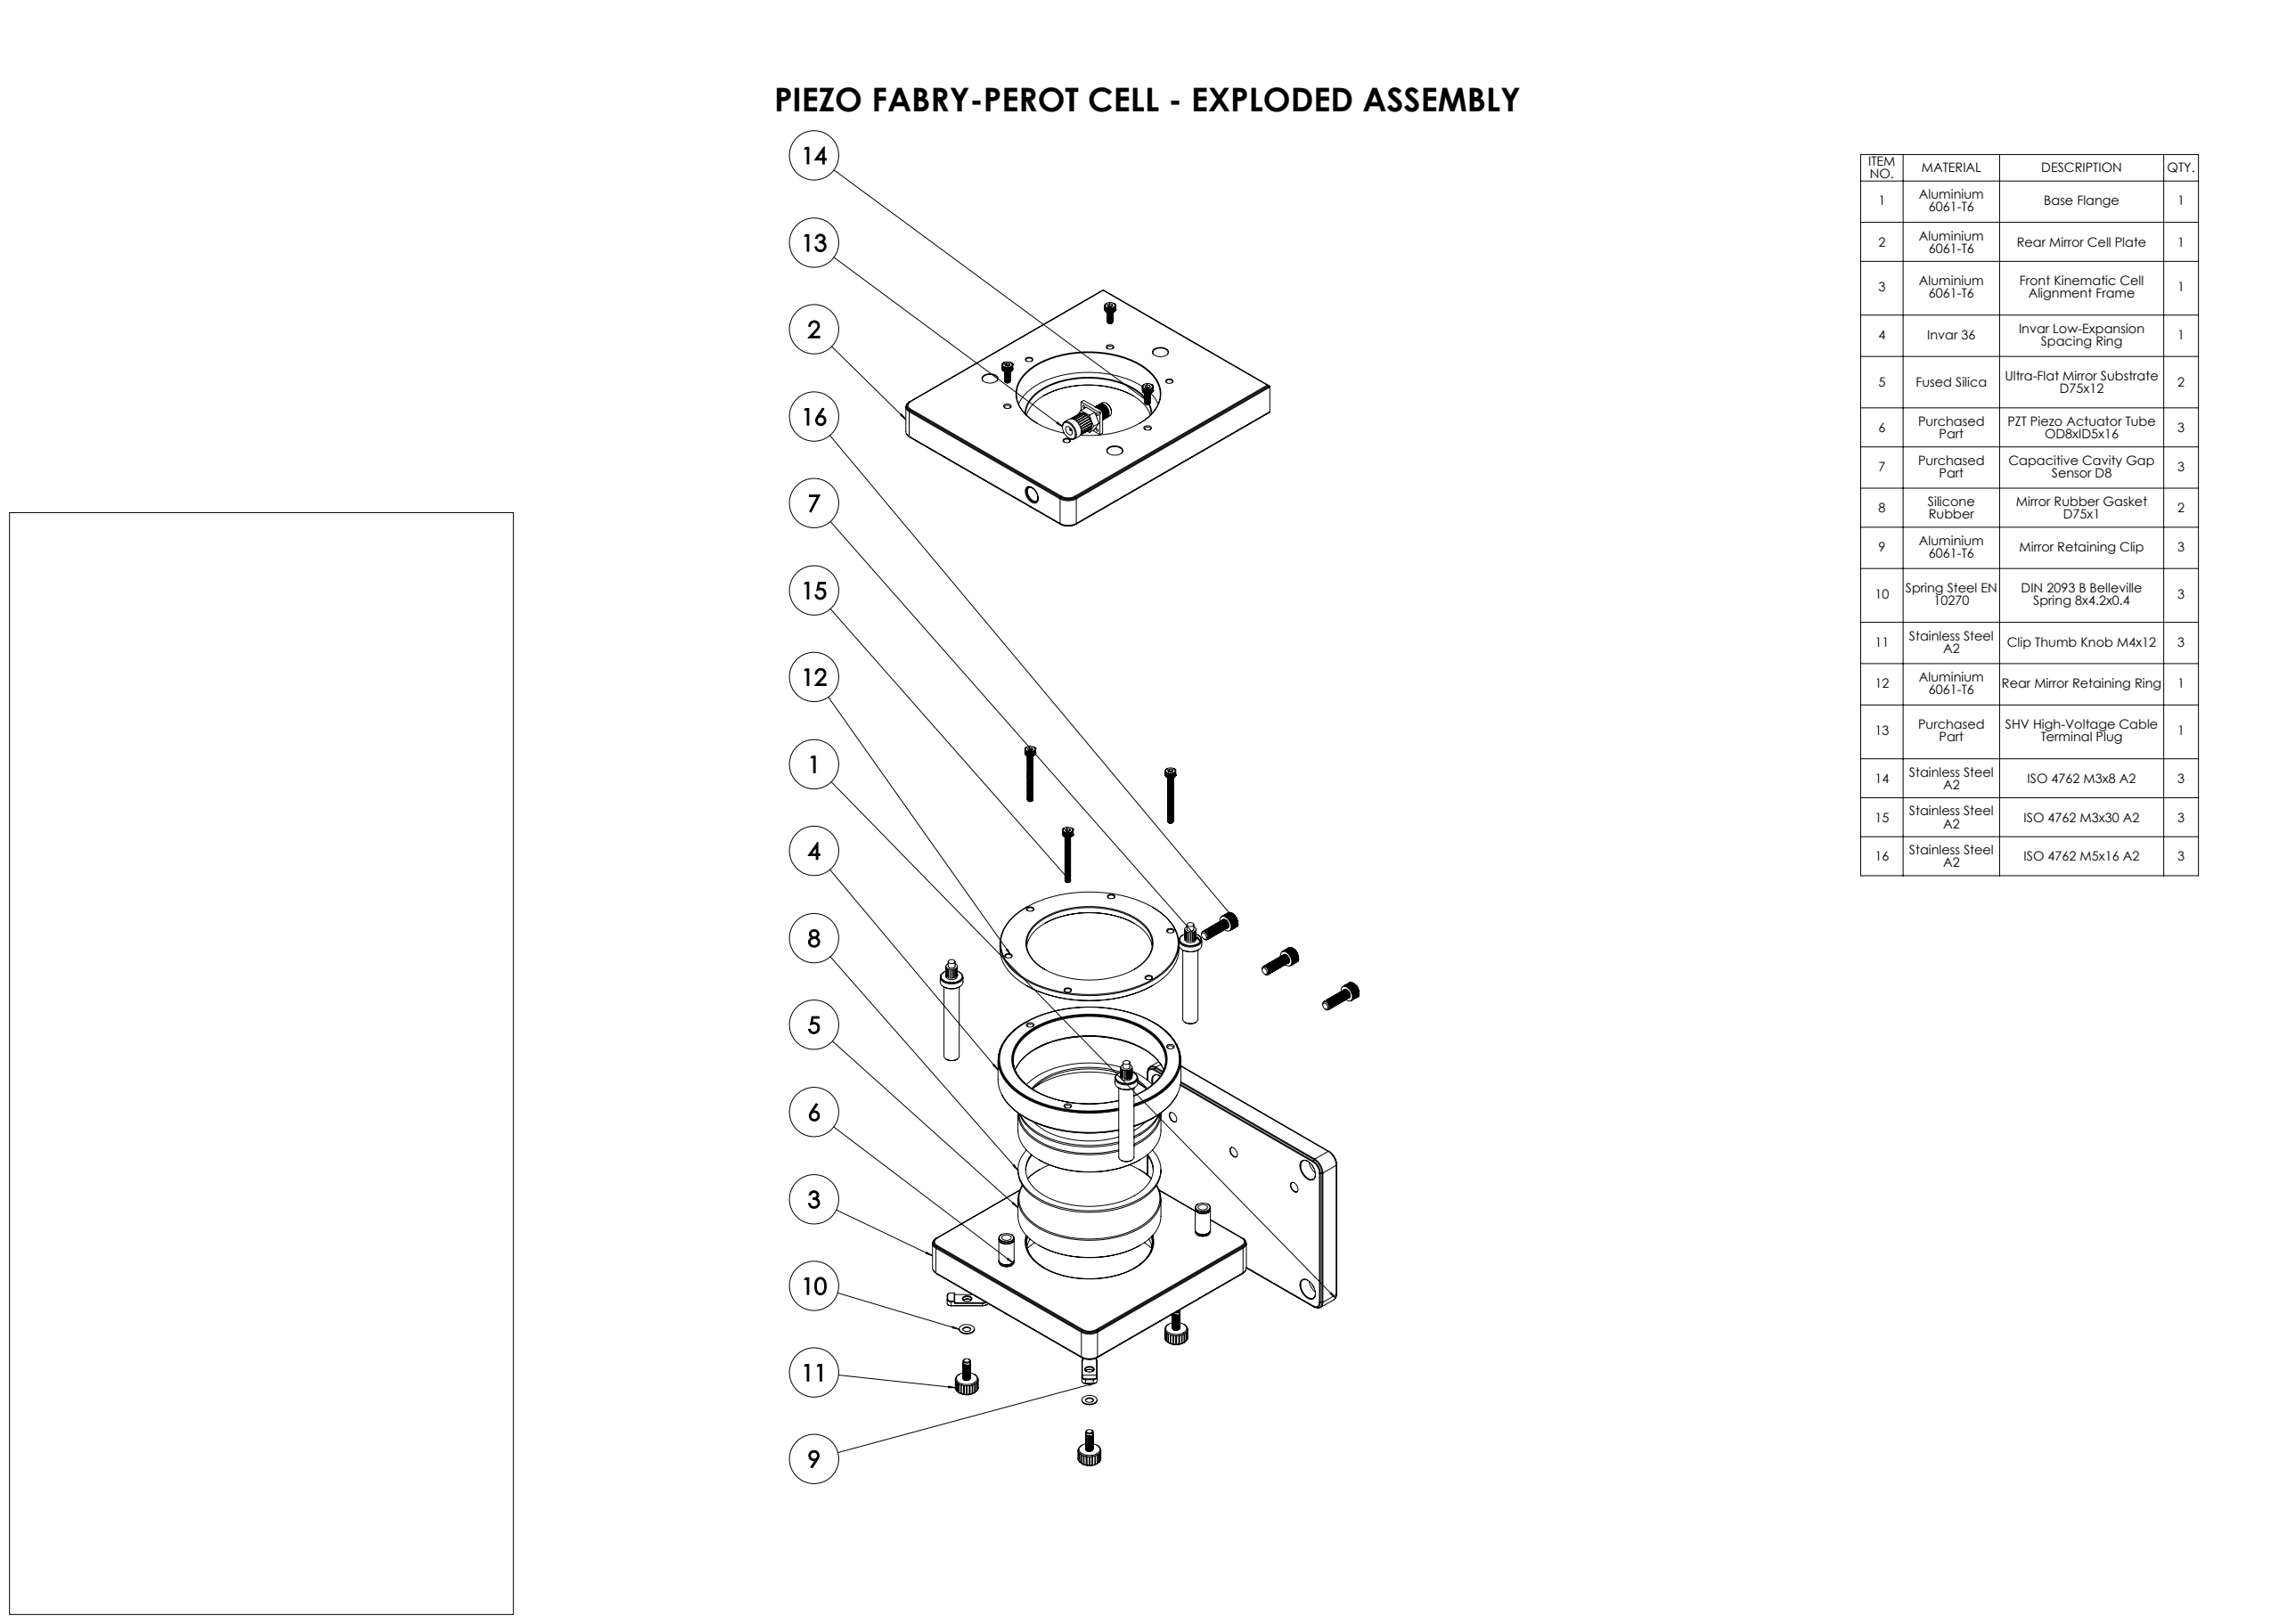
ISO-10303-21;
HEADER;
/* Generated by software containing ST-Developer
 * from STEP Tools, Inc. (www.steptools.com) 
 */

FILE_DESCRIPTION(
/* description */ (''),
/* implementation_level */ '2;1');

FILE_NAME(
/* name */ 'MAS-298',
/* time_stamp */ '2026-10-19T22:59:19-07:00',
/* author */ (''),
/* organization */ (''),
/* preprocessor_version */ 'ST-DEVELOPER v20.2',
/* originating_system */ 'Autodesk Translation Framework v15.15.0.0',
/* authorisation */ '');

FILE_SCHEMA (('AUTOMOTIVE_DESIGN { 1 0 10303 214 3 1 1 }'));
ENDSEC;

DATA;
#10=MECHANICAL_DESIGN_GEOMETRIC_PRESENTATION_REPRESENTATION('',(#911,#912,
#913,#914,#915,#916,#917,#918,#919,#920,#921,#922,#923,#924,#925,#926),
#53650);
#11=ITEM_DEFINED_TRANSFORMATION($,$,#23497,#25620);
#12=ITEM_DEFINED_TRANSFORMATION($,$,#23686,#25621);
#13=ITEM_DEFINED_TRANSFORMATION($,$,#23856,#25622);
#14=ITEM_DEFINED_TRANSFORMATION($,$,#23983,#25623);
#15=ITEM_DEFINED_TRANSFORMATION($,$,#24331,#25624);
#16=ITEM_DEFINED_TRANSFORMATION($,$,#24343,#25625);
#17=ITEM_DEFINED_TRANSFORMATION($,$,#24374,#25626);
#18=ITEM_DEFINED_TRANSFORMATION($,$,#24521,#25627);
#19=ITEM_DEFINED_TRANSFORMATION($,$,#24530,#25628);
#20=ITEM_DEFINED_TRANSFORMATION($,$,#24586,#25629);
#21=ITEM_DEFINED_TRANSFORMATION($,$,#24595,#25630);
#22=ITEM_DEFINED_TRANSFORMATION($,$,#24038,#25631);
#23=ITEM_DEFINED_TRANSFORMATION($,$,#24107,#25632);
#24=ITEM_DEFINED_TRANSFORMATION($,$,#24795,#25633);
#25=ITEM_DEFINED_TRANSFORMATION($,$,#25038,#25634);
#26=ITEM_DEFINED_TRANSFORMATION($,$,#25369,#25635);
#27=ITEM_DEFINED_TRANSFORMATION($,$,#24331,#25636);
#28=ITEM_DEFINED_TRANSFORMATION($,$,#24343,#25637);
#29=ITEM_DEFINED_TRANSFORMATION($,$,#24343,#25638);
#30=ITEM_DEFINED_TRANSFORMATION($,$,#24374,#25639);
#31=ITEM_DEFINED_TRANSFORMATION($,$,#24374,#25640);
#32=ITEM_DEFINED_TRANSFORMATION($,$,#24521,#25641);
#33=ITEM_DEFINED_TRANSFORMATION($,$,#24530,#25642);
#34=ITEM_DEFINED_TRANSFORMATION($,$,#24530,#25643);
#35=ITEM_DEFINED_TRANSFORMATION($,$,#24586,#25644);
#36=ITEM_DEFINED_TRANSFORMATION($,$,#24586,#25645);
#37=ITEM_DEFINED_TRANSFORMATION($,$,#24595,#25646);
#38=ITEM_DEFINED_TRANSFORMATION($,$,#24595,#25647);
#39=ITEM_DEFINED_TRANSFORMATION($,$,#24795,#25648);
#40=ITEM_DEFINED_TRANSFORMATION($,$,#24795,#25649);
#41=ITEM_DEFINED_TRANSFORMATION($,$,#25038,#25650);
#42=ITEM_DEFINED_TRANSFORMATION($,$,#25038,#25651);
#43=ITEM_DEFINED_TRANSFORMATION($,$,#25369,#25652);
#44=ITEM_DEFINED_TRANSFORMATION($,$,#25369,#25653);
#45=(
REPRESENTATION_RELATIONSHIP($,$,#53724,#53723)
REPRESENTATION_RELATIONSHIP_WITH_TRANSFORMATION(#11)
SHAPE_REPRESENTATION_RELATIONSHIP()
);
#46=(
REPRESENTATION_RELATIONSHIP($,$,#53725,#53723)
REPRESENTATION_RELATIONSHIP_WITH_TRANSFORMATION(#12)
SHAPE_REPRESENTATION_RELATIONSHIP()
);
#47=(
REPRESENTATION_RELATIONSHIP($,$,#53726,#53723)
REPRESENTATION_RELATIONSHIP_WITH_TRANSFORMATION(#13)
SHAPE_REPRESENTATION_RELATIONSHIP()
);
#48=(
REPRESENTATION_RELATIONSHIP($,$,#53727,#53723)
REPRESENTATION_RELATIONSHIP_WITH_TRANSFORMATION(#14)
SHAPE_REPRESENTATION_RELATIONSHIP()
);
#49=(
REPRESENTATION_RELATIONSHIP($,$,#53730,#53723)
REPRESENTATION_RELATIONSHIP_WITH_TRANSFORMATION(#15)
SHAPE_REPRESENTATION_RELATIONSHIP()
);
#50=(
REPRESENTATION_RELATIONSHIP($,$,#53731,#53723)
REPRESENTATION_RELATIONSHIP_WITH_TRANSFORMATION(#16)
SHAPE_REPRESENTATION_RELATIONSHIP()
);
#51=(
REPRESENTATION_RELATIONSHIP($,$,#53732,#53723)
REPRESENTATION_RELATIONSHIP_WITH_TRANSFORMATION(#17)
SHAPE_REPRESENTATION_RELATIONSHIP()
);
#52=(
REPRESENTATION_RELATIONSHIP($,$,#53733,#53723)
REPRESENTATION_RELATIONSHIP_WITH_TRANSFORMATION(#18)
SHAPE_REPRESENTATION_RELATIONSHIP()
);
#53=(
REPRESENTATION_RELATIONSHIP($,$,#53734,#53723)
REPRESENTATION_RELATIONSHIP_WITH_TRANSFORMATION(#19)
SHAPE_REPRESENTATION_RELATIONSHIP()
);
#54=(
REPRESENTATION_RELATIONSHIP($,$,#53735,#53723)
REPRESENTATION_RELATIONSHIP_WITH_TRANSFORMATION(#20)
SHAPE_REPRESENTATION_RELATIONSHIP()
);
#55=(
REPRESENTATION_RELATIONSHIP($,$,#53736,#53723)
REPRESENTATION_RELATIONSHIP_WITH_TRANSFORMATION(#21)
SHAPE_REPRESENTATION_RELATIONSHIP()
);
#56=(
REPRESENTATION_RELATIONSHIP($,$,#53728,#53723)
REPRESENTATION_RELATIONSHIP_WITH_TRANSFORMATION(#22)
SHAPE_REPRESENTATION_RELATIONSHIP()
);
#57=(
REPRESENTATION_RELATIONSHIP($,$,#53729,#53723)
REPRESENTATION_RELATIONSHIP_WITH_TRANSFORMATION(#23)
SHAPE_REPRESENTATION_RELATIONSHIP()
);
#58=(
REPRESENTATION_RELATIONSHIP($,$,#53737,#53723)
REPRESENTATION_RELATIONSHIP_WITH_TRANSFORMATION(#24)
SHAPE_REPRESENTATION_RELATIONSHIP()
);
#59=(
REPRESENTATION_RELATIONSHIP($,$,#53738,#53723)
REPRESENTATION_RELATIONSHIP_WITH_TRANSFORMATION(#25)
SHAPE_REPRESENTATION_RELATIONSHIP()
);
#60=(
REPRESENTATION_RELATIONSHIP($,$,#53739,#53723)
REPRESENTATION_RELATIONSHIP_WITH_TRANSFORMATION(#26)
SHAPE_REPRESENTATION_RELATIONSHIP()
);
#61=(
REPRESENTATION_RELATIONSHIP($,$,#53730,#53723)
REPRESENTATION_RELATIONSHIP_WITH_TRANSFORMATION(#27)
SHAPE_REPRESENTATION_RELATIONSHIP()
);
#62=(
REPRESENTATION_RELATIONSHIP($,$,#53731,#53723)
REPRESENTATION_RELATIONSHIP_WITH_TRANSFORMATION(#28)
SHAPE_REPRESENTATION_RELATIONSHIP()
);
#63=(
REPRESENTATION_RELATIONSHIP($,$,#53731,#53723)
REPRESENTATION_RELATIONSHIP_WITH_TRANSFORMATION(#29)
SHAPE_REPRESENTATION_RELATIONSHIP()
);
#64=(
REPRESENTATION_RELATIONSHIP($,$,#53732,#53723)
REPRESENTATION_RELATIONSHIP_WITH_TRANSFORMATION(#30)
SHAPE_REPRESENTATION_RELATIONSHIP()
);
#65=(
REPRESENTATION_RELATIONSHIP($,$,#53732,#53723)
REPRESENTATION_RELATIONSHIP_WITH_TRANSFORMATION(#31)
SHAPE_REPRESENTATION_RELATIONSHIP()
);
#66=(
REPRESENTATION_RELATIONSHIP($,$,#53733,#53723)
REPRESENTATION_RELATIONSHIP_WITH_TRANSFORMATION(#32)
SHAPE_REPRESENTATION_RELATIONSHIP()
);
#67=(
REPRESENTATION_RELATIONSHIP($,$,#53734,#53723)
REPRESENTATION_RELATIONSHIP_WITH_TRANSFORMATION(#33)
SHAPE_REPRESENTATION_RELATIONSHIP()
);
#68=(
REPRESENTATION_RELATIONSHIP($,$,#53734,#53723)
REPRESENTATION_RELATIONSHIP_WITH_TRANSFORMATION(#34)
SHAPE_REPRESENTATION_RELATIONSHIP()
);
#69=(
REPRESENTATION_RELATIONSHIP($,$,#53735,#53723)
REPRESENTATION_RELATIONSHIP_WITH_TRANSFORMATION(#35)
SHAPE_REPRESENTATION_RELATIONSHIP()
);
#70=(
REPRESENTATION_RELATIONSHIP($,$,#53735,#53723)
REPRESENTATION_RELATIONSHIP_WITH_TRANSFORMATION(#36)
SHAPE_REPRESENTATION_RELATIONSHIP()
);
#71=(
REPRESENTATION_RELATIONSHIP($,$,#53736,#53723)
REPRESENTATION_RELATIONSHIP_WITH_TRANSFORMATION(#37)
SHAPE_REPRESENTATION_RELATIONSHIP()
);
#72=(
REPRESENTATION_RELATIONSHIP($,$,#53736,#53723)
REPRESENTATION_RELATIONSHIP_WITH_TRANSFORMATION(#38)
SHAPE_REPRESENTATION_RELATIONSHIP()
);
#73=(
REPRESENTATION_RELATIONSHIP($,$,#53737,#53723)
REPRESENTATION_RELATIONSHIP_WITH_TRANSFORMATION(#39)
SHAPE_REPRESENTATION_RELATIONSHIP()
);
#74=(
REPRESENTATION_RELATIONSHIP($,$,#53737,#53723)
REPRESENTATION_RELATIONSHIP_WITH_TRANSFORMATION(#40)
SHAPE_REPRESENTATION_RELATIONSHIP()
);
#75=(
REPRESENTATION_RELATIONSHIP($,$,#53738,#53723)
REPRESENTATION_RELATIONSHIP_WITH_TRANSFORMATION(#41)
SHAPE_REPRESENTATION_RELATIONSHIP()
);
#76=(
REPRESENTATION_RELATIONSHIP($,$,#53738,#53723)
REPRESENTATION_RELATIONSHIP_WITH_TRANSFORMATION(#42)
SHAPE_REPRESENTATION_RELATIONSHIP()
);
#77=(
REPRESENTATION_RELATIONSHIP($,$,#53739,#53723)
REPRESENTATION_RELATIONSHIP_WITH_TRANSFORMATION(#43)
SHAPE_REPRESENTATION_RELATIONSHIP()
);
#78=(
REPRESENTATION_RELATIONSHIP($,$,#53739,#53723)
REPRESENTATION_RELATIONSHIP_WITH_TRANSFORMATION(#44)
SHAPE_REPRESENTATION_RELATIONSHIP()
);
#79=CONTEXT_DEPENDENT_SHAPE_REPRESENTATION(#45,#53689);
#80=CONTEXT_DEPENDENT_SHAPE_REPRESENTATION(#46,#53690);
#81=CONTEXT_DEPENDENT_SHAPE_REPRESENTATION(#47,#53691);
#82=CONTEXT_DEPENDENT_SHAPE_REPRESENTATION(#48,#53692);
#83=CONTEXT_DEPENDENT_SHAPE_REPRESENTATION(#49,#53693);
#84=CONTEXT_DEPENDENT_SHAPE_REPRESENTATION(#50,#53694);
#85=CONTEXT_DEPENDENT_SHAPE_REPRESENTATION(#51,#53695);
#86=CONTEXT_DEPENDENT_SHAPE_REPRESENTATION(#52,#53696);
#87=CONTEXT_DEPENDENT_SHAPE_REPRESENTATION(#53,#53697);
#88=CONTEXT_DEPENDENT_SHAPE_REPRESENTATION(#54,#53698);
#89=CONTEXT_DEPENDENT_SHAPE_REPRESENTATION(#55,#53699);
#90=CONTEXT_DEPENDENT_SHAPE_REPRESENTATION(#56,#53700);
#91=CONTEXT_DEPENDENT_SHAPE_REPRESENTATION(#57,#53701);
#92=CONTEXT_DEPENDENT_SHAPE_REPRESENTATION(#58,#53702);
#93=CONTEXT_DEPENDENT_SHAPE_REPRESENTATION(#59,#53703);
#94=CONTEXT_DEPENDENT_SHAPE_REPRESENTATION(#60,#53704);
#95=CONTEXT_DEPENDENT_SHAPE_REPRESENTATION(#61,#53705);
#96=CONTEXT_DEPENDENT_SHAPE_REPRESENTATION(#62,#53706);
#97=CONTEXT_DEPENDENT_SHAPE_REPRESENTATION(#63,#53707);
#98=CONTEXT_DEPENDENT_SHAPE_REPRESENTATION(#64,#53708);
#99=CONTEXT_DEPENDENT_SHAPE_REPRESENTATION(#65,#53709);
#100=CONTEXT_DEPENDENT_SHAPE_REPRESENTATION(#66,#53710);
#101=CONTEXT_DEPENDENT_SHAPE_REPRESENTATION(#67,#53711);
#102=CONTEXT_DEPENDENT_SHAPE_REPRESENTATION(#68,#53712);
#103=CONTEXT_DEPENDENT_SHAPE_REPRESENTATION(#69,#53713);
#104=CONTEXT_DEPENDENT_SHAPE_REPRESENTATION(#70,#53714);
#105=CONTEXT_DEPENDENT_SHAPE_REPRESENTATION(#71,#53715);
#106=CONTEXT_DEPENDENT_SHAPE_REPRESENTATION(#72,#53716);
#107=CONTEXT_DEPENDENT_SHAPE_REPRESENTATION(#73,#53717);
#108=CONTEXT_DEPENDENT_SHAPE_REPRESENTATION(#74,#53718);
#109=CONTEXT_DEPENDENT_SHAPE_REPRESENTATION(#75,#53719);
#110=CONTEXT_DEPENDENT_SHAPE_REPRESENTATION(#76,#53720);
#111=CONTEXT_DEPENDENT_SHAPE_REPRESENTATION(#77,#53721);
#112=CONTEXT_DEPENDENT_SHAPE_REPRESENTATION(#78,#53722);
#113=NEXT_ASSEMBLY_USAGE_OCCURRENCE('01_Base_Flange:1',
'01_Base_Flange:1','01_Base_Flange:1',#53741,#53742,'01_Base_Flange:1');
#114=NEXT_ASSEMBLY_USAGE_OCCURRENCE('02_Rear_Mirror_Cell_Plate:1',
'02_Rear_Mirror_Cell_Plate:1','02_Rear_Mirror_Cell_Plate:1',#53741,#53743,
'02_Rear_Mirror_Cell_Plate:1');
#115=NEXT_ASSEMBLY_USAGE_OCCURRENCE(
'03_Front_Kinematic_Cell_Alignment_Frame:1',
'03_Front_Kinematic_Cell_Alignment_Frame:1',
'03_Front_Kinematic_Cell_Alignment_Frame:1',#53741,#53744,
'03_Front_Kinematic_Cell_Alignment_Frame:1');
#116=NEXT_ASSEMBLY_USAGE_OCCURRENCE(
'04_Invar_Low-Expansion_Spacing_Ring:1',
'04_Invar_Low-Expansion_Spacing_Ring:1',
'04_Invar_Low-Expansion_Spacing_Ring:1',#53741,#53745,
'04_Invar_Low-Expansion_Spacing_Ring:1');
#117=NEXT_ASSEMBLY_USAGE_OCCURRENCE(
'05_Ultra-Flat_Mirror_Substrate_D75x12:1',
'05_Ultra-Flat_Mirror_Substrate_D75x12:1',
'05_Ultra-Flat_Mirror_Substrate_D75x12:1',#53741,#53748,
'05_Ultra-Flat_Mirror_Substrate_D75x12:1');
#118=NEXT_ASSEMBLY_USAGE_OCCURRENCE(
'06_PZT_Piezo_Actuator_Tube_OD8xID5x16:1',
'06_PZT_Piezo_Actuator_Tube_OD8xID5x16:1',
'06_PZT_Piezo_Actuator_Tube_OD8xID5x16:1',#53741,#53749,
'06_PZT_Piezo_Actuator_Tube_OD8xID5x16:1');
#119=NEXT_ASSEMBLY_USAGE_OCCURRENCE(
'07_Capacitive_Cavity_Gap_Sensor_D8:1',
'07_Capacitive_Cavity_Gap_Sensor_D8:1',
'07_Capacitive_Cavity_Gap_Sensor_D8:1',#53741,#53750,
'07_Capacitive_Cavity_Gap_Sensor_D8:1');
#120=NEXT_ASSEMBLY_USAGE_OCCURRENCE('08_Mirror_Rubber_Gasket_D75x1:1',
'08_Mirror_Rubber_Gasket_D75x1:1','08_Mirror_Rubber_Gasket_D75x1:1',#53741,
#53751,'08_Mirror_Rubber_Gasket_D75x1:1');
#121=NEXT_ASSEMBLY_USAGE_OCCURRENCE('09_Mirror_Retaining_Clip:1',
'09_Mirror_Retaining_Clip:1','09_Mirror_Retaining_Clip:1',#53741,#53752,
'09_Mirror_Retaining_Clip:1');
#122=NEXT_ASSEMBLY_USAGE_OCCURRENCE(
'10_DIN_2093_B_Belleville_Spring_8x4.2x0.4:1',
'10_DIN_2093_B_Belleville_Spring_8x4.2x0.4:1',
'10_DIN_2093_B_Belleville_Spring_8x4.2x0.4:1',#53741,#53753,
'10_DIN_2093_B_Belleville_Spring_8x4.2x0.4:1');
#123=NEXT_ASSEMBLY_USAGE_OCCURRENCE('11_Clip_Thumb_Knob_M4x12:1',
'11_Clip_Thumb_Knob_M4x12:1','11_Clip_Thumb_Knob_M4x12:1',#53741,#53754,
'11_Clip_Thumb_Knob_M4x12:1');
#124=NEXT_ASSEMBLY_USAGE_OCCURRENCE('12_Rear_Mirror_Retaining_Ring:1',
'12_Rear_Mirror_Retaining_Ring:1','12_Rear_Mirror_Retaining_Ring:1',#53741,
#53746,'12_Rear_Mirror_Retaining_Ring:1');
#125=NEXT_ASSEMBLY_USAGE_OCCURRENCE(
'13_SHV_High-Voltage_Cable_Terminal_Plug:1',
'13_SHV_High-Voltage_Cable_Terminal_Plug:1',
'13_SHV_High-Voltage_Cable_Terminal_Plug:1',#53741,#53747,
'13_SHV_High-Voltage_Cable_Terminal_Plug:1');
#126=NEXT_ASSEMBLY_USAGE_OCCURRENCE('14_ISO_4762_M3x8_A2:1',
'14_ISO_4762_M3x8_A2:1','14_ISO_4762_M3x8_A2:1',#53741,#53755,
'14_ISO_4762_M3x8_A2:1');
#127=NEXT_ASSEMBLY_USAGE_OCCURRENCE('15_ISO_4762_M3x30_A2:1',
'15_ISO_4762_M3x30_A2:1','15_ISO_4762_M3x30_A2:1',#53741,#53756,
'15_ISO_4762_M3x30_A2:1');
#128=NEXT_ASSEMBLY_USAGE_OCCURRENCE('16_ISO_4762_M5x16_A2:1',
'16_ISO_4762_M5x16_A2:1','16_ISO_4762_M5x16_A2:1',#53741,#53757,
'16_ISO_4762_M5x16_A2:1');
#129=NEXT_ASSEMBLY_USAGE_OCCURRENCE(
'05_Ultra-Flat_Mirror_Substrate_D75x12:2',
'05_Ultra-Flat_Mirror_Substrate_D75x12:2',
'05_Ultra-Flat_Mirror_Substrate_D75x12:2',#53741,#53748,
'05_Ultra-Flat_Mirror_Substrate_D75x12:2');
#130=NEXT_ASSEMBLY_USAGE_OCCURRENCE(
'06_PZT_Piezo_Actuator_Tube_OD8xID5x16:2',
'06_PZT_Piezo_Actuator_Tube_OD8xID5x16:2',
'06_PZT_Piezo_Actuator_Tube_OD8xID5x16:2',#53741,#53749,
'06_PZT_Piezo_Actuator_Tube_OD8xID5x16:2');
#131=NEXT_ASSEMBLY_USAGE_OCCURRENCE(
'06_PZT_Piezo_Actuator_Tube_OD8xID5x16:3',
'06_PZT_Piezo_Actuator_Tube_OD8xID5x16:3',
'06_PZT_Piezo_Actuator_Tube_OD8xID5x16:3',#53741,#53749,
'06_PZT_Piezo_Actuator_Tube_OD8xID5x16:3');
#132=NEXT_ASSEMBLY_USAGE_OCCURRENCE(
'07_Capacitive_Cavity_Gap_Sensor_D8:2',
'07_Capacitive_Cavity_Gap_Sensor_D8:2',
'07_Capacitive_Cavity_Gap_Sensor_D8:2',#53741,#53750,
'07_Capacitive_Cavity_Gap_Sensor_D8:2');
#133=NEXT_ASSEMBLY_USAGE_OCCURRENCE(
'07_Capacitive_Cavity_Gap_Sensor_D8:3',
'07_Capacitive_Cavity_Gap_Sensor_D8:3',
'07_Capacitive_Cavity_Gap_Sensor_D8:3',#53741,#53750,
'07_Capacitive_Cavity_Gap_Sensor_D8:3');
#134=NEXT_ASSEMBLY_USAGE_OCCURRENCE('08_Mirror_Rubber_Gasket_D75x1:2',
'08_Mirror_Rubber_Gasket_D75x1:2','08_Mirror_Rubber_Gasket_D75x1:2',#53741,
#53751,'08_Mirror_Rubber_Gasket_D75x1:2');
#135=NEXT_ASSEMBLY_USAGE_OCCURRENCE('09_Mirror_Retaining_Clip:2',
'09_Mirror_Retaining_Clip:2','09_Mirror_Retaining_Clip:2',#53741,#53752,
'09_Mirror_Retaining_Clip:2');
#136=NEXT_ASSEMBLY_USAGE_OCCURRENCE('09_Mirror_Retaining_Clip:3',
'09_Mirror_Retaining_Clip:3','09_Mirror_Retaining_Clip:3',#53741,#53752,
'09_Mirror_Retaining_Clip:3');
#137=NEXT_ASSEMBLY_USAGE_OCCURRENCE(
'10_DIN_2093_B_Belleville_Spring_8x4.2x0.4:2',
'10_DIN_2093_B_Belleville_Spring_8x4.2x0.4:2',
'10_DIN_2093_B_Belleville_Spring_8x4.2x0.4:2',#53741,#53753,
'10_DIN_2093_B_Belleville_Spring_8x4.2x0.4:2');
#138=NEXT_ASSEMBLY_USAGE_OCCURRENCE(
'10_DIN_2093_B_Belleville_Spring_8x4.2x0.4:3',
'10_DIN_2093_B_Belleville_Spring_8x4.2x0.4:3',
'10_DIN_2093_B_Belleville_Spring_8x4.2x0.4:3',#53741,#53753,
'10_DIN_2093_B_Belleville_Spring_8x4.2x0.4:3');
#139=NEXT_ASSEMBLY_USAGE_OCCURRENCE('11_Clip_Thumb_Knob_M4x12:2',
'11_Clip_Thumb_Knob_M4x12:2','11_Clip_Thumb_Knob_M4x12:2',#53741,#53754,
'11_Clip_Thumb_Knob_M4x12:2');
#140=NEXT_ASSEMBLY_USAGE_OCCURRENCE('11_Clip_Thumb_Knob_M4x12:3',
'11_Clip_Thumb_Knob_M4x12:3','11_Clip_Thumb_Knob_M4x12:3',#53741,#53754,
'11_Clip_Thumb_Knob_M4x12:3');
#141=NEXT_ASSEMBLY_USAGE_OCCURRENCE('14_ISO_4762_M3x8_A2:2',
'14_ISO_4762_M3x8_A2:2','14_ISO_4762_M3x8_A2:2',#53741,#53755,
'14_ISO_4762_M3x8_A2:2');
#142=NEXT_ASSEMBLY_USAGE_OCCURRENCE('14_ISO_4762_M3x8_A2:3',
'14_ISO_4762_M3x8_A2:3','14_ISO_4762_M3x8_A2:3',#53741,#53755,
'14_ISO_4762_M3x8_A2:3');
#143=NEXT_ASSEMBLY_USAGE_OCCURRENCE('15_ISO_4762_M3x30_A2:2',
'15_ISO_4762_M3x30_A2:2','15_ISO_4762_M3x30_A2:2',#53741,#53756,
'15_ISO_4762_M3x30_A2:2');
#144=NEXT_ASSEMBLY_USAGE_OCCURRENCE('15_ISO_4762_M3x30_A2:3',
'15_ISO_4762_M3x30_A2:3','15_ISO_4762_M3x30_A2:3',#53741,#53756,
'15_ISO_4762_M3x30_A2:3');
#145=NEXT_ASSEMBLY_USAGE_OCCURRENCE('16_ISO_4762_M5x16_A2:2',
'16_ISO_4762_M5x16_A2:2','16_ISO_4762_M5x16_A2:2',#53741,#53757,
'16_ISO_4762_M5x16_A2:2');
#146=NEXT_ASSEMBLY_USAGE_OCCURRENCE('16_ISO_4762_M5x16_A2:3',
'16_ISO_4762_M5x16_A2:3','16_ISO_4762_M5x16_A2:3',#53741,#53757,
'16_ISO_4762_M5x16_A2:3');
#147=(
BOUNDED_CURVE()
B_SPLINE_CURVE(2,(#40816,#40817,#40818),.UNSPECIFIED.,.F.,.F.)
B_SPLINE_CURVE_WITH_KNOTS((3,3),(0.,0.00848409808460555),.UNSPECIFIED.)
CURVE()
GEOMETRIC_REPRESENTATION_ITEM()
RATIONAL_B_SPLINE_CURVE((1.,1.00016582969981,1.00020138402525))
REPRESENTATION_ITEM('')
);
#148=(
BOUNDED_CURVE()
B_SPLINE_CURVE(2,(#40822,#40823,#40824),.UNSPECIFIED.,.F.,.F.)
B_SPLINE_CURVE_WITH_KNOTS((3,3),(0.0131150022108642,0.0215991002954745),
 .UNSPECIFIED.)
CURVE()
GEOMETRIC_REPRESENTATION_ITEM()
RATIONAL_B_SPLINE_CURVE((1.0002013840307,1.00016582970429,1.))
REPRESENTATION_ITEM('')
);
#149=(
BOUNDED_CURVE()
B_SPLINE_CURVE(2,(#40837,#40838,#40839),.UNSPECIFIED.,.F.,.F.)
B_SPLINE_CURVE_WITH_KNOTS((3,3),(0.,0.0084840980845983),.UNSPECIFIED.)
CURVE()
GEOMETRIC_REPRESENTATION_ITEM()
RATIONAL_B_SPLINE_CURVE((1.,1.00016582970166,1.00020138402749))
REPRESENTATION_ITEM('')
);
#150=(
BOUNDED_CURVE()
B_SPLINE_CURVE(2,(#40843,#40844,#40845),.UNSPECIFIED.,.F.,.F.)
B_SPLINE_CURVE_WITH_KNOTS((3,3),(0.0131150022108621,0.0215991002954745),
 .UNSPECIFIED.)
CURVE()
GEOMETRIC_REPRESENTATION_ITEM()
RATIONAL_B_SPLINE_CURVE((1.00020138404061,1.00016582971246,1.))
REPRESENTATION_ITEM('')
);
#151=(
BOUNDED_CURVE()
B_SPLINE_CURVE(2,(#40858,#40859,#40860),.UNSPECIFIED.,.F.,.F.)
B_SPLINE_CURVE_WITH_KNOTS((3,3),(0.,0.0084840980847528),.UNSPECIFIED.)
CURVE()
GEOMETRIC_REPRESENTATION_ITEM()
RATIONAL_B_SPLINE_CURVE((1.,1.00016582970549,1.00020138403215))
REPRESENTATION_ITEM('')
);
#152=(
BOUNDED_CURVE()
B_SPLINE_CURVE(2,(#40864,#40865,#40866),.UNSPECIFIED.,.F.,.F.)
B_SPLINE_CURVE_WITH_KNOTS((3,3),(0.0131150022108369,0.0215991002954744),
 .UNSPECIFIED.)
CURVE()
GEOMETRIC_REPRESENTATION_ITEM()
RATIONAL_B_SPLINE_CURVE((1.00020138403309,1.00016582970627,1.))
REPRESENTATION_ITEM('')
);
#153=(
BOUNDED_CURVE()
B_SPLINE_CURVE(2,(#40879,#40880,#40881),.UNSPECIFIED.,.F.,.F.)
B_SPLINE_CURVE_WITH_KNOTS((3,3),(0.,0.00848409808456441),.UNSPECIFIED.)
CURVE()
GEOMETRIC_REPRESENTATION_ITEM()
RATIONAL_B_SPLINE_CURVE((1.,1.00016582971128,1.00020138403918))
REPRESENTATION_ITEM('')
);
#154=(
BOUNDED_CURVE()
B_SPLINE_CURVE(2,(#40885,#40886,#40887),.UNSPECIFIED.,.F.,.F.)
B_SPLINE_CURVE_WITH_KNOTS((3,3),(0.0131150022107445,0.0215991002954745),
 .UNSPECIFIED.)
CURVE()
GEOMETRIC_REPRESENTATION_ITEM()
RATIONAL_B_SPLINE_CURVE((1.00020138401994,1.00016582969544,1.))
REPRESENTATION_ITEM('')
);
#155=(
BOUNDED_CURVE()
B_SPLINE_CURVE(2,(#40900,#40901,#40902),.UNSPECIFIED.,.F.,.F.)
B_SPLINE_CURVE_WITH_KNOTS((3,3),(0.,0.00848409808454028),.UNSPECIFIED.)
CURVE()
GEOMETRIC_REPRESENTATION_ITEM()
RATIONAL_B_SPLINE_CURVE((1.,1.00016582970383,1.00020138403013))
REPRESENTATION_ITEM('')
);
#156=(
BOUNDED_CURVE()
B_SPLINE_CURVE(2,(#40906,#40907,#40908),.UNSPECIFIED.,.F.,.F.)
B_SPLINE_CURVE_WITH_KNOTS((3,3),(0.0131150022108609,0.0215991002954744),
 .UNSPECIFIED.)
CURVE()
GEOMETRIC_REPRESENTATION_ITEM()
RATIONAL_B_SPLINE_CURVE((1.00020138403313,1.0001658297063,1.))
REPRESENTATION_ITEM('')
);
#157=(
BOUNDED_CURVE()
B_SPLINE_CURVE(2,(#40921,#40922,#40923),.UNSPECIFIED.,.F.,.F.)
B_SPLINE_CURVE_WITH_KNOTS((3,3),(0.,0.00848409808447202),.UNSPECIFIED.)
CURVE()
GEOMETRIC_REPRESENTATION_ITEM()
RATIONAL_B_SPLINE_CURVE((1.,1.00016582970768,1.00020138403481))
REPRESENTATION_ITEM('')
);
#158=(
BOUNDED_CURVE()
B_SPLINE_CURVE(2,(#40927,#40928,#40929),.UNSPECIFIED.,.F.,.F.)
B_SPLINE_CURVE_WITH_KNOTS((3,3),(0.0131150022108224,0.0215991002954744),
 .UNSPECIFIED.)
CURVE()
GEOMETRIC_REPRESENTATION_ITEM()
RATIONAL_B_SPLINE_CURVE((1.00020138403609,1.00016582970874,1.))
REPRESENTATION_ITEM('')
);
#159=(
BOUNDED_CURVE()
B_SPLINE_CURVE(2,(#40942,#40943,#40944),.UNSPECIFIED.,.F.,.F.)
B_SPLINE_CURVE_WITH_KNOTS((3,3),(0.,0.00848409808427833),.UNSPECIFIED.)
CURVE()
GEOMETRIC_REPRESENTATION_ITEM()
RATIONAL_B_SPLINE_CURVE((1.,1.00016582970634,1.00020138403319))
REPRESENTATION_ITEM('')
);
#160=(
BOUNDED_CURVE()
B_SPLINE_CURVE(2,(#40948,#40949,#40950),.UNSPECIFIED.,.F.,.F.)
B_SPLINE_CURVE_WITH_KNOTS((3,3),(0.013115002210556,0.0215991002954744),
 .UNSPECIFIED.)
CURVE()
GEOMETRIC_REPRESENTATION_ITEM()
RATIONAL_B_SPLINE_CURVE((1.00020138403007,1.00016582970378,1.))
REPRESENTATION_ITEM('')
);
#161=(
BOUNDED_CURVE()
B_SPLINE_CURVE(2,(#40963,#40964,#40965),.UNSPECIFIED.,.F.,.F.)
B_SPLINE_CURVE_WITH_KNOTS((3,3),(0.,0.00848409808441644),.UNSPECIFIED.)
CURVE()
GEOMETRIC_REPRESENTATION_ITEM()
RATIONAL_B_SPLINE_CURVE((1.,1.00016582971078,1.00020138403858))
REPRESENTATION_ITEM('')
);
#162=(
BOUNDED_CURVE()
B_SPLINE_CURVE(2,(#40969,#40970,#40971),.UNSPECIFIED.,.F.,.F.)
B_SPLINE_CURVE_WITH_KNOTS((3,3),(0.0131150022111809,0.0215991002954744),
 .UNSPECIFIED.)
CURVE()
GEOMETRIC_REPRESENTATION_ITEM()
RATIONAL_B_SPLINE_CURVE((1.00020138403856,1.00016582971077,1.))
REPRESENTATION_ITEM('')
);
#163=(
BOUNDED_CURVE()
B_SPLINE_CURVE(2,(#40984,#40985,#40986),.UNSPECIFIED.,.F.,.F.)
B_SPLINE_CURVE_WITH_KNOTS((3,3),(0.,0.00848409808461716),.UNSPECIFIED.)
CURVE()
GEOMETRIC_REPRESENTATION_ITEM()
RATIONAL_B_SPLINE_CURVE((1.,1.00016582970495,1.00020138403149))
REPRESENTATION_ITEM('')
);
#164=(
BOUNDED_CURVE()
B_SPLINE_CURVE(2,(#40990,#40991,#40992),.UNSPECIFIED.,.F.,.F.)
B_SPLINE_CURVE_WITH_KNOTS((3,3),(0.0131150022109262,0.0215991002954744),
 .UNSPECIFIED.)
CURVE()
GEOMETRIC_REPRESENTATION_ITEM()
RATIONAL_B_SPLINE_CURVE((1.00020138404239,1.00016582971392,1.))
REPRESENTATION_ITEM('')
);
#165=(
BOUNDED_CURVE()
B_SPLINE_CURVE(2,(#41005,#41006,#41007),.UNSPECIFIED.,.F.,.F.)
B_SPLINE_CURVE_WITH_KNOTS((3,3),(0.,0.00848409808431464),.UNSPECIFIED.)
CURVE()
GEOMETRIC_REPRESENTATION_ITEM()
RATIONAL_B_SPLINE_CURVE((1.,1.00016582970871,1.00020138403606))
REPRESENTATION_ITEM('')
);
#166=(
BOUNDED_CURVE()
B_SPLINE_CURVE(2,(#41011,#41012,#41013),.UNSPECIFIED.,.F.,.F.)
B_SPLINE_CURVE_WITH_KNOTS((3,3),(0.0131150022106601,0.0215991002954745),
 .UNSPECIFIED.)
CURVE()
GEOMETRIC_REPRESENTATION_ITEM()
RATIONAL_B_SPLINE_CURVE((1.00020138402617,1.00016582970057,1.))
REPRESENTATION_ITEM('')
);
#167=(
BOUNDED_CURVE()
B_SPLINE_CURVE(2,(#41026,#41027,#41028),.UNSPECIFIED.,.F.,.F.)
B_SPLINE_CURVE_WITH_KNOTS((3,3),(0.,0.00848409808479875),.UNSPECIFIED.)
CURVE()
GEOMETRIC_REPRESENTATION_ITEM()
RATIONAL_B_SPLINE_CURVE((1.,1.00016582970535,1.00020138403197))
REPRESENTATION_ITEM('')
);
#168=(
BOUNDED_CURVE()
B_SPLINE_CURVE(2,(#41032,#41033,#41034),.UNSPECIFIED.,.F.,.F.)
B_SPLINE_CURVE_WITH_KNOTS((3,3),(0.0131150022108306,0.0215991002954744),
 .UNSPECIFIED.)
CURVE()
GEOMETRIC_REPRESENTATION_ITEM()
RATIONAL_B_SPLINE_CURVE((1.00020138403405,1.00016582970706,1.))
REPRESENTATION_ITEM('')
);
#169=(
BOUNDED_CURVE()
B_SPLINE_CURVE(2,(#41047,#41048,#41049),.UNSPECIFIED.,.F.,.F.)
B_SPLINE_CURVE_WITH_KNOTS((3,3),(0.,0.0084840980847528),.UNSPECIFIED.)
CURVE()
GEOMETRIC_REPRESENTATION_ITEM()
RATIONAL_B_SPLINE_CURVE((1.,1.00016582970549,1.00020138403215))
REPRESENTATION_ITEM('')
);
#170=(
BOUNDED_CURVE()
B_SPLINE_CURVE(2,(#41053,#41054,#41055),.UNSPECIFIED.,.F.,.F.)
B_SPLINE_CURVE_WITH_KNOTS((3,3),(0.0131150022108369,0.0215991002954744),
 .UNSPECIFIED.)
CURVE()
GEOMETRIC_REPRESENTATION_ITEM()
RATIONAL_B_SPLINE_CURVE((1.00020138403309,1.00016582970627,1.))
REPRESENTATION_ITEM('')
);
#171=(
BOUNDED_CURVE()
B_SPLINE_CURVE(2,(#41068,#41069,#41070),.UNSPECIFIED.,.F.,.F.)
B_SPLINE_CURVE_WITH_KNOTS((3,3),(0.,0.0084840980842322),.UNSPECIFIED.)
CURVE()
GEOMETRIC_REPRESENTATION_ITEM()
RATIONAL_B_SPLINE_CURVE((1.,1.00016582971394,1.00020138404241))
REPRESENTATION_ITEM('')
);
#172=(
BOUNDED_CURVE()
B_SPLINE_CURVE(2,(#41074,#41075,#41076),.UNSPECIFIED.,.F.,.F.)
B_SPLINE_CURVE_WITH_KNOTS((3,3),(0.0131150022105481,0.0215991002954744),
 .UNSPECIFIED.)
CURVE()
GEOMETRIC_REPRESENTATION_ITEM()
RATIONAL_B_SPLINE_CURVE((1.00020138402709,1.00016582970133,1.))
REPRESENTATION_ITEM('')
);
#173=(
BOUNDED_CURVE()
B_SPLINE_CURVE(2,(#41089,#41090,#41091),.UNSPECIFIED.,.F.,.F.)
B_SPLINE_CURVE_WITH_KNOTS((3,3),(0.,0.00848409808414784),.UNSPECIFIED.)
CURVE()
GEOMETRIC_REPRESENTATION_ITEM()
RATIONAL_B_SPLINE_CURVE((1.,1.00016582970969,1.00020138403725))
REPRESENTATION_ITEM('')
);
#174=(
BOUNDED_CURVE()
B_SPLINE_CURVE(2,(#41095,#41096,#41097),.UNSPECIFIED.,.F.,.F.)
B_SPLINE_CURVE_WITH_KNOTS((3,3),(0.0131150022106295,0.0215991002954744),
 .UNSPECIFIED.)
CURVE()
GEOMETRIC_REPRESENTATION_ITEM()
RATIONAL_B_SPLINE_CURVE((1.00020138402686,1.00016582970114,1.))
REPRESENTATION_ITEM('')
);
#175=(
BOUNDED_CURVE()
B_SPLINE_CURVE(2,(#41110,#41111,#41112),.UNSPECIFIED.,.F.,.F.)
B_SPLINE_CURVE_WITH_KNOTS((3,3),(0.,0.00848409808445945),.UNSPECIFIED.)
CURVE()
GEOMETRIC_REPRESENTATION_ITEM()
RATIONAL_B_SPLINE_CURVE((1.,1.00016582971029,1.00020138403798))
REPRESENTATION_ITEM('')
);
#176=(
BOUNDED_CURVE()
B_SPLINE_CURVE(2,(#41116,#41117,#41118),.UNSPECIFIED.,.F.,.F.)
B_SPLINE_CURVE_WITH_KNOTS((3,3),(0.0131150022108553,0.0215991002954744),
 .UNSPECIFIED.)
CURVE()
GEOMETRIC_REPRESENTATION_ITEM()
RATIONAL_B_SPLINE_CURVE((1.00020138402807,1.00016582970213,1.))
REPRESENTATION_ITEM('')
);
#177=(
BOUNDED_CURVE()
B_SPLINE_CURVE(2,(#41131,#41132,#41133),.UNSPECIFIED.,.F.,.F.)
B_SPLINE_CURVE_WITH_KNOTS((3,3),(0.,0.00848409808448244),.UNSPECIFIED.)
CURVE()
GEOMETRIC_REPRESENTATION_ITEM()
RATIONAL_B_SPLINE_CURVE((1.,1.00016582970044,1.00020138402602))
REPRESENTATION_ITEM('')
);
#178=(
BOUNDED_CURVE()
B_SPLINE_CURVE(2,(#41137,#41138,#41139),.UNSPECIFIED.,.F.,.F.)
B_SPLINE_CURVE_WITH_KNOTS((3,3),(0.0131150022107,0.0215991002954745),
 .UNSPECIFIED.)
CURVE()
GEOMETRIC_REPRESENTATION_ITEM()
RATIONAL_B_SPLINE_CURVE((1.00020138402745,1.00016582970163,1.))
REPRESENTATION_ITEM('')
);
#179=(
BOUNDED_CURVE()
B_SPLINE_CURVE(2,(#41152,#41153,#41154),.UNSPECIFIED.,.F.,.F.)
B_SPLINE_CURVE_WITH_KNOTS((3,3),(0.,0.0084840980844404),.UNSPECIFIED.)
CURVE()
GEOMETRIC_REPRESENTATION_ITEM()
RATIONAL_B_SPLINE_CURVE((1.,1.00016582969984,1.00020138402529))
REPRESENTATION_ITEM('')
);
#180=(
BOUNDED_CURVE()
B_SPLINE_CURVE(2,(#41158,#41159,#41160),.UNSPECIFIED.,.F.,.F.)
B_SPLINE_CURVE_WITH_KNOTS((3,3),(0.0131150022109728,0.0215991002954744),
 .UNSPECIFIED.)
CURVE()
GEOMETRIC_REPRESENTATION_ITEM()
RATIONAL_B_SPLINE_CURVE((1.00020138403593,1.0001658297086,1.))
REPRESENTATION_ITEM('')
);
#181=(
BOUNDED_CURVE()
B_SPLINE_CURVE(2,(#41175,#41176,#41177),.UNSPECIFIED.,.F.,.F.)
B_SPLINE_CURVE_WITH_KNOTS((3,3),(0.,0.00848409808461716),.UNSPECIFIED.)
CURVE()
GEOMETRIC_REPRESENTATION_ITEM()
RATIONAL_B_SPLINE_CURVE((1.,1.00016582970494,1.00020138403149))
REPRESENTATION_ITEM('')
);
#182=(
BOUNDED_CURVE()
B_SPLINE_CURVE(2,(#41181,#41182,#41183),.UNSPECIFIED.,.F.,.F.)
B_SPLINE_CURVE_WITH_KNOTS((3,3),(0.0131150022107313,0.0215991002954744),
 .UNSPECIFIED.)
CURVE()
GEOMETRIC_REPRESENTATION_ITEM()
RATIONAL_B_SPLINE_CURVE((1.00020138404435,1.00016582971554,1.))
REPRESENTATION_ITEM('')
);
#183=(
BOUNDED_CURVE()
B_SPLINE_CURVE(2,(#41196,#41197,#41198),.UNSPECIFIED.,.F.,.F.)
B_SPLINE_CURVE_WITH_KNOTS((3,3),(0.,0.0084840980847339),.UNSPECIFIED.)
CURVE()
GEOMETRIC_REPRESENTATION_ITEM()
RATIONAL_B_SPLINE_CURVE((1.,1.00016582970597,1.00020138403273))
REPRESENTATION_ITEM('')
);
#184=(
BOUNDED_CURVE()
B_SPLINE_CURVE(2,(#41202,#41203,#41204),.UNSPECIFIED.,.F.,.F.)
B_SPLINE_CURVE_WITH_KNOTS((3,3),(0.0131150022106966,0.0215991002954744),
 .UNSPECIFIED.)
CURVE()
GEOMETRIC_REPRESENTATION_ITEM()
RATIONAL_B_SPLINE_CURVE((1.00020138403392,1.00016582970695,1.))
REPRESENTATION_ITEM('')
);
#185=(
BOUNDED_CURVE()
B_SPLINE_CURVE(2,(#41217,#41218,#41219),.UNSPECIFIED.,.F.,.F.)
B_SPLINE_CURVE_WITH_KNOTS((3,3),(0.,0.00848409808458664),.UNSPECIFIED.)
CURVE()
GEOMETRIC_REPRESENTATION_ITEM()
RATIONAL_B_SPLINE_CURVE((1.,1.00016582970477,1.00020138403127))
REPRESENTATION_ITEM('')
);
#186=(
BOUNDED_CURVE()
B_SPLINE_CURVE(2,(#41223,#41224,#41225),.UNSPECIFIED.,.F.,.F.)
B_SPLINE_CURVE_WITH_KNOTS((3,3),(0.0131150022108393,0.0215991002954745),
 .UNSPECIFIED.)
CURVE()
GEOMETRIC_REPRESENTATION_ITEM()
RATIONAL_B_SPLINE_CURVE((1.00020138403572,1.00016582970843,1.))
REPRESENTATION_ITEM('')
);
#187=(
BOUNDED_CURVE()
B_SPLINE_CURVE(2,(#41238,#41239,#41240),.UNSPECIFIED.,.F.,.F.)
B_SPLINE_CURVE_WITH_KNOTS((3,3),(0.,0.00848409808463718),.UNSPECIFIED.)
CURVE()
GEOMETRIC_REPRESENTATION_ITEM()
RATIONAL_B_SPLINE_CURVE((1.,1.00016582970055,1.00020138402615))
REPRESENTATION_ITEM('')
);
#188=(
BOUNDED_CURVE()
B_SPLINE_CURVE(2,(#41244,#41245,#41246),.UNSPECIFIED.,.F.,.F.)
B_SPLINE_CURVE_WITH_KNOTS((3,3),(0.013115002211021,0.0215991002954743),
 .UNSPECIFIED.)
CURVE()
GEOMETRIC_REPRESENTATION_ITEM()
RATIONAL_B_SPLINE_CURVE((1.00020138403351,1.00016582970661,1.))
REPRESENTATION_ITEM('')
);
#189=(
BOUNDED_CURVE()
B_SPLINE_CURVE(2,(#41259,#41260,#41261),.UNSPECIFIED.,.F.,.F.)
B_SPLINE_CURVE_WITH_KNOTS((3,3),(0.,0.0084840980842322),.UNSPECIFIED.)
CURVE()
GEOMETRIC_REPRESENTATION_ITEM()
RATIONAL_B_SPLINE_CURVE((1.,1.00016582971394,1.00020138404241))
REPRESENTATION_ITEM('')
);
#190=(
BOUNDED_CURVE()
B_SPLINE_CURVE(2,(#41265,#41266,#41267),.UNSPECIFIED.,.F.,.F.)
B_SPLINE_CURVE_WITH_KNOTS((3,3),(0.0131150022105481,0.0215991002954744),
 .UNSPECIFIED.)
CURVE()
GEOMETRIC_REPRESENTATION_ITEM()
RATIONAL_B_SPLINE_CURVE((1.00020138402709,1.00016582970133,1.))
REPRESENTATION_ITEM('')
);
#191=(
BOUNDED_CURVE()
B_SPLINE_CURVE(2,(#41280,#41281,#41282),.UNSPECIFIED.,.F.,.F.)
B_SPLINE_CURVE_WITH_KNOTS((3,3),(0.,0.00848409808456074),.UNSPECIFIED.)
CURVE()
GEOMETRIC_REPRESENTATION_ITEM()
RATIONAL_B_SPLINE_CURVE((1.,1.00016582970947,1.00020138403699))
REPRESENTATION_ITEM('')
);
#192=(
BOUNDED_CURVE()
B_SPLINE_CURVE(2,(#41286,#41287,#41288),.UNSPECIFIED.,.F.,.F.)
B_SPLINE_CURVE_WITH_KNOTS((3,3),(0.0131150022109338,0.0215991002954745),
 .UNSPECIFIED.)
CURVE()
GEOMETRIC_REPRESENTATION_ITEM()
RATIONAL_B_SPLINE_CURVE((1.00020138403466,1.00016582970756,1.))
REPRESENTATION_ITEM('')
);
#193=(
BOUNDED_CURVE()
B_SPLINE_CURVE(2,(#41301,#41302,#41303),.UNSPECIFIED.,.F.,.F.)
B_SPLINE_CURVE_WITH_KNOTS((3,3),(0.,0.00848409808446819),.UNSPECIFIED.)
CURVE()
GEOMETRIC_REPRESENTATION_ITEM()
RATIONAL_B_SPLINE_CURVE((1.,1.00016582970737,1.00020138403444))
REPRESENTATION_ITEM('')
);
#194=(
BOUNDED_CURVE()
B_SPLINE_CURVE(2,(#41307,#41308,#41309),.UNSPECIFIED.,.F.,.F.)
B_SPLINE_CURVE_WITH_KNOTS((3,3),(0.0131150022107308,0.0215991002954744),
 .UNSPECIFIED.)
CURVE()
GEOMETRIC_REPRESENTATION_ITEM()
RATIONAL_B_SPLINE_CURVE((1.00020138402973,1.0001658297035,1.))
REPRESENTATION_ITEM('')
);
#195=(
BOUNDED_CURVE()
B_SPLINE_CURVE(2,(#41322,#41323,#41324),.UNSPECIFIED.,.F.,.F.)
B_SPLINE_CURVE_WITH_KNOTS((3,3),(0.,0.00848409808448244),.UNSPECIFIED.)
CURVE()
GEOMETRIC_REPRESENTATION_ITEM()
RATIONAL_B_SPLINE_CURVE((1.,1.00016582970044,1.00020138402602))
REPRESENTATION_ITEM('')
);
#196=(
BOUNDED_CURVE()
B_SPLINE_CURVE(2,(#41328,#41329,#41330),.UNSPECIFIED.,.F.,.F.)
B_SPLINE_CURVE_WITH_KNOTS((3,3),(0.0131150022107,0.0215991002954745),
 .UNSPECIFIED.)
CURVE()
GEOMETRIC_REPRESENTATION_ITEM()
RATIONAL_B_SPLINE_CURVE((1.00020138402745,1.00016582970163,1.))
REPRESENTATION_ITEM('')
);
#197=(
BOUNDED_CURVE()
B_SPLINE_CURVE(2,(#41343,#41344,#41345),.UNSPECIFIED.,.F.,.F.)
B_SPLINE_CURVE_WITH_KNOTS((3,3),(0.,0.00848409808441086),.UNSPECIFIED.)
CURVE()
GEOMETRIC_REPRESENTATION_ITEM()
RATIONAL_B_SPLINE_CURVE((1.,1.00016582971069,1.00020138403846))
REPRESENTATION_ITEM('')
);
#198=(
BOUNDED_CURVE()
B_SPLINE_CURVE(2,(#41349,#41350,#41351),.UNSPECIFIED.,.F.,.F.)
B_SPLINE_CURVE_WITH_KNOTS((3,3),(0.0131150022109839,0.0215991002954745),
 .UNSPECIFIED.)
CURVE()
GEOMETRIC_REPRESENTATION_ITEM()
RATIONAL_B_SPLINE_CURVE((1.00020138402514,1.00016582969972,1.))
REPRESENTATION_ITEM('')
);
#199=(
BOUNDED_CURVE()
B_SPLINE_CURVE(2,(#41364,#41365,#41366),.UNSPECIFIED.,.F.,.F.)
B_SPLINE_CURVE_WITH_KNOTS((3,3),(0.,0.00848409808461089),.UNSPECIFIED.)
CURVE()
GEOMETRIC_REPRESENTATION_ITEM()
RATIONAL_B_SPLINE_CURVE((1.,1.00016582970996,1.00020138403757))
REPRESENTATION_ITEM('')
);
#200=(
BOUNDED_CURVE()
B_SPLINE_CURVE(2,(#41370,#41371,#41372),.UNSPECIFIED.,.F.,.F.)
B_SPLINE_CURVE_WITH_KNOTS((3,3),(0.0131150022107081,0.0215991002954744),
 .UNSPECIFIED.)
CURVE()
GEOMETRIC_REPRESENTATION_ITEM()
RATIONAL_B_SPLINE_CURVE((1.00020138403464,1.00016582970754,1.))
REPRESENTATION_ITEM('')
);
#201=(
BOUNDED_CURVE()
B_SPLINE_CURVE(2,(#41385,#41386,#41387),.UNSPECIFIED.,.F.,.F.)
B_SPLINE_CURVE_WITH_KNOTS((3,3),(0.,0.00848409808429742),.UNSPECIFIED.)
CURVE()
GEOMETRIC_REPRESENTATION_ITEM()
RATIONAL_B_SPLINE_CURVE((1.,1.00016582971405,1.00020138404255))
REPRESENTATION_ITEM('')
);
#202=(
BOUNDED_CURVE()
B_SPLINE_CURVE(2,(#41391,#41392,#41393),.UNSPECIFIED.,.F.,.F.)
B_SPLINE_CURVE_WITH_KNOTS((3,3),(0.0131150022109026,0.0215991002954744),
 .UNSPECIFIED.)
CURVE()
GEOMETRIC_REPRESENTATION_ITEM()
RATIONAL_B_SPLINE_CURVE((1.00020138403953,1.00016582971157,1.))
REPRESENTATION_ITEM('')
);
#203=(
BOUNDED_CURVE()
B_SPLINE_CURVE(2,(#41406,#41407,#41408),.UNSPECIFIED.,.F.,.F.)
B_SPLINE_CURVE_WITH_KNOTS((3,3),(0.,0.00848409808458664),.UNSPECIFIED.)
CURVE()
GEOMETRIC_REPRESENTATION_ITEM()
RATIONAL_B_SPLINE_CURVE((1.,1.00016582970477,1.00020138403127))
REPRESENTATION_ITEM('')
);
#204=(
BOUNDED_CURVE()
B_SPLINE_CURVE(2,(#41412,#41413,#41414),.UNSPECIFIED.,.F.,.F.)
B_SPLINE_CURVE_WITH_KNOTS((3,3),(0.0131150022108393,0.0215991002954745),
 .UNSPECIFIED.)
CURVE()
GEOMETRIC_REPRESENTATION_ITEM()
RATIONAL_B_SPLINE_CURVE((1.00020138403572,1.00016582970843,1.))
REPRESENTATION_ITEM('')
);
#205=(
BOUNDED_CURVE()
B_SPLINE_CURVE(2,(#41427,#41428,#41429),.UNSPECIFIED.,.F.,.F.)
B_SPLINE_CURVE_WITH_KNOTS((3,3),(0.,0.00848409808472772),.UNSPECIFIED.)
CURVE()
GEOMETRIC_REPRESENTATION_ITEM()
RATIONAL_B_SPLINE_CURVE((1.,1.00016582970133,1.0002013840271))
REPRESENTATION_ITEM('')
);
#206=(
BOUNDED_CURVE()
B_SPLINE_CURVE(2,(#41433,#41434,#41435),.UNSPECIFIED.,.F.,.F.)
B_SPLINE_CURVE_WITH_KNOTS((3,3),(0.0131150022106421,0.0215991002954744),
 .UNSPECIFIED.)
CURVE()
GEOMETRIC_REPRESENTATION_ITEM()
RATIONAL_B_SPLINE_CURVE((1.00020138403214,1.00016582970549,1.))
REPRESENTATION_ITEM('')
);
#207=(
BOUNDED_CURVE()
B_SPLINE_CURVE(2,(#41448,#41449,#41450),.UNSPECIFIED.,.F.,.F.)
B_SPLINE_CURVE_WITH_KNOTS((3,3),(0.,0.00848409808461495),.UNSPECIFIED.)
CURVE()
GEOMETRIC_REPRESENTATION_ITEM()
RATIONAL_B_SPLINE_CURVE((1.,1.00016582970949,1.000201384037))
REPRESENTATION_ITEM('')
);
#208=(
BOUNDED_CURVE()
B_SPLINE_CURVE(2,(#41454,#41455,#41456),.UNSPECIFIED.,.F.,.F.)
B_SPLINE_CURVE_WITH_KNOTS((3,3),(0.0131150022109445,0.0215991002954744),
 .UNSPECIFIED.)
CURVE()
GEOMETRIC_REPRESENTATION_ITEM()
RATIONAL_B_SPLINE_CURVE((1.00020138402523,1.00016582969979,1.))
REPRESENTATION_ITEM('')
);
#209=(
BOUNDED_CURVE()
B_SPLINE_CURVE(2,(#41469,#41470,#41471),.UNSPECIFIED.,.F.,.F.)
B_SPLINE_CURVE_WITH_KNOTS((3,3),(0.,0.00848409808414784),.UNSPECIFIED.)
CURVE()
GEOMETRIC_REPRESENTATION_ITEM()
RATIONAL_B_SPLINE_CURVE((1.,1.00016582970969,1.00020138403725))
REPRESENTATION_ITEM('')
);
#210=(
BOUNDED_CURVE()
B_SPLINE_CURVE(2,(#41475,#41476,#41477),.UNSPECIFIED.,.F.,.F.)
B_SPLINE_CURVE_WITH_KNOTS((3,3),(0.0131150022106295,0.0215991002954744),
 .UNSPECIFIED.)
CURVE()
GEOMETRIC_REPRESENTATION_ITEM()
RATIONAL_B_SPLINE_CURVE((1.00020138402686,1.00016582970114,1.))
REPRESENTATION_ITEM('')
);
#211=(
BOUNDED_CURVE()
B_SPLINE_CURVE(2,(#41490,#41491,#41492),.UNSPECIFIED.,.F.,.F.)
B_SPLINE_CURVE_WITH_KNOTS((3,3),(0.,0.00848409808467215),.UNSPECIFIED.)
CURVE()
GEOMETRIC_REPRESENTATION_ITEM()
RATIONAL_B_SPLINE_CURVE((1.,1.00016582970831,1.00020138403558))
REPRESENTATION_ITEM('')
);
#212=(
BOUNDED_CURVE()
B_SPLINE_CURVE(2,(#41496,#41497,#41498),.UNSPECIFIED.,.F.,.F.)
B_SPLINE_CURVE_WITH_KNOTS((3,3),(0.0131150022106657,0.0215991002954744),
 .UNSPECIFIED.)
CURVE()
GEOMETRIC_REPRESENTATION_ITEM()
RATIONAL_B_SPLINE_CURVE((1.00020138402665,1.00016582970096,1.))
REPRESENTATION_ITEM('')
);
#213=(
BOUNDED_CURVE()
B_SPLINE_CURVE(2,(#41511,#41512,#41513),.UNSPECIFIED.,.F.,.F.)
B_SPLINE_CURVE_WITH_KNOTS((3,3),(0.,0.00848409808448244),.UNSPECIFIED.)
CURVE()
GEOMETRIC_REPRESENTATION_ITEM()
RATIONAL_B_SPLINE_CURVE((1.,1.00016582970044,1.00020138402602))
REPRESENTATION_ITEM('')
);
#214=(
BOUNDED_CURVE()
B_SPLINE_CURVE(2,(#41517,#41518,#41519),.UNSPECIFIED.,.F.,.F.)
B_SPLINE_CURVE_WITH_KNOTS((3,3),(0.0131150022107,0.0215991002954745),
 .UNSPECIFIED.)
CURVE()
GEOMETRIC_REPRESENTATION_ITEM()
RATIONAL_B_SPLINE_CURVE((1.00020138402745,1.00016582970163,1.))
REPRESENTATION_ITEM('')
);
#215=(
BOUNDED_CURVE()
B_SPLINE_CURVE(2,(#41532,#41533,#41534),.UNSPECIFIED.,.F.,.F.)
B_SPLINE_CURVE_WITH_KNOTS((3,3),(0.,0.00848409808462521),.UNSPECIFIED.)
CURVE()
GEOMETRIC_REPRESENTATION_ITEM()
RATIONAL_B_SPLINE_CURVE((1.,1.00016582970203,1.00020138402795))
REPRESENTATION_ITEM('')
);
#216=(
BOUNDED_CURVE()
B_SPLINE_CURVE(2,(#41538,#41539,#41540),.UNSPECIFIED.,.F.,.F.)
B_SPLINE_CURVE_WITH_KNOTS((3,3),(0.0131150022109901,0.0215991002954744),
 .UNSPECIFIED.)
CURVE()
GEOMETRIC_REPRESENTATION_ITEM()
RATIONAL_B_SPLINE_CURVE((1.00020138403892,1.00016582971107,1.))
REPRESENTATION_ITEM('')
);
#217=(
BOUNDED_CURVE()
B_SPLINE_CURVE(2,(#41593,#41594,#41595),.UNSPECIFIED.,.F.,.F.)
B_SPLINE_CURVE_WITH_KNOTS((3,3),(0.,0.0084840980844225),.UNSPECIFIED.)
CURVE()
GEOMETRIC_REPRESENTATION_ITEM()
RATIONAL_B_SPLINE_CURVE((1.,1.00016582970633,1.00020138403317))
REPRESENTATION_ITEM('')
);
#218=(
BOUNDED_CURVE()
B_SPLINE_CURVE(2,(#41597,#41598,#41599),.UNSPECIFIED.,.F.,.F.)
B_SPLINE_CURVE_WITH_KNOTS((3,3),(0.0131150022108769,0.0215991002954744),
 .UNSPECIFIED.)
CURVE()
GEOMETRIC_REPRESENTATION_ITEM()
RATIONAL_B_SPLINE_CURVE((1.00020138402781,1.00016582970192,1.))
REPRESENTATION_ITEM('')
);
#219=(
BOUNDED_CURVE()
B_SPLINE_CURVE(2,(#49244,#49245,#49246),.UNSPECIFIED.,.F.,.F.)
B_SPLINE_CURVE_WITH_KNOTS((3,3),(0.,0.00848409808460555),.UNSPECIFIED.)
CURVE()
GEOMETRIC_REPRESENTATION_ITEM()
RATIONAL_B_SPLINE_CURVE((1.,1.00016582969981,1.00020138402525))
REPRESENTATION_ITEM('')
);
#220=(
BOUNDED_CURVE()
B_SPLINE_CURVE(2,(#49250,#49251,#49252),.UNSPECIFIED.,.F.,.F.)
B_SPLINE_CURVE_WITH_KNOTS((3,3),(0.0131150022108642,0.0215991002954745),
 .UNSPECIFIED.)
CURVE()
GEOMETRIC_REPRESENTATION_ITEM()
RATIONAL_B_SPLINE_CURVE((1.0002013840307,1.00016582970429,1.))
REPRESENTATION_ITEM('')
);
#221=(
BOUNDED_CURVE()
B_SPLINE_CURVE(2,(#49265,#49266,#49267),.UNSPECIFIED.,.F.,.F.)
B_SPLINE_CURVE_WITH_KNOTS((3,3),(0.,0.0084840980845983),.UNSPECIFIED.)
CURVE()
GEOMETRIC_REPRESENTATION_ITEM()
RATIONAL_B_SPLINE_CURVE((1.,1.00016582970166,1.00020138402749))
REPRESENTATION_ITEM('')
);
#222=(
BOUNDED_CURVE()
B_SPLINE_CURVE(2,(#49271,#49272,#49273),.UNSPECIFIED.,.F.,.F.)
B_SPLINE_CURVE_WITH_KNOTS((3,3),(0.0131150022108621,0.0215991002954745),
 .UNSPECIFIED.)
CURVE()
GEOMETRIC_REPRESENTATION_ITEM()
RATIONAL_B_SPLINE_CURVE((1.00020138404061,1.00016582971246,1.))
REPRESENTATION_ITEM('')
);
#223=(
BOUNDED_CURVE()
B_SPLINE_CURVE(2,(#49286,#49287,#49288),.UNSPECIFIED.,.F.,.F.)
B_SPLINE_CURVE_WITH_KNOTS((3,3),(0.,0.0084840980847528),.UNSPECIFIED.)
CURVE()
GEOMETRIC_REPRESENTATION_ITEM()
RATIONAL_B_SPLINE_CURVE((1.,1.00016582970549,1.00020138403215))
REPRESENTATION_ITEM('')
);
#224=(
BOUNDED_CURVE()
B_SPLINE_CURVE(2,(#49292,#49293,#49294),.UNSPECIFIED.,.F.,.F.)
B_SPLINE_CURVE_WITH_KNOTS((3,3),(0.0131150022108369,0.0215991002954744),
 .UNSPECIFIED.)
CURVE()
GEOMETRIC_REPRESENTATION_ITEM()
RATIONAL_B_SPLINE_CURVE((1.00020138403309,1.00016582970627,1.))
REPRESENTATION_ITEM('')
);
#225=(
BOUNDED_CURVE()
B_SPLINE_CURVE(2,(#49307,#49308,#49309),.UNSPECIFIED.,.F.,.F.)
B_SPLINE_CURVE_WITH_KNOTS((3,3),(0.,0.00848409808456441),.UNSPECIFIED.)
CURVE()
GEOMETRIC_REPRESENTATION_ITEM()
RATIONAL_B_SPLINE_CURVE((1.,1.00016582971128,1.00020138403918))
REPRESENTATION_ITEM('')
);
#226=(
BOUNDED_CURVE()
B_SPLINE_CURVE(2,(#49313,#49314,#49315),.UNSPECIFIED.,.F.,.F.)
B_SPLINE_CURVE_WITH_KNOTS((3,3),(0.0131150022107445,0.0215991002954745),
 .UNSPECIFIED.)
CURVE()
GEOMETRIC_REPRESENTATION_ITEM()
RATIONAL_B_SPLINE_CURVE((1.00020138401994,1.00016582969544,1.))
REPRESENTATION_ITEM('')
);
#227=(
BOUNDED_CURVE()
B_SPLINE_CURVE(2,(#49328,#49329,#49330),.UNSPECIFIED.,.F.,.F.)
B_SPLINE_CURVE_WITH_KNOTS((3,3),(0.,0.00848409808454028),.UNSPECIFIED.)
CURVE()
GEOMETRIC_REPRESENTATION_ITEM()
RATIONAL_B_SPLINE_CURVE((1.,1.00016582970383,1.00020138403013))
REPRESENTATION_ITEM('')
);
#228=(
BOUNDED_CURVE()
B_SPLINE_CURVE(2,(#49334,#49335,#49336),.UNSPECIFIED.,.F.,.F.)
B_SPLINE_CURVE_WITH_KNOTS((3,3),(0.0131150022108609,0.0215991002954744),
 .UNSPECIFIED.)
CURVE()
GEOMETRIC_REPRESENTATION_ITEM()
RATIONAL_B_SPLINE_CURVE((1.00020138403313,1.0001658297063,1.))
REPRESENTATION_ITEM('')
);
#229=(
BOUNDED_CURVE()
B_SPLINE_CURVE(2,(#49349,#49350,#49351),.UNSPECIFIED.,.F.,.F.)
B_SPLINE_CURVE_WITH_KNOTS((3,3),(0.,0.00848409808447202),.UNSPECIFIED.)
CURVE()
GEOMETRIC_REPRESENTATION_ITEM()
RATIONAL_B_SPLINE_CURVE((1.,1.00016582970768,1.00020138403481))
REPRESENTATION_ITEM('')
);
#230=(
BOUNDED_CURVE()
B_SPLINE_CURVE(2,(#49355,#49356,#49357),.UNSPECIFIED.,.F.,.F.)
B_SPLINE_CURVE_WITH_KNOTS((3,3),(0.0131150022108224,0.0215991002954744),
 .UNSPECIFIED.)
CURVE()
GEOMETRIC_REPRESENTATION_ITEM()
RATIONAL_B_SPLINE_CURVE((1.00020138403609,1.00016582970874,1.))
REPRESENTATION_ITEM('')
);
#231=(
BOUNDED_CURVE()
B_SPLINE_CURVE(2,(#49370,#49371,#49372),.UNSPECIFIED.,.F.,.F.)
B_SPLINE_CURVE_WITH_KNOTS((3,3),(0.,0.00848409808427833),.UNSPECIFIED.)
CURVE()
GEOMETRIC_REPRESENTATION_ITEM()
RATIONAL_B_SPLINE_CURVE((1.,1.00016582970634,1.00020138403319))
REPRESENTATION_ITEM('')
);
#232=(
BOUNDED_CURVE()
B_SPLINE_CURVE(2,(#49376,#49377,#49378),.UNSPECIFIED.,.F.,.F.)
B_SPLINE_CURVE_WITH_KNOTS((3,3),(0.013115002210556,0.0215991002954744),
 .UNSPECIFIED.)
CURVE()
GEOMETRIC_REPRESENTATION_ITEM()
RATIONAL_B_SPLINE_CURVE((1.00020138403007,1.00016582970378,1.))
REPRESENTATION_ITEM('')
);
#233=(
BOUNDED_CURVE()
B_SPLINE_CURVE(2,(#49391,#49392,#49393),.UNSPECIFIED.,.F.,.F.)
B_SPLINE_CURVE_WITH_KNOTS((3,3),(0.,0.00848409808441644),.UNSPECIFIED.)
CURVE()
GEOMETRIC_REPRESENTATION_ITEM()
RATIONAL_B_SPLINE_CURVE((1.,1.00016582971078,1.00020138403858))
REPRESENTATION_ITEM('')
);
#234=(
BOUNDED_CURVE()
B_SPLINE_CURVE(2,(#49397,#49398,#49399),.UNSPECIFIED.,.F.,.F.)
B_SPLINE_CURVE_WITH_KNOTS((3,3),(0.0131150022111809,0.0215991002954744),
 .UNSPECIFIED.)
CURVE()
GEOMETRIC_REPRESENTATION_ITEM()
RATIONAL_B_SPLINE_CURVE((1.00020138403856,1.00016582971077,1.))
REPRESENTATION_ITEM('')
);
#235=(
BOUNDED_CURVE()
B_SPLINE_CURVE(2,(#49412,#49413,#49414),.UNSPECIFIED.,.F.,.F.)
B_SPLINE_CURVE_WITH_KNOTS((3,3),(0.,0.00848409808461716),.UNSPECIFIED.)
CURVE()
GEOMETRIC_REPRESENTATION_ITEM()
RATIONAL_B_SPLINE_CURVE((1.,1.00016582970495,1.00020138403149))
REPRESENTATION_ITEM('')
);
#236=(
BOUNDED_CURVE()
B_SPLINE_CURVE(2,(#49418,#49419,#49420),.UNSPECIFIED.,.F.,.F.)
B_SPLINE_CURVE_WITH_KNOTS((3,3),(0.0131150022109262,0.0215991002954744),
 .UNSPECIFIED.)
CURVE()
GEOMETRIC_REPRESENTATION_ITEM()
RATIONAL_B_SPLINE_CURVE((1.00020138404239,1.00016582971392,1.))
REPRESENTATION_ITEM('')
);
#237=(
BOUNDED_CURVE()
B_SPLINE_CURVE(2,(#49433,#49434,#49435),.UNSPECIFIED.,.F.,.F.)
B_SPLINE_CURVE_WITH_KNOTS((3,3),(0.,0.00848409808431464),.UNSPECIFIED.)
CURVE()
GEOMETRIC_REPRESENTATION_ITEM()
RATIONAL_B_SPLINE_CURVE((1.,1.00016582970871,1.00020138403606))
REPRESENTATION_ITEM('')
);
#238=(
BOUNDED_CURVE()
B_SPLINE_CURVE(2,(#49439,#49440,#49441),.UNSPECIFIED.,.F.,.F.)
B_SPLINE_CURVE_WITH_KNOTS((3,3),(0.0131150022106601,0.0215991002954745),
 .UNSPECIFIED.)
CURVE()
GEOMETRIC_REPRESENTATION_ITEM()
RATIONAL_B_SPLINE_CURVE((1.00020138402617,1.00016582970057,1.))
REPRESENTATION_ITEM('')
);
#239=(
BOUNDED_CURVE()
B_SPLINE_CURVE(2,(#49454,#49455,#49456),.UNSPECIFIED.,.F.,.F.)
B_SPLINE_CURVE_WITH_KNOTS((3,3),(0.,0.00848409808479875),.UNSPECIFIED.)
CURVE()
GEOMETRIC_REPRESENTATION_ITEM()
RATIONAL_B_SPLINE_CURVE((1.,1.00016582970535,1.00020138403197))
REPRESENTATION_ITEM('')
);
#240=(
BOUNDED_CURVE()
B_SPLINE_CURVE(2,(#49460,#49461,#49462),.UNSPECIFIED.,.F.,.F.)
B_SPLINE_CURVE_WITH_KNOTS((3,3),(0.0131150022108306,0.0215991002954744),
 .UNSPECIFIED.)
CURVE()
GEOMETRIC_REPRESENTATION_ITEM()
RATIONAL_B_SPLINE_CURVE((1.00020138403405,1.00016582970706,1.))
REPRESENTATION_ITEM('')
);
#241=(
BOUNDED_CURVE()
B_SPLINE_CURVE(2,(#49475,#49476,#49477),.UNSPECIFIED.,.F.,.F.)
B_SPLINE_CURVE_WITH_KNOTS((3,3),(0.,0.0084840980847528),.UNSPECIFIED.)
CURVE()
GEOMETRIC_REPRESENTATION_ITEM()
RATIONAL_B_SPLINE_CURVE((1.,1.00016582970549,1.00020138403215))
REPRESENTATION_ITEM('')
);
#242=(
BOUNDED_CURVE()
B_SPLINE_CURVE(2,(#49481,#49482,#49483),.UNSPECIFIED.,.F.,.F.)
B_SPLINE_CURVE_WITH_KNOTS((3,3),(0.0131150022108369,0.0215991002954744),
 .UNSPECIFIED.)
CURVE()
GEOMETRIC_REPRESENTATION_ITEM()
RATIONAL_B_SPLINE_CURVE((1.00020138403309,1.00016582970627,1.))
REPRESENTATION_ITEM('')
);
#243=(
BOUNDED_CURVE()
B_SPLINE_CURVE(2,(#49496,#49497,#49498),.UNSPECIFIED.,.F.,.F.)
B_SPLINE_CURVE_WITH_KNOTS((3,3),(0.,0.0084840980842322),.UNSPECIFIED.)
CURVE()
GEOMETRIC_REPRESENTATION_ITEM()
RATIONAL_B_SPLINE_CURVE((1.,1.00016582971394,1.00020138404241))
REPRESENTATION_ITEM('')
);
#244=(
BOUNDED_CURVE()
B_SPLINE_CURVE(2,(#49502,#49503,#49504),.UNSPECIFIED.,.F.,.F.)
B_SPLINE_CURVE_WITH_KNOTS((3,3),(0.0131150022105481,0.0215991002954744),
 .UNSPECIFIED.)
CURVE()
GEOMETRIC_REPRESENTATION_ITEM()
RATIONAL_B_SPLINE_CURVE((1.00020138402709,1.00016582970133,1.))
REPRESENTATION_ITEM('')
);
#245=(
BOUNDED_CURVE()
B_SPLINE_CURVE(2,(#49517,#49518,#49519),.UNSPECIFIED.,.F.,.F.)
B_SPLINE_CURVE_WITH_KNOTS((3,3),(0.,0.00848409808414784),.UNSPECIFIED.)
CURVE()
GEOMETRIC_REPRESENTATION_ITEM()
RATIONAL_B_SPLINE_CURVE((1.,1.00016582970969,1.00020138403725))
REPRESENTATION_ITEM('')
);
#246=(
BOUNDED_CURVE()
B_SPLINE_CURVE(2,(#49523,#49524,#49525),.UNSPECIFIED.,.F.,.F.)
B_SPLINE_CURVE_WITH_KNOTS((3,3),(0.0131150022106295,0.0215991002954744),
 .UNSPECIFIED.)
CURVE()
GEOMETRIC_REPRESENTATION_ITEM()
RATIONAL_B_SPLINE_CURVE((1.00020138402686,1.00016582970114,1.))
REPRESENTATION_ITEM('')
);
#247=(
BOUNDED_CURVE()
B_SPLINE_CURVE(2,(#49538,#49539,#49540),.UNSPECIFIED.,.F.,.F.)
B_SPLINE_CURVE_WITH_KNOTS((3,3),(0.,0.00848409808445945),.UNSPECIFIED.)
CURVE()
GEOMETRIC_REPRESENTATION_ITEM()
RATIONAL_B_SPLINE_CURVE((1.,1.00016582971029,1.00020138403798))
REPRESENTATION_ITEM('')
);
#248=(
BOUNDED_CURVE()
B_SPLINE_CURVE(2,(#49544,#49545,#49546),.UNSPECIFIED.,.F.,.F.)
B_SPLINE_CURVE_WITH_KNOTS((3,3),(0.0131150022108553,0.0215991002954744),
 .UNSPECIFIED.)
CURVE()
GEOMETRIC_REPRESENTATION_ITEM()
RATIONAL_B_SPLINE_CURVE((1.00020138402807,1.00016582970213,1.))
REPRESENTATION_ITEM('')
);
#249=(
BOUNDED_CURVE()
B_SPLINE_CURVE(2,(#49559,#49560,#49561),.UNSPECIFIED.,.F.,.F.)
B_SPLINE_CURVE_WITH_KNOTS((3,3),(0.,0.00848409808448244),.UNSPECIFIED.)
CURVE()
GEOMETRIC_REPRESENTATION_ITEM()
RATIONAL_B_SPLINE_CURVE((1.,1.00016582970044,1.00020138402602))
REPRESENTATION_ITEM('')
);
#250=(
BOUNDED_CURVE()
B_SPLINE_CURVE(2,(#49565,#49566,#49567),.UNSPECIFIED.,.F.,.F.)
B_SPLINE_CURVE_WITH_KNOTS((3,3),(0.0131150022107,0.0215991002954745),
 .UNSPECIFIED.)
CURVE()
GEOMETRIC_REPRESENTATION_ITEM()
RATIONAL_B_SPLINE_CURVE((1.00020138402745,1.00016582970163,1.))
REPRESENTATION_ITEM('')
);
#251=(
BOUNDED_CURVE()
B_SPLINE_CURVE(2,(#49580,#49581,#49582),.UNSPECIFIED.,.F.,.F.)
B_SPLINE_CURVE_WITH_KNOTS((3,3),(0.,0.0084840980844404),.UNSPECIFIED.)
CURVE()
GEOMETRIC_REPRESENTATION_ITEM()
RATIONAL_B_SPLINE_CURVE((1.,1.00016582969984,1.00020138402529))
REPRESENTATION_ITEM('')
);
#252=(
BOUNDED_CURVE()
B_SPLINE_CURVE(2,(#49586,#49587,#49588),.UNSPECIFIED.,.F.,.F.)
B_SPLINE_CURVE_WITH_KNOTS((3,3),(0.0131150022109728,0.0215991002954744),
 .UNSPECIFIED.)
CURVE()
GEOMETRIC_REPRESENTATION_ITEM()
RATIONAL_B_SPLINE_CURVE((1.00020138403593,1.0001658297086,1.))
REPRESENTATION_ITEM('')
);
#253=(
BOUNDED_CURVE()
B_SPLINE_CURVE(2,(#49603,#49604,#49605),.UNSPECIFIED.,.F.,.F.)
B_SPLINE_CURVE_WITH_KNOTS((3,3),(0.,0.00848409808461716),.UNSPECIFIED.)
CURVE()
GEOMETRIC_REPRESENTATION_ITEM()
RATIONAL_B_SPLINE_CURVE((1.,1.00016582970494,1.00020138403149))
REPRESENTATION_ITEM('')
);
#254=(
BOUNDED_CURVE()
B_SPLINE_CURVE(2,(#49609,#49610,#49611),.UNSPECIFIED.,.F.,.F.)
B_SPLINE_CURVE_WITH_KNOTS((3,3),(0.0131150022107313,0.0215991002954744),
 .UNSPECIFIED.)
CURVE()
GEOMETRIC_REPRESENTATION_ITEM()
RATIONAL_B_SPLINE_CURVE((1.00020138404435,1.00016582971554,1.))
REPRESENTATION_ITEM('')
);
#255=(
BOUNDED_CURVE()
B_SPLINE_CURVE(2,(#49624,#49625,#49626),.UNSPECIFIED.,.F.,.F.)
B_SPLINE_CURVE_WITH_KNOTS((3,3),(0.,0.0084840980847339),.UNSPECIFIED.)
CURVE()
GEOMETRIC_REPRESENTATION_ITEM()
RATIONAL_B_SPLINE_CURVE((1.,1.00016582970597,1.00020138403273))
REPRESENTATION_ITEM('')
);
#256=(
BOUNDED_CURVE()
B_SPLINE_CURVE(2,(#49630,#49631,#49632),.UNSPECIFIED.,.F.,.F.)
B_SPLINE_CURVE_WITH_KNOTS((3,3),(0.0131150022106966,0.0215991002954744),
 .UNSPECIFIED.)
CURVE()
GEOMETRIC_REPRESENTATION_ITEM()
RATIONAL_B_SPLINE_CURVE((1.00020138403392,1.00016582970695,1.))
REPRESENTATION_ITEM('')
);
#257=(
BOUNDED_CURVE()
B_SPLINE_CURVE(2,(#49645,#49646,#49647),.UNSPECIFIED.,.F.,.F.)
B_SPLINE_CURVE_WITH_KNOTS((3,3),(0.,0.00848409808458664),.UNSPECIFIED.)
CURVE()
GEOMETRIC_REPRESENTATION_ITEM()
RATIONAL_B_SPLINE_CURVE((1.,1.00016582970477,1.00020138403127))
REPRESENTATION_ITEM('')
);
#258=(
BOUNDED_CURVE()
B_SPLINE_CURVE(2,(#49651,#49652,#49653),.UNSPECIFIED.,.F.,.F.)
B_SPLINE_CURVE_WITH_KNOTS((3,3),(0.0131150022108393,0.0215991002954745),
 .UNSPECIFIED.)
CURVE()
GEOMETRIC_REPRESENTATION_ITEM()
RATIONAL_B_SPLINE_CURVE((1.00020138403572,1.00016582970843,1.))
REPRESENTATION_ITEM('')
);
#259=(
BOUNDED_CURVE()
B_SPLINE_CURVE(2,(#49666,#49667,#49668),.UNSPECIFIED.,.F.,.F.)
B_SPLINE_CURVE_WITH_KNOTS((3,3),(0.,0.00848409808463718),.UNSPECIFIED.)
CURVE()
GEOMETRIC_REPRESENTATION_ITEM()
RATIONAL_B_SPLINE_CURVE((1.,1.00016582970055,1.00020138402615))
REPRESENTATION_ITEM('')
);
#260=(
BOUNDED_CURVE()
B_SPLINE_CURVE(2,(#49672,#49673,#49674),.UNSPECIFIED.,.F.,.F.)
B_SPLINE_CURVE_WITH_KNOTS((3,3),(0.013115002211021,0.0215991002954743),
 .UNSPECIFIED.)
CURVE()
GEOMETRIC_REPRESENTATION_ITEM()
RATIONAL_B_SPLINE_CURVE((1.00020138403351,1.00016582970661,1.))
REPRESENTATION_ITEM('')
);
#261=(
BOUNDED_CURVE()
B_SPLINE_CURVE(2,(#49687,#49688,#49689),.UNSPECIFIED.,.F.,.F.)
B_SPLINE_CURVE_WITH_KNOTS((3,3),(0.,0.0084840980842322),.UNSPECIFIED.)
CURVE()
GEOMETRIC_REPRESENTATION_ITEM()
RATIONAL_B_SPLINE_CURVE((1.,1.00016582971394,1.00020138404241))
REPRESENTATION_ITEM('')
);
#262=(
BOUNDED_CURVE()
B_SPLINE_CURVE(2,(#49693,#49694,#49695),.UNSPECIFIED.,.F.,.F.)
B_SPLINE_CURVE_WITH_KNOTS((3,3),(0.0131150022105481,0.0215991002954744),
 .UNSPECIFIED.)
CURVE()
GEOMETRIC_REPRESENTATION_ITEM()
RATIONAL_B_SPLINE_CURVE((1.00020138402709,1.00016582970133,1.))
REPRESENTATION_ITEM('')
);
#263=(
BOUNDED_CURVE()
B_SPLINE_CURVE(2,(#49708,#49709,#49710),.UNSPECIFIED.,.F.,.F.)
B_SPLINE_CURVE_WITH_KNOTS((3,3),(0.,0.00848409808456074),.UNSPECIFIED.)
CURVE()
GEOMETRIC_REPRESENTATION_ITEM()
RATIONAL_B_SPLINE_CURVE((1.,1.00016582970947,1.00020138403699))
REPRESENTATION_ITEM('')
);
#264=(
BOUNDED_CURVE()
B_SPLINE_CURVE(2,(#49714,#49715,#49716),.UNSPECIFIED.,.F.,.F.)
B_SPLINE_CURVE_WITH_KNOTS((3,3),(0.0131150022109338,0.0215991002954745),
 .UNSPECIFIED.)
CURVE()
GEOMETRIC_REPRESENTATION_ITEM()
RATIONAL_B_SPLINE_CURVE((1.00020138403466,1.00016582970756,1.))
REPRESENTATION_ITEM('')
);
#265=(
BOUNDED_CURVE()
B_SPLINE_CURVE(2,(#49729,#49730,#49731),.UNSPECIFIED.,.F.,.F.)
B_SPLINE_CURVE_WITH_KNOTS((3,3),(0.,0.00848409808446819),.UNSPECIFIED.)
CURVE()
GEOMETRIC_REPRESENTATION_ITEM()
RATIONAL_B_SPLINE_CURVE((1.,1.00016582970737,1.00020138403444))
REPRESENTATION_ITEM('')
);
#266=(
BOUNDED_CURVE()
B_SPLINE_CURVE(2,(#49735,#49736,#49737),.UNSPECIFIED.,.F.,.F.)
B_SPLINE_CURVE_WITH_KNOTS((3,3),(0.0131150022107308,0.0215991002954744),
 .UNSPECIFIED.)
CURVE()
GEOMETRIC_REPRESENTATION_ITEM()
RATIONAL_B_SPLINE_CURVE((1.00020138402973,1.0001658297035,1.))
REPRESENTATION_ITEM('')
);
#267=(
BOUNDED_CURVE()
B_SPLINE_CURVE(2,(#49750,#49751,#49752),.UNSPECIFIED.,.F.,.F.)
B_SPLINE_CURVE_WITH_KNOTS((3,3),(0.,0.00848409808448244),.UNSPECIFIED.)
CURVE()
GEOMETRIC_REPRESENTATION_ITEM()
RATIONAL_B_SPLINE_CURVE((1.,1.00016582970044,1.00020138402602))
REPRESENTATION_ITEM('')
);
#268=(
BOUNDED_CURVE()
B_SPLINE_CURVE(2,(#49756,#49757,#49758),.UNSPECIFIED.,.F.,.F.)
B_SPLINE_CURVE_WITH_KNOTS((3,3),(0.0131150022107,0.0215991002954745),
 .UNSPECIFIED.)
CURVE()
GEOMETRIC_REPRESENTATION_ITEM()
RATIONAL_B_SPLINE_CURVE((1.00020138402745,1.00016582970163,1.))
REPRESENTATION_ITEM('')
);
#269=(
BOUNDED_CURVE()
B_SPLINE_CURVE(2,(#49771,#49772,#49773),.UNSPECIFIED.,.F.,.F.)
B_SPLINE_CURVE_WITH_KNOTS((3,3),(0.,0.00848409808441086),.UNSPECIFIED.)
CURVE()
GEOMETRIC_REPRESENTATION_ITEM()
RATIONAL_B_SPLINE_CURVE((1.,1.00016582971069,1.00020138403846))
REPRESENTATION_ITEM('')
);
#270=(
BOUNDED_CURVE()
B_SPLINE_CURVE(2,(#49777,#49778,#49779),.UNSPECIFIED.,.F.,.F.)
B_SPLINE_CURVE_WITH_KNOTS((3,3),(0.0131150022109839,0.0215991002954745),
 .UNSPECIFIED.)
CURVE()
GEOMETRIC_REPRESENTATION_ITEM()
RATIONAL_B_SPLINE_CURVE((1.00020138402514,1.00016582969972,1.))
REPRESENTATION_ITEM('')
);
#271=(
BOUNDED_CURVE()
B_SPLINE_CURVE(2,(#49792,#49793,#49794),.UNSPECIFIED.,.F.,.F.)
B_SPLINE_CURVE_WITH_KNOTS((3,3),(0.,0.00848409808461089),.UNSPECIFIED.)
CURVE()
GEOMETRIC_REPRESENTATION_ITEM()
RATIONAL_B_SPLINE_CURVE((1.,1.00016582970996,1.00020138403757))
REPRESENTATION_ITEM('')
);
#272=(
BOUNDED_CURVE()
B_SPLINE_CURVE(2,(#49798,#49799,#49800),.UNSPECIFIED.,.F.,.F.)
B_SPLINE_CURVE_WITH_KNOTS((3,3),(0.0131150022107081,0.0215991002954744),
 .UNSPECIFIED.)
CURVE()
GEOMETRIC_REPRESENTATION_ITEM()
RATIONAL_B_SPLINE_CURVE((1.00020138403464,1.00016582970754,1.))
REPRESENTATION_ITEM('')
);
#273=(
BOUNDED_CURVE()
B_SPLINE_CURVE(2,(#49813,#49814,#49815),.UNSPECIFIED.,.F.,.F.)
B_SPLINE_CURVE_WITH_KNOTS((3,3),(0.,0.00848409808429742),.UNSPECIFIED.)
CURVE()
GEOMETRIC_REPRESENTATION_ITEM()
RATIONAL_B_SPLINE_CURVE((1.,1.00016582971405,1.00020138404255))
REPRESENTATION_ITEM('')
);
#274=(
BOUNDED_CURVE()
B_SPLINE_CURVE(2,(#49819,#49820,#49821),.UNSPECIFIED.,.F.,.F.)
B_SPLINE_CURVE_WITH_KNOTS((3,3),(0.0131150022109026,0.0215991002954744),
 .UNSPECIFIED.)
CURVE()
GEOMETRIC_REPRESENTATION_ITEM()
RATIONAL_B_SPLINE_CURVE((1.00020138403953,1.00016582971157,1.))
REPRESENTATION_ITEM('')
);
#275=(
BOUNDED_CURVE()
B_SPLINE_CURVE(2,(#49834,#49835,#49836),.UNSPECIFIED.,.F.,.F.)
B_SPLINE_CURVE_WITH_KNOTS((3,3),(0.,0.00848409808458664),.UNSPECIFIED.)
CURVE()
GEOMETRIC_REPRESENTATION_ITEM()
RATIONAL_B_SPLINE_CURVE((1.,1.00016582970477,1.00020138403127))
REPRESENTATION_ITEM('')
);
#276=(
BOUNDED_CURVE()
B_SPLINE_CURVE(2,(#49840,#49841,#49842),.UNSPECIFIED.,.F.,.F.)
B_SPLINE_CURVE_WITH_KNOTS((3,3),(0.0131150022108393,0.0215991002954745),
 .UNSPECIFIED.)
CURVE()
GEOMETRIC_REPRESENTATION_ITEM()
RATIONAL_B_SPLINE_CURVE((1.00020138403572,1.00016582970843,1.))
REPRESENTATION_ITEM('')
);
#277=(
BOUNDED_CURVE()
B_SPLINE_CURVE(2,(#49855,#49856,#49857),.UNSPECIFIED.,.F.,.F.)
B_SPLINE_CURVE_WITH_KNOTS((3,3),(0.,0.00848409808472772),.UNSPECIFIED.)
CURVE()
GEOMETRIC_REPRESENTATION_ITEM()
RATIONAL_B_SPLINE_CURVE((1.,1.00016582970133,1.0002013840271))
REPRESENTATION_ITEM('')
);
#278=(
BOUNDED_CURVE()
B_SPLINE_CURVE(2,(#49861,#49862,#49863),.UNSPECIFIED.,.F.,.F.)
B_SPLINE_CURVE_WITH_KNOTS((3,3),(0.0131150022106421,0.0215991002954744),
 .UNSPECIFIED.)
CURVE()
GEOMETRIC_REPRESENTATION_ITEM()
RATIONAL_B_SPLINE_CURVE((1.00020138403214,1.00016582970549,1.))
REPRESENTATION_ITEM('')
);
#279=(
BOUNDED_CURVE()
B_SPLINE_CURVE(2,(#49876,#49877,#49878),.UNSPECIFIED.,.F.,.F.)
B_SPLINE_CURVE_WITH_KNOTS((3,3),(0.,0.00848409808461495),.UNSPECIFIED.)
CURVE()
GEOMETRIC_REPRESENTATION_ITEM()
RATIONAL_B_SPLINE_CURVE((1.,1.00016582970949,1.000201384037))
REPRESENTATION_ITEM('')
);
#280=(
BOUNDED_CURVE()
B_SPLINE_CURVE(2,(#49882,#49883,#49884),.UNSPECIFIED.,.F.,.F.)
B_SPLINE_CURVE_WITH_KNOTS((3,3),(0.0131150022109445,0.0215991002954744),
 .UNSPECIFIED.)
CURVE()
GEOMETRIC_REPRESENTATION_ITEM()
RATIONAL_B_SPLINE_CURVE((1.00020138402523,1.00016582969979,1.))
REPRESENTATION_ITEM('')
);
#281=(
BOUNDED_CURVE()
B_SPLINE_CURVE(2,(#49897,#49898,#49899),.UNSPECIFIED.,.F.,.F.)
B_SPLINE_CURVE_WITH_KNOTS((3,3),(0.,0.00848409808414784),.UNSPECIFIED.)
CURVE()
GEOMETRIC_REPRESENTATION_ITEM()
RATIONAL_B_SPLINE_CURVE((1.,1.00016582970969,1.00020138403725))
REPRESENTATION_ITEM('')
);
#282=(
BOUNDED_CURVE()
B_SPLINE_CURVE(2,(#49903,#49904,#49905),.UNSPECIFIED.,.F.,.F.)
B_SPLINE_CURVE_WITH_KNOTS((3,3),(0.0131150022106295,0.0215991002954744),
 .UNSPECIFIED.)
CURVE()
GEOMETRIC_REPRESENTATION_ITEM()
RATIONAL_B_SPLINE_CURVE((1.00020138402686,1.00016582970114,1.))
REPRESENTATION_ITEM('')
);
#283=(
BOUNDED_CURVE()
B_SPLINE_CURVE(2,(#49918,#49919,#49920),.UNSPECIFIED.,.F.,.F.)
B_SPLINE_CURVE_WITH_KNOTS((3,3),(0.,0.00848409808467215),.UNSPECIFIED.)
CURVE()
GEOMETRIC_REPRESENTATION_ITEM()
RATIONAL_B_SPLINE_CURVE((1.,1.00016582970831,1.00020138403558))
REPRESENTATION_ITEM('')
);
#284=(
BOUNDED_CURVE()
B_SPLINE_CURVE(2,(#49924,#49925,#49926),.UNSPECIFIED.,.F.,.F.)
B_SPLINE_CURVE_WITH_KNOTS((3,3),(0.0131150022106657,0.0215991002954744),
 .UNSPECIFIED.)
CURVE()
GEOMETRIC_REPRESENTATION_ITEM()
RATIONAL_B_SPLINE_CURVE((1.00020138402665,1.00016582970096,1.))
REPRESENTATION_ITEM('')
);
#285=(
BOUNDED_CURVE()
B_SPLINE_CURVE(2,(#49939,#49940,#49941),.UNSPECIFIED.,.F.,.F.)
B_SPLINE_CURVE_WITH_KNOTS((3,3),(0.,0.00848409808448244),.UNSPECIFIED.)
CURVE()
GEOMETRIC_REPRESENTATION_ITEM()
RATIONAL_B_SPLINE_CURVE((1.,1.00016582970044,1.00020138402602))
REPRESENTATION_ITEM('')
);
#286=(
BOUNDED_CURVE()
B_SPLINE_CURVE(2,(#49945,#49946,#49947),.UNSPECIFIED.,.F.,.F.)
B_SPLINE_CURVE_WITH_KNOTS((3,3),(0.0131150022107,0.0215991002954745),
 .UNSPECIFIED.)
CURVE()
GEOMETRIC_REPRESENTATION_ITEM()
RATIONAL_B_SPLINE_CURVE((1.00020138402745,1.00016582970163,1.))
REPRESENTATION_ITEM('')
);
#287=(
BOUNDED_CURVE()
B_SPLINE_CURVE(2,(#49960,#49961,#49962),.UNSPECIFIED.,.F.,.F.)
B_SPLINE_CURVE_WITH_KNOTS((3,3),(0.,0.00848409808462521),.UNSPECIFIED.)
CURVE()
GEOMETRIC_REPRESENTATION_ITEM()
RATIONAL_B_SPLINE_CURVE((1.,1.00016582970203,1.00020138402795))
REPRESENTATION_ITEM('')
);
#288=(
BOUNDED_CURVE()
B_SPLINE_CURVE(2,(#49966,#49967,#49968),.UNSPECIFIED.,.F.,.F.)
B_SPLINE_CURVE_WITH_KNOTS((3,3),(0.0131150022109901,0.0215991002954744),
 .UNSPECIFIED.)
CURVE()
GEOMETRIC_REPRESENTATION_ITEM()
RATIONAL_B_SPLINE_CURVE((1.00020138403892,1.00016582971107,1.))
REPRESENTATION_ITEM('')
);
#289=(
BOUNDED_CURVE()
B_SPLINE_CURVE(2,(#50021,#50022,#50023),.UNSPECIFIED.,.F.,.F.)
B_SPLINE_CURVE_WITH_KNOTS((3,3),(0.,0.0084840980844225),.UNSPECIFIED.)
CURVE()
GEOMETRIC_REPRESENTATION_ITEM()
RATIONAL_B_SPLINE_CURVE((1.,1.00016582970633,1.00020138403317))
REPRESENTATION_ITEM('')
);
#290=(
BOUNDED_CURVE()
B_SPLINE_CURVE(2,(#50025,#50026,#50027),.UNSPECIFIED.,.F.,.F.)
B_SPLINE_CURVE_WITH_KNOTS((3,3),(0.0131150022108769,0.0215991002954744),
 .UNSPECIFIED.)
CURVE()
GEOMETRIC_REPRESENTATION_ITEM()
RATIONAL_B_SPLINE_CURVE((1.00020138402781,1.00016582970192,1.))
REPRESENTATION_ITEM('')
);
#291=(
BOUNDED_CURVE()
B_SPLINE_CURVE(2,(#52736,#52737,#52738),.UNSPECIFIED.,.F.,.F.)
B_SPLINE_CURVE_WITH_KNOTS((3,3),(0.,0.00853918025720996),.UNSPECIFIED.)
CURVE()
GEOMETRIC_REPRESENTATION_ITEM()
RATIONAL_B_SPLINE_CURVE((1.,1.00006847609056,1.000082803656))
REPRESENTATION_ITEM('')
);
#292=(
BOUNDED_CURVE()
B_SPLINE_CURVE(2,(#52742,#52743,#52744),.UNSPECIFIED.,.F.,.F.)
B_SPLINE_CURVE_WITH_KNOTS((3,3),(0.0130580720892981,0.0215972523464016),
 .UNSPECIFIED.)
CURVE()
GEOMETRIC_REPRESENTATION_ITEM()
RATIONAL_B_SPLINE_CURVE((1.0000828036589,1.00006847609296,1.))
REPRESENTATION_ITEM('')
);
#293=(
BOUNDED_CURVE()
B_SPLINE_CURVE(2,(#52757,#52758,#52759),.UNSPECIFIED.,.F.,.F.)
B_SPLINE_CURVE_WITH_KNOTS((3,3),(0.,0.00853918025691421),.UNSPECIFIED.)
CURVE()
GEOMETRIC_REPRESENTATION_ITEM()
RATIONAL_B_SPLINE_CURVE((1.,1.00006847609621,1.00008280366283))
REPRESENTATION_ITEM('')
);
#294=(
BOUNDED_CURVE()
B_SPLINE_CURVE(2,(#52763,#52764,#52765),.UNSPECIFIED.,.F.,.F.)
B_SPLINE_CURVE_WITH_KNOTS((3,3),(0.0130580720898257,0.0215972523464016),
 .UNSPECIFIED.)
CURVE()
GEOMETRIC_REPRESENTATION_ITEM()
RATIONAL_B_SPLINE_CURVE((1.00008280366765,1.00006847610019,1.))
REPRESENTATION_ITEM('')
);
#295=(
BOUNDED_CURVE()
B_SPLINE_CURVE(2,(#52778,#52779,#52780),.UNSPECIFIED.,.F.,.F.)
B_SPLINE_CURVE_WITH_KNOTS((3,3),(0.,0.00853918025697634),.UNSPECIFIED.)
CURVE()
GEOMETRIC_REPRESENTATION_ITEM()
RATIONAL_B_SPLINE_CURVE((1.,1.00006847609435,1.00008280366058))
REPRESENTATION_ITEM('')
);
#296=(
BOUNDED_CURVE()
B_SPLINE_CURVE(2,(#52784,#52785,#52786),.UNSPECIFIED.,.F.,.F.)
B_SPLINE_CURVE_WITH_KNOTS((3,3),(0.0130580720892075,0.0215972523464017),
 .UNSPECIFIED.)
CURVE()
GEOMETRIC_REPRESENTATION_ITEM()
RATIONAL_B_SPLINE_CURVE((1.00008280365926,1.00006847609326,1.))
REPRESENTATION_ITEM('')
);
#297=(
BOUNDED_CURVE()
B_SPLINE_CURVE(2,(#52799,#52800,#52801),.UNSPECIFIED.,.F.,.F.)
B_SPLINE_CURVE_WITH_KNOTS((3,3),(0.,0.00853918025740409),.UNSPECIFIED.)
CURVE()
GEOMETRIC_REPRESENTATION_ITEM()
RATIONAL_B_SPLINE_CURVE((1.,1.0000684761032,1.00008280367129))
REPRESENTATION_ITEM('')
);
#298=(
BOUNDED_CURVE()
B_SPLINE_CURVE(2,(#52805,#52806,#52807),.UNSPECIFIED.,.F.,.F.)
B_SPLINE_CURVE_WITH_KNOTS((3,3),(0.0130580720892825,0.0215972523464017),
 .UNSPECIFIED.)
CURVE()
GEOMETRIC_REPRESENTATION_ITEM()
RATIONAL_B_SPLINE_CURVE((1.00008280366617,1.00006847609897,1.))
REPRESENTATION_ITEM('')
);
#299=(
BOUNDED_CURVE()
B_SPLINE_CURVE(2,(#52820,#52821,#52822),.UNSPECIFIED.,.F.,.F.)
B_SPLINE_CURVE_WITH_KNOTS((3,3),(0.,0.00853918025766262),.UNSPECIFIED.)
CURVE()
GEOMETRIC_REPRESENTATION_ITEM()
RATIONAL_B_SPLINE_CURVE((1.,1.0000684761088,1.00008280367806))
REPRESENTATION_ITEM('')
);
#300=(
BOUNDED_CURVE()
B_SPLINE_CURVE(2,(#52826,#52827,#52828),.UNSPECIFIED.,.F.,.F.)
B_SPLINE_CURVE_WITH_KNOTS((3,3),(0.0130580720892071,0.0215972523464016),
 .UNSPECIFIED.)
CURVE()
GEOMETRIC_REPRESENTATION_ITEM()
RATIONAL_B_SPLINE_CURVE((1.00008280363157,1.00006847607036,1.))
REPRESENTATION_ITEM('')
);
#301=(
BOUNDED_CURVE()
B_SPLINE_CURVE(2,(#52841,#52842,#52843),.UNSPECIFIED.,.F.,.F.)
B_SPLINE_CURVE_WITH_KNOTS((3,3),(0.,0.00853918025670973),.UNSPECIFIED.)
CURVE()
GEOMETRIC_REPRESENTATION_ITEM()
RATIONAL_B_SPLINE_CURVE((1.,1.00006847609795,1.00008280366494))
REPRESENTATION_ITEM('')
);
#302=(
BOUNDED_CURVE()
B_SPLINE_CURVE(2,(#52847,#52848,#52849),.UNSPECIFIED.,.F.,.F.)
B_SPLINE_CURVE_WITH_KNOTS((3,3),(0.0130580720892956,0.0215972523464017),
 .UNSPECIFIED.)
CURVE()
GEOMETRIC_REPRESENTATION_ITEM()
RATIONAL_B_SPLINE_CURVE((1.00008280365344,1.00006847608844,1.))
REPRESENTATION_ITEM('')
);
#303=(
BOUNDED_CURVE()
B_SPLINE_CURVE(2,(#52862,#52863,#52864),.UNSPECIFIED.,.F.,.F.)
B_SPLINE_CURVE_WITH_KNOTS((3,3),(0.,0.00853918025748816),.UNSPECIFIED.)
CURVE()
GEOMETRIC_REPRESENTATION_ITEM()
RATIONAL_B_SPLINE_CURVE((1.,1.00006847611526,1.00008280368587))
REPRESENTATION_ITEM('')
);
#304=(
BOUNDED_CURVE()
B_SPLINE_CURVE(2,(#52868,#52869,#52870),.UNSPECIFIED.,.F.,.F.)
B_SPLINE_CURVE_WITH_KNOTS((3,3),(0.0130580720891411,0.0215972523464017),
 .UNSPECIFIED.)
CURVE()
GEOMETRIC_REPRESENTATION_ITEM()
RATIONAL_B_SPLINE_CURVE((1.00008280367274,1.00006847610441,1.))
REPRESENTATION_ITEM('')
);
#305=(
BOUNDED_CURVE()
B_SPLINE_CURVE(2,(#52883,#52884,#52885),.UNSPECIFIED.,.F.,.F.)
B_SPLINE_CURVE_WITH_KNOTS((3,3),(0.,0.00853918025712499),.UNSPECIFIED.)
CURVE()
GEOMETRIC_REPRESENTATION_ITEM()
RATIONAL_B_SPLINE_CURVE((1.,1.00006847609903,1.00008280366624))
REPRESENTATION_ITEM('')
);
#306=(
BOUNDED_CURVE()
B_SPLINE_CURVE(2,(#52889,#52890,#52891),.UNSPECIFIED.,.F.,.F.)
B_SPLINE_CURVE_WITH_KNOTS((3,3),(0.0130580720891696,0.0215972523464017),
 .UNSPECIFIED.)
CURVE()
GEOMETRIC_REPRESENTATION_ITEM()
RATIONAL_B_SPLINE_CURVE((1.00008280365716,1.00006847609152,1.))
REPRESENTATION_ITEM('')
);
#307=(
BOUNDED_CURVE()
B_SPLINE_CURVE(2,(#52904,#52905,#52906),.UNSPECIFIED.,.F.,.F.)
B_SPLINE_CURVE_WITH_KNOTS((3,3),(0.,0.00853918025650805),.UNSPECIFIED.)
CURVE()
GEOMETRIC_REPRESENTATION_ITEM()
RATIONAL_B_SPLINE_CURVE((1.,1.00006847611696,1.00008280368793))
REPRESENTATION_ITEM('')
);
#308=(
BOUNDED_CURVE()
B_SPLINE_CURVE(2,(#52910,#52911,#52912),.UNSPECIFIED.,.F.,.F.)
B_SPLINE_CURVE_WITH_KNOTS((3,3),(0.0130580720893445,0.0215972523464017),
 .UNSPECIFIED.)
CURVE()
GEOMETRIC_REPRESENTATION_ITEM()
RATIONAL_B_SPLINE_CURVE((1.00008280366859,1.00006847610097,1.))
REPRESENTATION_ITEM('')
);
#309=(
BOUNDED_CURVE()
B_SPLINE_CURVE(2,(#52925,#52926,#52927),.UNSPECIFIED.,.F.,.F.)
B_SPLINE_CURVE_WITH_KNOTS((3,3),(0.,0.00853918025671517),.UNSPECIFIED.)
CURVE()
GEOMETRIC_REPRESENTATION_ITEM()
RATIONAL_B_SPLINE_CURVE((1.,1.00006847609917,1.00008280366641))
REPRESENTATION_ITEM('')
);
#310=(
BOUNDED_CURVE()
B_SPLINE_CURVE(2,(#52931,#52932,#52933),.UNSPECIFIED.,.F.,.F.)
B_SPLINE_CURVE_WITH_KNOTS((3,3),(0.013058072089299,0.0215972523464016),
 .UNSPECIFIED.)
CURVE()
GEOMETRIC_REPRESENTATION_ITEM()
RATIONAL_B_SPLINE_CURVE((1.00008280365965,1.00006847609358,1.))
REPRESENTATION_ITEM('')
);
#311=(
BOUNDED_CURVE()
B_SPLINE_CURVE(2,(#52946,#52947,#52948),.UNSPECIFIED.,.F.,.F.)
B_SPLINE_CURVE_WITH_KNOTS((3,3),(0.,0.00853918025687022),.UNSPECIFIED.)
CURVE()
GEOMETRIC_REPRESENTATION_ITEM()
RATIONAL_B_SPLINE_CURVE((1.,1.0000684761112,1.00008280368096))
REPRESENTATION_ITEM('')
);
#312=(
BOUNDED_CURVE()
B_SPLINE_CURVE(2,(#52952,#52953,#52954),.UNSPECIFIED.,.F.,.F.)
B_SPLINE_CURVE_WITH_KNOTS((3,3),(0.0130580720898527,0.0215972523464016),
 .UNSPECIFIED.)
CURVE()
GEOMETRIC_REPRESENTATION_ITEM()
RATIONAL_B_SPLINE_CURVE((1.00008280367213,1.00006847610389,1.))
REPRESENTATION_ITEM('')
);
#313=(
BOUNDED_CURVE()
B_SPLINE_CURVE(2,(#52967,#52968,#52969),.UNSPECIFIED.,.F.,.F.)
B_SPLINE_CURVE_WITH_KNOTS((3,3),(0.,0.00853918025697634),.UNSPECIFIED.)
CURVE()
GEOMETRIC_REPRESENTATION_ITEM()
RATIONAL_B_SPLINE_CURVE((1.,1.00006847609435,1.00008280366058))
REPRESENTATION_ITEM('')
);
#314=(
BOUNDED_CURVE()
B_SPLINE_CURVE(2,(#52973,#52974,#52975),.UNSPECIFIED.,.F.,.F.)
B_SPLINE_CURVE_WITH_KNOTS((3,3),(0.0130580720892075,0.0215972523464017),
 .UNSPECIFIED.)
CURVE()
GEOMETRIC_REPRESENTATION_ITEM()
RATIONAL_B_SPLINE_CURVE((1.00008280365926,1.00006847609326,1.))
REPRESENTATION_ITEM('')
);
#315=(
BOUNDED_CURVE()
B_SPLINE_CURVE(2,(#52988,#52989,#52990),.UNSPECIFIED.,.F.,.F.)
B_SPLINE_CURVE_WITH_KNOTS((3,3),(0.,0.0085391802568594),.UNSPECIFIED.)
CURVE()
GEOMETRIC_REPRESENTATION_ITEM()
RATIONAL_B_SPLINE_CURVE((1.,1.00006847609064,1.00008280365609))
REPRESENTATION_ITEM('')
);
#316=(
BOUNDED_CURVE()
B_SPLINE_CURVE(2,(#52994,#52995,#52996),.UNSPECIFIED.,.F.,.F.)
B_SPLINE_CURVE_WITH_KNOTS((3,3),(0.0130580720892872,0.0215972523464017),
 .UNSPECIFIED.)
CURVE()
GEOMETRIC_REPRESENTATION_ITEM()
RATIONAL_B_SPLINE_CURVE((1.00008280366813,1.00006847610059,1.))
REPRESENTATION_ITEM('')
);
#317=(
BOUNDED_CURVE()
B_SPLINE_CURVE(2,(#53009,#53010,#53011),.UNSPECIFIED.,.F.,.F.)
B_SPLINE_CURVE_WITH_KNOTS((3,3),(0.,0.0085391802567755),.UNSPECIFIED.)
CURVE()
GEOMETRIC_REPRESENTATION_ITEM()
RATIONAL_B_SPLINE_CURVE((1.,1.00006847609773,1.00008280366467))
REPRESENTATION_ITEM('')
);
#318=(
BOUNDED_CURVE()
B_SPLINE_CURVE(2,(#53015,#53016,#53017),.UNSPECIFIED.,.F.,.F.)
B_SPLINE_CURVE_WITH_KNOTS((3,3),(0.0130580720893092,0.0215972523464017),
 .UNSPECIFIED.)
CURVE()
GEOMETRIC_REPRESENTATION_ITEM()
RATIONAL_B_SPLINE_CURVE((1.00008280366132,1.00006847609496,1.))
REPRESENTATION_ITEM('')
);
#319=(
BOUNDED_CURVE()
B_SPLINE_CURVE(2,(#53030,#53031,#53032),.UNSPECIFIED.,.F.,.F.)
B_SPLINE_CURVE_WITH_KNOTS((3,3),(0.,0.00853918025625497),.UNSPECIFIED.)
CURVE()
GEOMETRIC_REPRESENTATION_ITEM()
RATIONAL_B_SPLINE_CURVE((1.,1.00006847611021,1.00008280367977))
REPRESENTATION_ITEM('')
);
#320=(
BOUNDED_CURVE()
B_SPLINE_CURVE(2,(#53036,#53037,#53038),.UNSPECIFIED.,.F.,.F.)
B_SPLINE_CURVE_WITH_KNOTS((3,3),(0.0130580720899158,0.0215972523464017),
 .UNSPECIFIED.)
CURVE()
GEOMETRIC_REPRESENTATION_ITEM()
RATIONAL_B_SPLINE_CURVE((1.00008280367479,1.0000684761061,1.))
REPRESENTATION_ITEM('')
);
#321=(
BOUNDED_CURVE()
B_SPLINE_CURVE(2,(#53051,#53052,#53053),.UNSPECIFIED.,.F.,.F.)
B_SPLINE_CURVE_WITH_KNOTS((3,3),(0.,0.00853918025654146),.UNSPECIFIED.)
CURVE()
GEOMETRIC_REPRESENTATION_ITEM()
RATIONAL_B_SPLINE_CURVE((1.,1.00006847611225,1.00008280368223))
REPRESENTATION_ITEM('')
);
#322=(
BOUNDED_CURVE()
B_SPLINE_CURVE(2,(#53057,#53058,#53059),.UNSPECIFIED.,.F.,.F.)
B_SPLINE_CURVE_WITH_KNOTS((3,3),(0.0130580720890747,0.0215972523464017),
 .UNSPECIFIED.)
CURVE()
GEOMETRIC_REPRESENTATION_ITEM()
RATIONAL_B_SPLINE_CURVE((1.00008280366807,1.00006847610054,1.))
REPRESENTATION_ITEM('')
);
#323=(
BOUNDED_CURVE()
B_SPLINE_CURVE(2,(#53072,#53073,#53074),.UNSPECIFIED.,.F.,.F.)
B_SPLINE_CURVE_WITH_KNOTS((3,3),(0.,0.00853918025709599),.UNSPECIFIED.)
CURVE()
GEOMETRIC_REPRESENTATION_ITEM()
RATIONAL_B_SPLINE_CURVE((1.,1.00006847610924,1.00008280367859))
REPRESENTATION_ITEM('')
);
#324=(
BOUNDED_CURVE()
B_SPLINE_CURVE(2,(#53078,#53079,#53080),.UNSPECIFIED.,.F.,.F.)
B_SPLINE_CURVE_WITH_KNOTS((3,3),(0.0130580720900087,0.0215972523464017),
 .UNSPECIFIED.)
CURVE()
GEOMETRIC_REPRESENTATION_ITEM()
RATIONAL_B_SPLINE_CURVE((1.00008280365785,1.00006847609209,1.))
REPRESENTATION_ITEM('')
);
#325=(
BOUNDED_CURVE()
B_SPLINE_CURVE(2,(#53095,#53096,#53097),.UNSPECIFIED.,.F.,.F.)
B_SPLINE_CURVE_WITH_KNOTS((3,3),(0.,0.00853918025700788),.UNSPECIFIED.)
CURVE()
GEOMETRIC_REPRESENTATION_ITEM()
RATIONAL_B_SPLINE_CURVE((1.,1.00006847611371,1.000082803684))
REPRESENTATION_ITEM('')
);
#326=(
BOUNDED_CURVE()
B_SPLINE_CURVE(2,(#53101,#53102,#53103),.UNSPECIFIED.,.F.,.F.)
B_SPLINE_CURVE_WITH_KNOTS((3,3),(0.0130580720893571,0.0215972523464017),
 .UNSPECIFIED.)
CURVE()
GEOMETRIC_REPRESENTATION_ITEM()
RATIONAL_B_SPLINE_CURVE((1.00008280366365,1.00006847609689,1.))
REPRESENTATION_ITEM('')
);
#327=(
BOUNDED_CURVE()
B_SPLINE_CURVE(2,(#53116,#53117,#53118),.UNSPECIFIED.,.F.,.F.)
B_SPLINE_CURVE_WITH_KNOTS((3,3),(0.,0.0085391802571346),.UNSPECIFIED.)
CURVE()
GEOMETRIC_REPRESENTATION_ITEM()
RATIONAL_B_SPLINE_CURVE((1.,1.00006847610954,1.00008280367896))
REPRESENTATION_ITEM('')
);
#328=(
BOUNDED_CURVE()
B_SPLINE_CURVE(2,(#53122,#53123,#53124),.UNSPECIFIED.,.F.,.F.)
B_SPLINE_CURVE_WITH_KNOTS((3,3),(0.0130580720898028,0.0215972523464017),
 .UNSPECIFIED.)
CURVE()
GEOMETRIC_REPRESENTATION_ITEM()
RATIONAL_B_SPLINE_CURVE((1.00008280367741,1.00006847610826,1.))
REPRESENTATION_ITEM('')
);
#329=(
BOUNDED_CURVE()
B_SPLINE_CURVE(2,(#53137,#53138,#53139),.UNSPECIFIED.,.F.,.F.)
B_SPLINE_CURVE_WITH_KNOTS((3,3),(0.,0.00853918025673768),.UNSPECIFIED.)
CURVE()
GEOMETRIC_REPRESENTATION_ITEM()
RATIONAL_B_SPLINE_CURVE((1.,1.00006847610804,1.00008280367714))
REPRESENTATION_ITEM('')
);
#330=(
BOUNDED_CURVE()
B_SPLINE_CURVE(2,(#53143,#53144,#53145),.UNSPECIFIED.,.F.,.F.)
B_SPLINE_CURVE_WITH_KNOTS((3,3),(0.013058072089849,0.0215972523464017),
 .UNSPECIFIED.)
CURVE()
GEOMETRIC_REPRESENTATION_ITEM()
RATIONAL_B_SPLINE_CURVE((1.0000828036755,1.00006847610668,1.))
REPRESENTATION_ITEM('')
);
#331=(
BOUNDED_CURVE()
B_SPLINE_CURVE(2,(#53158,#53159,#53160),.UNSPECIFIED.,.F.,.F.)
B_SPLINE_CURVE_WITH_KNOTS((3,3),(0.,0.00853918025708019),.UNSPECIFIED.)
CURVE()
GEOMETRIC_REPRESENTATION_ITEM()
RATIONAL_B_SPLINE_CURVE((1.,1.00006847610096,1.00008280366858))
REPRESENTATION_ITEM('')
);
#332=(
BOUNDED_CURVE()
B_SPLINE_CURVE(2,(#53164,#53165,#53166),.UNSPECIFIED.,.F.,.F.)
B_SPLINE_CURVE_WITH_KNOTS((3,3),(0.0130580720886814,0.0215972523464017),
 .UNSPECIFIED.)
CURVE()
GEOMETRIC_REPRESENTATION_ITEM()
RATIONAL_B_SPLINE_CURVE((1.00008280364451,1.00006847608106,1.))
REPRESENTATION_ITEM('')
);
#333=(
BOUNDED_CURVE()
B_SPLINE_CURVE(2,(#53179,#53180,#53181),.UNSPECIFIED.,.F.,.F.)
B_SPLINE_CURVE_WITH_KNOTS((3,3),(0.,0.0085391802568594),.UNSPECIFIED.)
CURVE()
GEOMETRIC_REPRESENTATION_ITEM()
RATIONAL_B_SPLINE_CURVE((1.,1.00006847609064,1.00008280365609))
REPRESENTATION_ITEM('')
);
#334=(
BOUNDED_CURVE()
B_SPLINE_CURVE(2,(#53185,#53186,#53187),.UNSPECIFIED.,.F.,.F.)
B_SPLINE_CURVE_WITH_KNOTS((3,3),(0.0130580720892872,0.0215972523464017),
 .UNSPECIFIED.)
CURVE()
GEOMETRIC_REPRESENTATION_ITEM()
RATIONAL_B_SPLINE_CURVE((1.00008280366813,1.00006847610059,1.))
REPRESENTATION_ITEM('')
);
#335=(
BOUNDED_CURVE()
B_SPLINE_CURVE(2,(#53200,#53201,#53202),.UNSPECIFIED.,.F.,.F.)
B_SPLINE_CURVE_WITH_KNOTS((3,3),(0.,0.00853918025666453),.UNSPECIFIED.)
CURVE()
GEOMETRIC_REPRESENTATION_ITEM()
RATIONAL_B_SPLINE_CURVE((1.,1.0000684761013,1.00008280366899))
REPRESENTATION_ITEM('')
);
#336=(
BOUNDED_CURVE()
B_SPLINE_CURVE(2,(#53206,#53207,#53208),.UNSPECIFIED.,.F.,.F.)
B_SPLINE_CURVE_WITH_KNOTS((3,3),(0.013058072089416,0.0215972523464017),
 .UNSPECIFIED.)
CURVE()
GEOMETRIC_REPRESENTATION_ITEM()
RATIONAL_B_SPLINE_CURVE((1.00008280367373,1.00006847610522,1.))
REPRESENTATION_ITEM('')
);
#337=(
BOUNDED_CURVE()
B_SPLINE_CURVE(2,(#53221,#53222,#53223),.UNSPECIFIED.,.F.,.F.)
B_SPLINE_CURVE_WITH_KNOTS((3,3),(0.,0.00853918025670855),.UNSPECIFIED.)
CURVE()
GEOMETRIC_REPRESENTATION_ITEM()
RATIONAL_B_SPLINE_CURVE((1.,1.00006847610409,1.00008280367237))
REPRESENTATION_ITEM('')
);
#338=(
BOUNDED_CURVE()
B_SPLINE_CURVE(2,(#53227,#53228,#53229),.UNSPECIFIED.,.F.,.F.)
B_SPLINE_CURVE_WITH_KNOTS((3,3),(0.0130580720894821,0.0215972523464016),
 .UNSPECIFIED.)
CURVE()
GEOMETRIC_REPRESENTATION_ITEM()
RATIONAL_B_SPLINE_CURVE((1.00008280368423,1.00006847611391,1.))
REPRESENTATION_ITEM('')
);
#339=(
BOUNDED_CURVE()
B_SPLINE_CURVE(2,(#53242,#53243,#53244),.UNSPECIFIED.,.F.,.F.)
B_SPLINE_CURVE_WITH_KNOTS((3,3),(0.,0.00853918025654146),.UNSPECIFIED.)
CURVE()
GEOMETRIC_REPRESENTATION_ITEM()
RATIONAL_B_SPLINE_CURVE((1.,1.00006847611225,1.00008280368223))
REPRESENTATION_ITEM('')
);
#340=(
BOUNDED_CURVE()
B_SPLINE_CURVE(2,(#53248,#53249,#53250),.UNSPECIFIED.,.F.,.F.)
B_SPLINE_CURVE_WITH_KNOTS((3,3),(0.0130580720890747,0.0215972523464017),
 .UNSPECIFIED.)
CURVE()
GEOMETRIC_REPRESENTATION_ITEM()
RATIONAL_B_SPLINE_CURVE((1.00008280366807,1.00006847610054,1.))
REPRESENTATION_ITEM('')
);
#341=(
BOUNDED_CURVE()
B_SPLINE_CURVE(2,(#53263,#53264,#53265),.UNSPECIFIED.,.F.,.F.)
B_SPLINE_CURVE_WITH_KNOTS((3,3),(0.,0.00853918025706428),.UNSPECIFIED.)
CURVE()
GEOMETRIC_REPRESENTATION_ITEM()
RATIONAL_B_SPLINE_CURVE((1.,1.00006847610177,1.00008280366956))
REPRESENTATION_ITEM('')
);
#342=(
BOUNDED_CURVE()
B_SPLINE_CURVE(2,(#53269,#53270,#53271),.UNSPECIFIED.,.F.,.F.)
B_SPLINE_CURVE_WITH_KNOTS((3,3),(0.013058072089191,0.0215972523464017),
 .UNSPECIFIED.)
CURVE()
GEOMETRIC_REPRESENTATION_ITEM()
RATIONAL_B_SPLINE_CURVE((1.00008280366799,1.00006847610048,1.))
REPRESENTATION_ITEM('')
);
#343=(
BOUNDED_CURVE()
B_SPLINE_CURVE(2,(#53284,#53285,#53286),.UNSPECIFIED.,.F.,.F.)
B_SPLINE_CURVE_WITH_KNOTS((3,3),(0.,0.00853918025704869),.UNSPECIFIED.)
CURVE()
GEOMETRIC_REPRESENTATION_ITEM()
RATIONAL_B_SPLINE_CURVE((1.,1.00006847609971,1.00008280366706))
REPRESENTATION_ITEM('')
);
#344=(
BOUNDED_CURVE()
B_SPLINE_CURVE(2,(#53290,#53291,#53292),.UNSPECIFIED.,.F.,.F.)
B_SPLINE_CURVE_WITH_KNOTS((3,3),(0.0130580720893516,0.0215972523464017),
 .UNSPECIFIED.)
CURVE()
GEOMETRIC_REPRESENTATION_ITEM()
RATIONAL_B_SPLINE_CURVE((1.00008280366174,1.0000684760953,1.))
REPRESENTATION_ITEM('')
);
#345=(
BOUNDED_CURVE()
B_SPLINE_CURVE(2,(#53305,#53306,#53307),.UNSPECIFIED.,.F.,.F.)
B_SPLINE_CURVE_WITH_KNOTS((3,3),(0.,0.00853918025720127),.UNSPECIFIED.)
CURVE()
GEOMETRIC_REPRESENTATION_ITEM()
RATIONAL_B_SPLINE_CURVE((1.,1.0000684760941,1.00008280366028))
REPRESENTATION_ITEM('')
);
#346=(
BOUNDED_CURVE()
B_SPLINE_CURVE(2,(#53311,#53312,#53313),.UNSPECIFIED.,.F.,.F.)
B_SPLINE_CURVE_WITH_KNOTS((3,3),(0.0130580720897893,0.0215972523464017),
 .UNSPECIFIED.)
CURVE()
GEOMETRIC_REPRESENTATION_ITEM()
RATIONAL_B_SPLINE_CURVE((1.00008280367779,1.00006847610857,1.))
REPRESENTATION_ITEM('')
);
#347=(
BOUNDED_CURVE()
B_SPLINE_CURVE(2,(#53326,#53327,#53328),.UNSPECIFIED.,.F.,.F.)
B_SPLINE_CURVE_WITH_KNOTS((3,3),(0.,0.00853918025673768),.UNSPECIFIED.)
CURVE()
GEOMETRIC_REPRESENTATION_ITEM()
RATIONAL_B_SPLINE_CURVE((1.,1.00006847610804,1.00008280367714))
REPRESENTATION_ITEM('')
);
#348=(
BOUNDED_CURVE()
B_SPLINE_CURVE(2,(#53332,#53333,#53334),.UNSPECIFIED.,.F.,.F.)
B_SPLINE_CURVE_WITH_KNOTS((3,3),(0.013058072089849,0.0215972523464017),
 .UNSPECIFIED.)
CURVE()
GEOMETRIC_REPRESENTATION_ITEM()
RATIONAL_B_SPLINE_CURVE((1.0000828036755,1.00006847610668,1.))
REPRESENTATION_ITEM('')
);
#349=(
BOUNDED_CURVE()
B_SPLINE_CURVE(2,(#53347,#53348,#53349),.UNSPECIFIED.,.F.,.F.)
B_SPLINE_CURVE_WITH_KNOTS((3,3),(0.,0.00853918025648162),.UNSPECIFIED.)
CURVE()
GEOMETRIC_REPRESENTATION_ITEM()
RATIONAL_B_SPLINE_CURVE((1.,1.00006847611061,1.00008280368025))
REPRESENTATION_ITEM('')
);
#350=(
BOUNDED_CURVE()
B_SPLINE_CURVE(2,(#53353,#53354,#53355),.UNSPECIFIED.,.F.,.F.)
B_SPLINE_CURVE_WITH_KNOTS((3,3),(0.0130580720891761,0.0215972523464017),
 .UNSPECIFIED.)
CURVE()
GEOMETRIC_REPRESENTATION_ITEM()
RATIONAL_B_SPLINE_CURVE((1.00008280364825,1.00006847608415,1.))
REPRESENTATION_ITEM('')
);
#351=(
BOUNDED_CURVE()
B_SPLINE_CURVE(2,(#53368,#53369,#53370),.UNSPECIFIED.,.F.,.F.)
B_SPLINE_CURVE_WITH_KNOTS((3,3),(0.,0.00853918025753211),.UNSPECIFIED.)
CURVE()
GEOMETRIC_REPRESENTATION_ITEM()
RATIONAL_B_SPLINE_CURVE((1.,1.00006847610271,1.0000828036707))
REPRESENTATION_ITEM('')
);
#352=(
BOUNDED_CURVE()
B_SPLINE_CURVE(2,(#53374,#53375,#53376),.UNSPECIFIED.,.F.,.F.)
B_SPLINE_CURVE_WITH_KNOTS((3,3),(0.0130580720891711,0.0215972523464017),
 .UNSPECIFIED.)
CURVE()
GEOMETRIC_REPRESENTATION_ITEM()
RATIONAL_B_SPLINE_CURVE((1.00008280365529,1.00006847608997,1.))
REPRESENTATION_ITEM('')
);
#353=(
BOUNDED_CURVE()
B_SPLINE_CURVE(2,(#53389,#53390,#53391),.UNSPECIFIED.,.F.,.F.)
B_SPLINE_CURVE_WITH_KNOTS((3,3),(0.,0.0085391802567755),.UNSPECIFIED.)
CURVE()
GEOMETRIC_REPRESENTATION_ITEM()
RATIONAL_B_SPLINE_CURVE((1.,1.00006847609773,1.00008280366467))
REPRESENTATION_ITEM('')
);
#354=(
BOUNDED_CURVE()
B_SPLINE_CURVE(2,(#53395,#53396,#53397),.UNSPECIFIED.,.F.,.F.)
B_SPLINE_CURVE_WITH_KNOTS((3,3),(0.0130580720893092,0.0215972523464017),
 .UNSPECIFIED.)
CURVE()
GEOMETRIC_REPRESENTATION_ITEM()
RATIONAL_B_SPLINE_CURVE((1.00008280366132,1.00006847609496,1.))
REPRESENTATION_ITEM('')
);
#355=(
BOUNDED_CURVE()
B_SPLINE_CURVE(2,(#53410,#53411,#53412),.UNSPECIFIED.,.F.,.F.)
B_SPLINE_CURVE_WITH_KNOTS((3,3),(0.,0.00853918025675444),.UNSPECIFIED.)
CURVE()
GEOMETRIC_REPRESENTATION_ITEM()
RATIONAL_B_SPLINE_CURVE((1.,1.00006847610301,1.00008280367106))
REPRESENTATION_ITEM('')
);
#356=(
BOUNDED_CURVE()
B_SPLINE_CURVE(2,(#53416,#53417,#53418),.UNSPECIFIED.,.F.,.F.)
B_SPLINE_CURVE_WITH_KNOTS((3,3),(0.0130580720893406,0.0215972523464017),
 .UNSPECIFIED.)
CURVE()
GEOMETRIC_REPRESENTATION_ITEM()
RATIONAL_B_SPLINE_CURVE((1.00008280367253,1.00006847610423,1.))
REPRESENTATION_ITEM('')
);
#357=(
BOUNDED_CURVE()
B_SPLINE_CURVE(2,(#53431,#53432,#53433),.UNSPECIFIED.,.F.,.F.)
B_SPLINE_CURVE_WITH_KNOTS((3,3),(0.,0.00853918025654146),.UNSPECIFIED.)
CURVE()
GEOMETRIC_REPRESENTATION_ITEM()
RATIONAL_B_SPLINE_CURVE((1.,1.00006847611225,1.00008280368223))
REPRESENTATION_ITEM('')
);
#358=(
BOUNDED_CURVE()
B_SPLINE_CURVE(2,(#53437,#53438,#53439),.UNSPECIFIED.,.F.,.F.)
B_SPLINE_CURVE_WITH_KNOTS((3,3),(0.0130580720890747,0.0215972523464017),
 .UNSPECIFIED.)
CURVE()
GEOMETRIC_REPRESENTATION_ITEM()
RATIONAL_B_SPLINE_CURVE((1.00008280366807,1.00006847610054,1.))
REPRESENTATION_ITEM('')
);
#359=(
BOUNDED_CURVE()
B_SPLINE_CURVE(2,(#53452,#53453,#53454),.UNSPECIFIED.,.F.,.F.)
B_SPLINE_CURVE_WITH_KNOTS((3,3),(0.,0.00853918025712073),.UNSPECIFIED.)
CURVE()
GEOMETRIC_REPRESENTATION_ITEM()
RATIONAL_B_SPLINE_CURVE((1.,1.00006847609561,1.0000828036621))
REPRESENTATION_ITEM('')
);
#360=(
BOUNDED_CURVE()
B_SPLINE_CURVE(2,(#53458,#53459,#53460),.UNSPECIFIED.,.F.,.F.)
B_SPLINE_CURVE_WITH_KNOTS((3,3),(0.0130580720897129,0.0215972523464017),
 .UNSPECIFIED.)
CURVE()
GEOMETRIC_REPRESENTATION_ITEM()
RATIONAL_B_SPLINE_CURVE((1.00008280368364,1.00006847611341,1.))
REPRESENTATION_ITEM('')
);
#361=(
BOUNDED_CURVE()
B_SPLINE_CURVE(2,(#53513,#53514,#53515),.UNSPECIFIED.,.F.,.F.)
B_SPLINE_CURVE_WITH_KNOTS((3,3),(0.,0.00853918025702907),.UNSPECIFIED.)
CURVE()
GEOMETRIC_REPRESENTATION_ITEM()
RATIONAL_B_SPLINE_CURVE((1.,1.00006847610662,1.00008280367543))
REPRESENTATION_ITEM('')
);
#362=(
BOUNDED_CURVE()
B_SPLINE_CURVE(2,(#53517,#53518,#53519),.UNSPECIFIED.,.F.,.F.)
B_SPLINE_CURVE_WITH_KNOTS((3,3),(0.0130580720893726,0.0215972523464017),
 .UNSPECIFIED.)
CURVE()
GEOMETRIC_REPRESENTATION_ITEM()
RATIONAL_B_SPLINE_CURVE((1.00008280367543,1.00006847610662,1.))
REPRESENTATION_ITEM('')
);
#363=B_SPLINE_SURFACE_WITH_KNOTS('',3,3,((#34003,#34004,#34005,#34006,#34007,
#34008,#34009,#34010,#34011,#34012,#34013,#34014,#34015,#34016,#34017,#34018,
#34019,#34020,#34021,#34022,#34023,#34024,#34025,#34026,#34027,#34028,#34029,
#34030,#34031,#34032,#34033,#34034,#34035,#34036,#34037,#34038,#34039,#34040,
#34041,#34042,#34043,#34044,#34045,#34046,#34047,#34048,#34049,#34050,#34051,
#34052,#34053,#34054,#34055,#34056,#34057,#34058,#34059,#34060,#34061,#34062,
#34063,#34064,#34065,#34066,#34067,#34068,#34069,#34070,#34071,#34072,#34073,
#34074,#34075),(#34076,#34077,#34078,#34079,#34080,#34081,#34082,#34083,
#34084,#34085,#34086,#34087,#34088,#34089,#34090,#34091,#34092,#34093,#34094,
#34095,#34096,#34097,#34098,#34099,#34100,#34101,#34102,#34103,#34104,#34105,
#34106,#34107,#34108,#34109,#34110,#34111,#34112,#34113,#34114,#34115,#34116,
#34117,#34118,#34119,#34120,#34121,#34122,#34123,#34124,#34125,#34126,#34127,
#34128,#34129,#34130,#34131,#34132,#34133,#34134,#34135,#34136,#34137,#34138,
#34139,#34140,#34141,#34142,#34143,#34144,#34145,#34146,#34147,#34148),
(#34149,#34150,#34151,#34152,#34153,#34154,#34155,#34156,#34157,#34158,
#34159,#34160,#34161,#34162,#34163,#34164,#34165,#34166,#34167,#34168,#34169,
#34170,#34171,#34172,#34173,#34174,#34175,#34176,#34177,#34178,#34179,#34180,
#34181,#34182,#34183,#34184,#34185,#34186,#34187,#34188,#34189,#34190,#34191,
#34192,#34193,#34194,#34195,#34196,#34197,#34198,#34199,#34200,#34201,#34202,
#34203,#34204,#34205,#34206,#34207,#34208,#34209,#34210,#34211,#34212,#34213,
#34214,#34215,#34216,#34217,#34218,#34219,#34220,#34221),(#34222,#34223,
#34224,#34225,#34226,#34227,#34228,#34229,#34230,#34231,#34232,#34233,#34234,
#34235,#34236,#34237,#34238,#34239,#34240,#34241,#34242,#34243,#34244,#34245,
#34246,#34247,#34248,#34249,#34250,#34251,#34252,#34253,#34254,#34255,#34256,
#34257,#34258,#34259,#34260,#34261,#34262,#34263,#34264,#34265,#34266,#34267,
#34268,#34269,#34270,#34271,#34272,#34273,#34274,#34275,#34276,#34277,#34278,
#34279,#34280,#34281,#34282,#34283,#34284,#34285,#34286,#34287,#34288,#34289,
#34290,#34291,#34292,#34293,#34294)),.UNSPECIFIED.,.F.,.F.,.F.,(4,4),(4,
1,1,1,1,1,1,1,1,1,1,1,1,1,1,1,1,1,1,1,1,1,1,1,1,1,1,1,1,1,1,1,1,1,1,1,1,
1,1,1,1,1,1,1,1,1,1,1,1,1,1,1,1,1,1,1,1,1,1,1,1,1,1,1,1,1,1,1,1,1,4),(0.,
0.0496809906637673),(9.51827045652186,10.5054372529097,11.4926040492975,
12.4797708456853,13.4669376420731,14.4541044384609,15.4412712348487,16.4284380312366,
17.4156048276244,18.4027716240122,19.3899384204,20.3771052167878,21.3642720131756,
22.3514388095634,23.3386056059513,24.3257724023391,25.3129391987269,26.3001059951147,
27.2872727915025,28.2744395878903,29.2616063842781,30.2487731806659,31.2359399770538,
32.2231067734416,33.2102735698294,34.1974403662172,35.184607162605,36.1717739589928,
37.1589407553806,38.1461075517685,39.1332743481563,40.1204411445441,41.1076079409319,
42.0947747373197,43.0819415337075,44.0691083300953,45.0562751264832,46.043441922871,
47.0306087192588,48.0177755156466,49.0049423120344,49.9921091084222,50.97927590481,
51.9664427011978,52.9536094975857,53.9407762939735,54.9279430903613,55.9151098867491,
56.9022766831369,57.8894434795247,58.8766102759126,59.8637770723004,60.8509438686882,
61.838110665076,62.8252774614638,63.8124442578516,64.7996110542394,65.7867778506272,
66.7739446470151,67.7611114434029,68.7482782397907,69.7354450361785,70.7226118325663,
71.7097786289541,72.696945425342,73.6841122217298,74.6712790181176,75.6584458145054,
76.6456126108932,77.632779407281,78.6199462036688),.UNSPECIFIED.);
#364=B_SPLINE_SURFACE_WITH_KNOTS('',3,3,((#34517,#34518,#34519,#34520,#34521,
#34522,#34523,#34524,#34525,#34526,#34527,#34528,#34529,#34530,#34531,#34532,
#34533,#34534,#34535,#34536,#34537,#34538,#34539,#34540,#34541,#34542,#34543,
#34544,#34545,#34546,#34547,#34548,#34549,#34550,#34551,#34552,#34553,#34554,
#34555,#34556,#34557,#34558,#34559,#34560,#34561,#34562,#34563,#34564,#34565,
#34566,#34567,#34568,#34569,#34570,#34571,#34572,#34573,#34574,#34575,#34576,
#34577,#34578,#34579,#34580,#34581,#34582,#34583,#34584,#34585,#34586,#34587,
#34588,#34589),(#34590,#34591,#34592,#34593,#34594,#34595,#34596,#34597,
#34598,#34599,#34600,#34601,#34602,#34603,#34604,#34605,#34606,#34607,#34608,
#34609,#34610,#34611,#34612,#34613,#34614,#34615,#34616,#34617,#34618,#34619,
#34620,#34621,#34622,#34623,#34624,#34625,#34626,#34627,#34628,#34629,#34630,
#34631,#34632,#34633,#34634,#34635,#34636,#34637,#34638,#34639,#34640,#34641,
#34642,#34643,#34644,#34645,#34646,#34647,#34648,#34649,#34650,#34651,#34652,
#34653,#34654,#34655,#34656,#34657,#34658,#34659,#34660,#34661,#34662),
(#34663,#34664,#34665,#34666,#34667,#34668,#34669,#34670,#34671,#34672,
#34673,#34674,#34675,#34676,#34677,#34678,#34679,#34680,#34681,#34682,#34683,
#34684,#34685,#34686,#34687,#34688,#34689,#34690,#34691,#34692,#34693,#34694,
#34695,#34696,#34697,#34698,#34699,#34700,#34701,#34702,#34703,#34704,#34705,
#34706,#34707,#34708,#34709,#34710,#34711,#34712,#34713,#34714,#34715,#34716,
#34717,#34718,#34719,#34720,#34721,#34722,#34723,#34724,#34725,#34726,#34727,
#34728,#34729,#34730,#34731,#34732,#34733,#34734,#34735),(#34736,#34737,
#34738,#34739,#34740,#34741,#34742,#34743,#34744,#34745,#34746,#34747,#34748,
#34749,#34750,#34751,#34752,#34753,#34754,#34755,#34756,#34757,#34758,#34759,
#34760,#34761,#34762,#34763,#34764,#34765,#34766,#34767,#34768,#34769,#34770,
#34771,#34772,#34773,#34774,#34775,#34776,#34777,#34778,#34779,#34780,#34781,
#34782,#34783,#34784,#34785,#34786,#34787,#34788,#34789,#34790,#34791,#34792,
#34793,#34794,#34795,#34796,#34797,#34798,#34799,#34800,#34801,#34802,#34803,
#34804,#34805,#34806,#34807,#34808)),.UNSPECIFIED.,.F.,.F.,.F.,(4,4),(4,
1,1,1,1,1,1,1,1,1,1,1,1,1,1,1,1,1,1,1,1,1,1,1,1,1,1,1,1,1,1,1,1,1,1,1,1,
1,1,1,1,1,1,1,1,1,1,1,1,1,1,1,1,1,1,1,1,1,1,1,1,1,1,1,1,1,1,1,1,1,4),(0.,
0.0496809906637673),(12.8380991276371,13.8252659240249,14.8124327204127,
15.7995995168005,16.7867663131883,17.7739331095761,18.7610999059639,19.7482667023518,
20.7354334987396,21.7226002951274,22.7097670915152,23.696933887903,24.6841006842908,
25.6712674806786,26.6584342770665,27.6456010734543,28.6327678698421,29.6199346662299,
30.6071014626177,31.5942682590055,32.5814350553933,33.5686018517812,34.555768648169,
35.5429354445568,36.5301022409446,37.5172690373324,38.5044358337202,39.491602630108,
40.4787694264959,41.4659362228837,42.4531030192715,43.4402698156593,44.4274366120471,
45.4146034084349,46.4017702048227,47.3889370012105,48.3761037975984,49.3632705939862,
50.350437390374,51.3376041867618,52.3247709831496,53.3119377795374,54.2991045759252,
55.2862713723131,56.2734381687009,57.2606049650887,58.2477717614765,59.2349385578643,
60.2221053542521,61.2092721506399,62.1964389470278,63.1836057434156,64.1707725398034,
65.1579393361912,66.145106132579,67.1322729289668,68.1194397253546,69.1066065217424,
70.0937733181303,71.0809401145181,72.0681069109059,73.0552737072937,74.0424405036815,
75.0296073000693,76.0167740964572,77.003940892845,77.9911076892328,78.9782744856206,
79.9654412820084,80.9526080783962,81.939774874784),.UNSPECIFIED.);
#365=B_SPLINE_SURFACE_WITH_KNOTS('',3,3,((#37203,#37204,#37205,#37206,#37207,
#37208,#37209,#37210,#37211,#37212,#37213,#37214,#37215,#37216,#37217,#37218,
#37219,#37220,#37221,#37222,#37223,#37224,#37225,#37226,#37227,#37228,#37229,
#37230,#37231,#37232,#37233,#37234,#37235,#37236,#37237,#37238,#37239,#37240,
#37241,#37242,#37243,#37244,#37245,#37246,#37247,#37248,#37249,#37250,#37251,
#37252,#37253,#37254,#37255,#37256,#37257,#37258,#37259,#37260,#37261,#37262,
#37263,#37264,#37265,#37266,#37267,#37268,#37269,#37270,#37271,#37272,#37273,
#37274,#37275,#37276,#37277,#37278,#37279,#37280,#37281,#37282,#37283,#37284,
#37285,#37286,#37287,#37288,#37289,#37290,#37291,#37292,#37293,#37294,#37295,
#37296,#37297),(#37298,#37299,#37300,#37301,#37302,#37303,#37304,#37305,
#37306,#37307,#37308,#37309,#37310,#37311,#37312,#37313,#37314,#37315,#37316,
#37317,#37318,#37319,#37320,#37321,#37322,#37323,#37324,#37325,#37326,#37327,
#37328,#37329,#37330,#37331,#37332,#37333,#37334,#37335,#37336,#37337,#37338,
#37339,#37340,#37341,#37342,#37343,#37344,#37345,#37346,#37347,#37348,#37349,
#37350,#37351,#37352,#37353,#37354,#37355,#37356,#37357,#37358,#37359,#37360,
#37361,#37362,#37363,#37364,#37365,#37366,#37367,#37368,#37369,#37370,#37371,
#37372,#37373,#37374,#37375,#37376,#37377,#37378,#37379,#37380,#37381,#37382,
#37383,#37384,#37385,#37386,#37387,#37388,#37389,#37390,#37391,#37392),
(#37393,#37394,#37395,#37396,#37397,#37398,#37399,#37400,#37401,#37402,
#37403,#37404,#37405,#37406,#37407,#37408,#37409,#37410,#37411,#37412,#37413,
#37414,#37415,#37416,#37417,#37418,#37419,#37420,#37421,#37422,#37423,#37424,
#37425,#37426,#37427,#37428,#37429,#37430,#37431,#37432,#37433,#37434,#37435,
#37436,#37437,#37438,#37439,#37440,#37441,#37442,#37443,#37444,#37445,#37446,
#37447,#37448,#37449,#37450,#37451,#37452,#37453,#37454,#37455,#37456,#37457,
#37458,#37459,#37460,#37461,#37462,#37463,#37464,#37465,#37466,#37467,#37468,
#37469,#37470,#37471,#37472,#37473,#37474,#37475,#37476,#37477,#37478,#37479,
#37480,#37481,#37482,#37483,#37484,#37485,#37486,#37487),(#37488,#37489,
#37490,#37491,#37492,#37493,#37494,#37495,#37496,#37497,#37498,#37499,#37500,
#37501,#37502,#37503,#37504,#37505,#37506,#37507,#37508,#37509,#37510,#37511,
#37512,#37513,#37514,#37515,#37516,#37517,#37518,#37519,#37520,#37521,#37522,
#37523,#37524,#37525,#37526,#37527,#37528,#37529,#37530,#37531,#37532,#37533,
#37534,#37535,#37536,#37537,#37538,#37539,#37540,#37541,#37542,#37543,#37544,
#37545,#37546,#37547,#37548,#37549,#37550,#37551,#37552,#37553,#37554,#37555,
#37556,#37557,#37558,#37559,#37560,#37561,#37562,#37563,#37564,#37565,#37566,
#37567,#37568,#37569,#37570,#37571,#37572,#37573,#37574,#37575,#37576,#37577,
#37578,#37579,#37580,#37581,#37582)),.UNSPECIFIED.,.F.,.F.,.F.,(4,4),(4,
1,1,1,1,1,1,1,1,1,1,1,1,1,1,1,1,1,1,1,1,1,1,1,1,1,1,1,1,1,1,1,1,1,1,1,1,
1,1,1,1,1,1,1,1,1,1,1,1,1,1,1,1,1,1,1,1,1,1,1,1,1,1,1,1,1,1,1,1,1,1,1,1,
1,1,1,1,1,1,1,1,1,1,1,1,1,1,1,1,1,1,1,4),(0.,0.0460148164544131),(13.2114714623398,
14.2095685301207,15.2076655979016,16.2057626656825,17.2038597334634,18.2019568012443,
19.2000538690252,20.1981509368061,21.1962480045871,22.194345072368,23.1924421401489,
24.1905392079298,25.1886362757107,26.1867333434916,27.1848304112725,28.1829274790534,
29.1810245468343,30.1791216146152,31.1772186823961,32.1753157501771,33.173412817958,
34.1715098857389,35.1696069535198,36.1677040213007,37.1658010890816,38.1638981568625,
39.1619952246434,40.1600922924243,41.1581893602052,42.1562864279861,43.1543834957671,
44.152480563548,45.1505776313289,46.1486746991098,47.1467717668907,48.1448688346716,
49.1429659024525,50.1410629702334,51.1391600380143,52.1372571057952,53.1353541735761,
54.1334512413571,55.131548309138,56.1296453769189,57.1277424446998,58.1258395124807,
59.1239365802616,60.1220336480425,61.1201307158234,62.1182277836043,63.1163248513852,
64.1144219191661,65.1125189869471,66.110616054728,67.1087131225089,68.1068101902898,
69.1049072580707,70.1030043258516,71.1011013936325,72.0991984614134,73.0972955291943,
74.0953925969752,75.0934896647561,76.0915867325371,77.089683800318,78.0877808680989,
79.0858779358798,80.0839750036607,81.0820720714416,82.0801691392225,83.0782662070034,
84.0763632747843,85.0744603425652,86.0725574103461,87.0706544781271,88.068751545908,
89.0668486136889,90.0649456814698,91.0630427492507,92.0611398170316,93.0592368848125,
94.0573339525934,95.0554310203743,96.0535280881552,97.0516251559362,98.0497222237171,
99.047819291498,100.045916359279,101.04401342706,102.042110494841,103.040207562622,
104.038304630403,105.036401698183),.UNSPECIFIED.);
#366=B_SPLINE_SURFACE_WITH_KNOTS('',3,3,((#37767,#37768,#37769,#37770,#37771,
#37772,#37773,#37774,#37775,#37776,#37777,#37778,#37779,#37780,#37781,#37782,
#37783,#37784,#37785,#37786,#37787,#37788,#37789,#37790,#37791,#37792,#37793,
#37794,#37795,#37796,#37797,#37798,#37799,#37800,#37801,#37802,#37803,#37804,
#37805,#37806,#37807,#37808,#37809,#37810,#37811,#37812,#37813,#37814,#37815,
#37816,#37817,#37818,#37819,#37820,#37821,#37822,#37823,#37824,#37825,#37826,
#37827,#37828,#37829,#37830,#37831,#37832,#37833,#37834,#37835,#37836,#37837,
#37838,#37839,#37840,#37841,#37842,#37843,#37844,#37845,#37846,#37847,#37848,
#37849,#37850,#37851,#37852,#37853,#37854,#37855,#37856,#37857,#37858,#37859,
#37860,#37861),(#37862,#37863,#37864,#37865,#37866,#37867,#37868,#37869,
#37870,#37871,#37872,#37873,#37874,#37875,#37876,#37877,#37878,#37879,#37880,
#37881,#37882,#37883,#37884,#37885,#37886,#37887,#37888,#37889,#37890,#37891,
#37892,#37893,#37894,#37895,#37896,#37897,#37898,#37899,#37900,#37901,#37902,
#37903,#37904,#37905,#37906,#37907,#37908,#37909,#37910,#37911,#37912,#37913,
#37914,#37915,#37916,#37917,#37918,#37919,#37920,#37921,#37922,#37923,#37924,
#37925,#37926,#37927,#37928,#37929,#37930,#37931,#37932,#37933,#37934,#37935,
#37936,#37937,#37938,#37939,#37940,#37941,#37942,#37943,#37944,#37945,#37946,
#37947,#37948,#37949,#37950,#37951,#37952,#37953,#37954,#37955,#37956),
(#37957,#37958,#37959,#37960,#37961,#37962,#37963,#37964,#37965,#37966,
#37967,#37968,#37969,#37970,#37971,#37972,#37973,#37974,#37975,#37976,#37977,
#37978,#37979,#37980,#37981,#37982,#37983,#37984,#37985,#37986,#37987,#37988,
#37989,#37990,#37991,#37992,#37993,#37994,#37995,#37996,#37997,#37998,#37999,
#38000,#38001,#38002,#38003,#38004,#38005,#38006,#38007,#38008,#38009,#38010,
#38011,#38012,#38013,#38014,#38015,#38016,#38017,#38018,#38019,#38020,#38021,
#38022,#38023,#38024,#38025,#38026,#38027,#38028,#38029,#38030,#38031,#38032,
#38033,#38034,#38035,#38036,#38037,#38038,#38039,#38040,#38041,#38042,#38043,
#38044,#38045,#38046,#38047,#38048,#38049,#38050,#38051),(#38052,#38053,
#38054,#38055,#38056,#38057,#38058,#38059,#38060,#38061,#38062,#38063,#38064,
#38065,#38066,#38067,#38068,#38069,#38070,#38071,#38072,#38073,#38074,#38075,
#38076,#38077,#38078,#38079,#38080,#38081,#38082,#38083,#38084,#38085,#38086,
#38087,#38088,#38089,#38090,#38091,#38092,#38093,#38094,#38095,#38096,#38097,
#38098,#38099,#38100,#38101,#38102,#38103,#38104,#38105,#38106,#38107,#38108,
#38109,#38110,#38111,#38112,#38113,#38114,#38115,#38116,#38117,#38118,#38119,
#38120,#38121,#38122,#38123,#38124,#38125,#38126,#38127,#38128,#38129,#38130,
#38131,#38132,#38133,#38134,#38135,#38136,#38137,#38138,#38139,#38140,#38141,
#38142,#38143,#38144,#38145,#38146)),.UNSPECIFIED.,.F.,.F.,.F.,(4,4),(4,
1,1,1,1,1,1,1,1,1,1,1,1,1,1,1,1,1,1,1,1,1,1,1,1,1,1,1,1,1,1,1,1,1,1,1,1,
1,1,1,1,1,1,1,1,1,1,1,1,1,1,1,1,1,1,1,1,1,1,1,1,1,1,1,1,1,1,1,1,1,1,1,1,
1,1,1,1,1,1,1,1,1,1,1,1,1,1,1,1,1,1,1,4),(0.,0.0460148164544131),(16.5163060587106,
17.5144031264916,18.5125001942725,19.5105972620534,20.5086943298343,21.5067913976152,
22.5048884653961,23.502985533177,24.5010826009579,25.4991796687388,26.4972767365197,
27.4953738043006,28.4934708720816,29.4915679398625,30.4896650076434,31.4877620754243,
32.4858591432052,33.4839562109861,34.482053278767,35.4801503465479,36.4782474143288,
37.4763444821097,38.4744415498906,39.4725386176716,40.4706356854525,41.4687327532334,
42.4668298210143,43.4649268887952,44.4630239565761,45.461121024357,46.4592180921379,
47.4573151599188,48.4554122276997,49.4535092954806,50.4516063632615,51.4497034310425,
52.4478004988234,53.4458975666043,54.4439946343852,55.4420917021661,56.440188769947,
57.4382858377279,58.4363829055088,59.4344799732897,60.4325770410706,61.4306741088515,
62.4287711766325,63.4268682444134,64.4249653121943,65.4230623799752,66.4211594477561,
67.419256515537,68.4173535833179,69.4154506510988,70.4135477188797,71.4116447866606,
72.4097418544415,73.4078389222225,74.4059359900034,75.4040330577843,76.4021301255652,
77.4002271933461,78.398324261127,79.3964213289079,80.3945183966888,81.3926154644697,
82.3907125322506,83.3888096000315,84.3869066678125,85.3850037355934,86.3831008033743,
87.3811978711552,88.3792949389361,89.377392006717,90.3754890744979,91.3735861422788,
92.3716832100597,93.3697802778406,94.3678773456216,95.3659744134025,96.3640714811834,
97.3621685489643,98.3602656167452,99.3583626845261,100.356459752307,101.354556820088,
102.352653887869,103.35075095565,104.348848023431,105.346945091212,106.345042158992,
107.343139226773,108.341236294554),.UNSPECIFIED.);
#367=B_SPLINE_SURFACE_WITH_KNOTS('',3,3,((#39875,#39876,#39877,#39878,#39879,
#39880,#39881,#39882,#39883,#39884,#39885,#39886,#39887,#39888,#39889,#39890,
#39891,#39892,#39893,#39894,#39895,#39896,#39897,#39898,#39899,#39900,#39901,
#39902,#39903,#39904,#39905,#39906,#39907,#39908,#39909,#39910,#39911,#39912,
#39913,#39914,#39915,#39916,#39917,#39918,#39919,#39920,#39921,#39922,#39923,
#39924,#39925,#39926,#39927,#39928,#39929,#39930,#39931,#39932,#39933,#39934,
#39935,#39936,#39937,#39938,#39939,#39940,#39941,#39942,#39943,#39944,#39945,
#39946,#39947,#39948,#39949,#39950,#39951,#39952,#39953,#39954,#39955,#39956,
#39957,#39958,#39959,#39960,#39961,#39962,#39963,#39964,#39965,#39966,#39967,
#39968,#39969,#39970,#39971),(#39972,#39973,#39974,#39975,#39976,#39977,
#39978,#39979,#39980,#39981,#39982,#39983,#39984,#39985,#39986,#39987,#39988,
#39989,#39990,#39991,#39992,#39993,#39994,#39995,#39996,#39997,#39998,#39999,
#40000,#40001,#40002,#40003,#40004,#40005,#40006,#40007,#40008,#40009,#40010,
#40011,#40012,#40013,#40014,#40015,#40016,#40017,#40018,#40019,#40020,#40021,
#40022,#40023,#40024,#40025,#40026,#40027,#40028,#40029,#40030,#40031,#40032,
#40033,#40034,#40035,#40036,#40037,#40038,#40039,#40040,#40041,#40042,#40043,
#40044,#40045,#40046,#40047,#40048,#40049,#40050,#40051,#40052,#40053,#40054,
#40055,#40056,#40057,#40058,#40059,#40060,#40061,#40062,#40063,#40064,#40065,
#40066,#40067,#40068),(#40069,#40070,#40071,#40072,#40073,#40074,#40075,
#40076,#40077,#40078,#40079,#40080,#40081,#40082,#40083,#40084,#40085,#40086,
#40087,#40088,#40089,#40090,#40091,#40092,#40093,#40094,#40095,#40096,#40097,
#40098,#40099,#40100,#40101,#40102,#40103,#40104,#40105,#40106,#40107,#40108,
#40109,#40110,#40111,#40112,#40113,#40114,#40115,#40116,#40117,#40118,#40119,
#40120,#40121,#40122,#40123,#40124,#40125,#40126,#40127,#40128,#40129,#40130,
#40131,#40132,#40133,#40134,#40135,#40136,#40137,#40138,#40139,#40140,#40141,
#40142,#40143,#40144,#40145,#40146,#40147,#40148,#40149,#40150,#40151,#40152,
#40153,#40154,#40155,#40156,#40157,#40158,#40159,#40160,#40161,#40162,#40163,
#40164,#40165),(#40166,#40167,#40168,#40169,#40170,#40171,#40172,#40173,
#40174,#40175,#40176,#40177,#40178,#40179,#40180,#40181,#40182,#40183,#40184,
#40185,#40186,#40187,#40188,#40189,#40190,#40191,#40192,#40193,#40194,#40195,
#40196,#40197,#40198,#40199,#40200,#40201,#40202,#40203,#40204,#40205,#40206,
#40207,#40208,#40209,#40210,#40211,#40212,#40213,#40214,#40215,#40216,#40217,
#40218,#40219,#40220,#40221,#40222,#40223,#40224,#40225,#40226,#40227,#40228,
#40229,#40230,#40231,#40232,#40233,#40234,#40235,#40236,#40237,#40238,#40239,
#40240,#40241,#40242,#40243,#40244,#40245,#40246,#40247,#40248,#40249,#40250,
#40251,#40252,#40253,#40254,#40255,#40256,#40257,#40258,#40259,#40260,#40261,
#40262)),.UNSPECIFIED.,.F.,.F.,.F.,(4,4),(4,1,1,1,1,1,1,1,1,1,1,1,1,1,1,
1,1,1,1,1,1,1,1,1,1,1,1,1,1,1,1,1,1,1,1,1,1,1,1,1,1,1,1,1,1,1,1,1,1,1,1,
1,1,1,1,1,1,1,1,1,1,1,1,1,1,1,1,1,1,1,1,1,1,1,1,1,1,1,1,1,1,1,1,1,1,1,1,
1,1,1,1,1,1,1,4),(0.,0.0329955678841871),(12.071947338616,13.0618802739488,
14.0518132092816,15.0417461446143,16.0316790799471,17.0216120152799,18.0115449506126,
19.0014778859454,19.9914108212782,20.981343756611,21.9712766919437,22.9612096272765,
23.9511425626093,24.941075497942,25.9310084332748,26.9209413686076,27.9108743039403,
28.9008072392731,29.8907401746059,30.8806731099386,31.8706060452714,32.8605389806042,
33.8504719159369,34.8404048512697,35.8303377866025,36.8202707219352,37.810203657268,
38.8001365926008,39.7900695279335,40.7800024632663,41.7699353985991,42.7598683339318,
43.7498012692646,44.7397342045974,45.7296671399301,46.7196000752629,47.7095330105957,
48.6994659459284,49.6893988812612,50.679331816594,51.6692647519267,52.6591976872595,
53.6491306225923,54.639063557925,55.6289964932578,56.6189294285906,57.6088623639234,
58.5987952992561,59.5887282345889,60.5786611699216,61.5685941052544,62.5585270405872,
63.54845997592,64.5383929112527,65.5283258465855,66.5182587819182,67.508191717251,
68.4981246525838,69.4880575879166,70.4779905232493,71.4679234585821,72.4578563939149,
73.4477893292476,74.4377222645804,75.4276551999132,76.4175881352459,77.4075210705787,
78.3974540059115,79.3873869412442,80.377319876577,81.3672528119098,82.3571857472425,
83.3471186825753,84.3370516179081,85.3269845532408,86.3169174885736,87.3068504239064,
88.2967833592391,89.2867162945719,90.2766492299047,91.2665821652374,92.2565151005702,
93.246448035903,94.2363809712357,95.2263139065685,96.2162468419013,97.206179777234,
98.1961127125668,99.1860456478996,100.175978583232,101.165911518565,102.155844453898,
103.145777389231,104.135710324563,105.125643259896),.UNSPECIFIED.);
#368=B_SPLINE_SURFACE_WITH_KNOTS('',3,3,((#40400,#40401,#40402,#40403,#40404,
#40405,#40406,#40407,#40408,#40409,#40410,#40411,#40412,#40413,#40414,#40415,
#40416,#40417,#40418,#40419,#40420,#40421,#40422,#40423,#40424,#40425,#40426,
#40427,#40428,#40429,#40430,#40431,#40432,#40433,#40434,#40435,#40436,#40437,
#40438,#40439,#40440,#40441,#40442,#40443,#40444,#40445,#40446,#40447,#40448,
#40449,#40450,#40451,#40452,#40453,#40454,#40455,#40456,#40457,#40458,#40459,
#40460,#40461,#40462,#40463,#40464,#40465,#40466,#40467,#40468,#40469,#40470,
#40471,#40472,#40473,#40474,#40475,#40476,#40477,#40478,#40479,#40480,#40481,
#40482,#40483,#40484,#40485,#40486,#40487,#40488,#40489,#40490,#40491,#40492,
#40493,#40494,#40495,#40496),(#40497,#40498,#40499,#40500,#40501,#40502,
#40503,#40504,#40505,#40506,#40507,#40508,#40509,#40510,#40511,#40512,#40513,
#40514,#40515,#40516,#40517,#40518,#40519,#40520,#40521,#40522,#40523,#40524,
#40525,#40526,#40527,#40528,#40529,#40530,#40531,#40532,#40533,#40534,#40535,
#40536,#40537,#40538,#40539,#40540,#40541,#40542,#40543,#40544,#40545,#40546,
#40547,#40548,#40549,#40550,#40551,#40552,#40553,#40554,#40555,#40556,#40557,
#40558,#40559,#40560,#40561,#40562,#40563,#40564,#40565,#40566,#40567,#40568,
#40569,#40570,#40571,#40572,#40573,#40574,#40575,#40576,#40577,#40578,#40579,
#40580,#40581,#40582,#40583,#40584,#40585,#40586,#40587,#40588,#40589,#40590,
#40591,#40592,#40593),(#40594,#40595,#40596,#40597,#40598,#40599,#40600,
#40601,#40602,#40603,#40604,#40605,#40606,#40607,#40608,#40609,#40610,#40611,
#40612,#40613,#40614,#40615,#40616,#40617,#40618,#40619,#40620,#40621,#40622,
#40623,#40624,#40625,#40626,#40627,#40628,#40629,#40630,#40631,#40632,#40633,
#40634,#40635,#40636,#40637,#40638,#40639,#40640,#40641,#40642,#40643,#40644,
#40645,#40646,#40647,#40648,#40649,#40650,#40651,#40652,#40653,#40654,#40655,
#40656,#40657,#40658,#40659,#40660,#40661,#40662,#40663,#40664,#40665,#40666,
#40667,#40668,#40669,#40670,#40671,#40672,#40673,#40674,#40675,#40676,#40677,
#40678,#40679,#40680,#40681,#40682,#40683,#40684,#40685,#40686,#40687,#40688,
#40689,#40690),(#40691,#40692,#40693,#40694,#40695,#40696,#40697,#40698,
#40699,#40700,#40701,#40702,#40703,#40704,#40705,#40706,#40707,#40708,#40709,
#40710,#40711,#40712,#40713,#40714,#40715,#40716,#40717,#40718,#40719,#40720,
#40721,#40722,#40723,#40724,#40725,#40726,#40727,#40728,#40729,#40730,#40731,
#40732,#40733,#40734,#40735,#40736,#40737,#40738,#40739,#40740,#40741,#40742,
#40743,#40744,#40745,#40746,#40747,#40748,#40749,#40750,#40751,#40752,#40753,
#40754,#40755,#40756,#40757,#40758,#40759,#40760,#40761,#40762,#40763,#40764,
#40765,#40766,#40767,#40768,#40769,#40770,#40771,#40772,#40773,#40774,#40775,
#40776,#40777,#40778,#40779,#40780,#40781,#40782,#40783,#40784,#40785,#40786,
#40787)),.UNSPECIFIED.,.F.,.F.,.F.,(4,4),(4,1,1,1,1,1,1,1,1,1,1,1,1,1,1,
1,1,1,1,1,1,1,1,1,1,1,1,1,1,1,1,1,1,1,1,1,1,1,1,1,1,1,1,1,1,1,1,1,1,1,1,
1,1,1,1,1,1,1,1,1,1,1,1,1,1,1,1,1,1,1,1,1,1,1,1,1,1,1,1,1,1,1,1,1,1,1,1,
1,1,1,1,1,1,1,4),(0.,0.0329955678841871),(15.3858509318081,16.3757838671408,
17.3657168024736,18.3556497378064,19.3455826731391,20.3355156084719,21.3254485438047,
22.3153814791375,23.3053144144702,24.295247349803,25.2851802851358,26.2751132204685,
27.2650461558013,28.2549790911341,29.2449120264668,30.2348449617996,31.2247778971324,
32.2147108324651,33.2046437677979,34.1945767031307,35.1845096384634,36.1744425737962,
37.164375509129,38.1543084444617,39.1442413797945,40.1341743151273,41.12410725046,
42.1140401857928,43.1039731211256,44.0939060564583,45.0838389917911,46.0737719271239,
47.0637048624566,48.0536377977894,49.0435707331222,50.0335036684549,51.0234366037877,
52.0133695391205,53.0033024744532,53.993235409786,54.9831683451188,55.9731012804516,
56.9630342157843,57.9529671511171,58.9429000864499,59.9328330217826,60.9227659571154,
61.9126988924482,62.9026318277809,63.8925647631137,64.8824976984465,65.8724306337792,
66.862363569112,67.8522965044448,68.8422294397775,69.8321623751103,70.8220953104431,
71.8120282457758,72.8019611811086,73.7918941164414,74.7818270517741,75.7717599871069,
76.7616929224397,77.7516258577724,78.7415587931052,79.731491728438,80.7214246637707,
81.7113575991035,82.7012905344363,83.6912234697691,84.6811564051018,85.6710893404346,
86.6610222757674,87.6509552111001,88.6408881464329,89.6308210817657,90.6207540170984,
91.6106869524312,92.600619887764,93.5905528230967,94.5804857584295,95.5704186937623,
96.560351629095,97.5502845644278,98.5402174997606,99.5301504350933,100.520083370426,
101.510016305759,102.499949241092,103.489882176424,104.479815111757,105.46974804709,
106.459680982423,107.449613917755,108.439546853088),.UNSPECIFIED.);
#369=B_SPLINE_SURFACE_WITH_KNOTS('',3,3,((#46095,#46096,#46097,#46098,#46099,
#46100,#46101,#46102,#46103,#46104,#46105,#46106,#46107,#46108,#46109,#46110,
#46111,#46112,#46113,#46114,#46115,#46116,#46117,#46118,#46119,#46120,#46121,
#46122,#46123,#46124,#46125,#46126,#46127,#46128,#46129,#46130,#46131,#46132,
#46133,#46134,#46135,#46136,#46137,#46138,#46139,#46140,#46141,#46142,#46143,
#46144,#46145,#46146,#46147,#46148,#46149,#46150,#46151,#46152,#46153,#46154,
#46155,#46156,#46157,#46158,#46159,#46160,#46161,#46162,#46163,#46164,#46165,
#46166,#46167,#46168,#46169,#46170,#46171,#46172,#46173,#46174,#46175,#46176,
#46177,#46178,#46179,#46180,#46181,#46182,#46183,#46184,#46185,#46186,#46187,
#46188,#46189,#46190,#46191,#46192,#46193,#46194,#46195,#46196,#46197,#46198,
#46199,#46200,#46201,#46202,#46203,#46204,#46205,#46206,#46207,#46208,#46209,
#46210,#46211,#46212,#46213,#46214,#46215,#46216,#46217,#46218,#46219,#46220,
#46221,#46222,#46223,#46224,#46225,#46226,#46227,#46228,#46229,#46230,#46231,
#46232,#46233,#46234,#46235,#46236,#46237,#46238,#46239,#46240,#46241,#46242,
#46243,#46244,#46245,#46246,#46247,#46248,#46249,#46250,#46251,#46252,#46253,
#46254,#46255,#46256,#46257,#46258,#46259,#46260,#46261,#46262,#46263,#46264,
#46265,#46266,#46267,#46268,#46269,#46270,#46271,#46272,#46273,#46274,#46275,
#46276,#46277,#46278,#46279,#46280,#46281,#46282,#46283,#46284,#46285,#46286,
#46287,#46288,#46289,#46290,#46291,#46292,#46293,#46294,#46295,#46296,#46297,
#46298,#46299,#46300,#46301,#46302,#46303,#46304,#46305,#46306,#46307,#46308,
#46309,#46310,#46311,#46312,#46313,#46314,#46315,#46316,#46317,#46318,#46319,
#46320,#46321,#46322,#46323,#46324,#46325,#46326,#46327,#46328,#46329,#46330,
#46331,#46332,#46333,#46334,#46335,#46336,#46337,#46338,#46339,#46340,#46341,
#46342,#46343,#46344,#46345,#46346,#46347,#46348,#46349,#46350,#46351,#46352,
#46353,#46354,#46355,#46356,#46357,#46358,#46359,#46360,#46361,#46362,#46363,
#46364,#46365,#46366,#46367,#46368,#46369,#46370,#46371,#46372,#46373,#46374,
#46375,#46376,#46377,#46378,#46379,#46380,#46381,#46382,#46383,#46384,#46385,
#46386,#46387,#46388,#46389,#46390,#46391,#46392,#46393,#46394,#46395,#46396,
#46397,#46398,#46399,#46400,#46401,#46402,#46403,#46404,#46405,#46406,#46407,
#46408,#46409,#46410,#46411,#46412,#46413,#46414,#46415,#46416,#46417,#46418,
#46419,#46420,#46421,#46422,#46423,#46424,#46425,#46426,#46427,#46428,#46429,
#46430,#46431,#46432,#46433,#46434,#46435,#46436,#46437,#46438,#46439,#46440,
#46441,#46442,#46443,#46444,#46445,#46446,#46447,#46448,#46449,#46450,#46451,
#46452,#46453,#46454,#46455,#46456,#46457,#46458,#46459,#46460,#46461,#46462,
#46463,#46464,#46465,#46466,#46467),(#46468,#46469,#46470,#46471,#46472,
#46473,#46474,#46475,#46476,#46477,#46478,#46479,#46480,#46481,#46482,#46483,
#46484,#46485,#46486,#46487,#46488,#46489,#46490,#46491,#46492,#46493,#46494,
#46495,#46496,#46497,#46498,#46499,#46500,#46501,#46502,#46503,#46504,#46505,
#46506,#46507,#46508,#46509,#46510,#46511,#46512,#46513,#46514,#46515,#46516,
#46517,#46518,#46519,#46520,#46521,#46522,#46523,#46524,#46525,#46526,#46527,
#46528,#46529,#46530,#46531,#46532,#46533,#46534,#46535,#46536,#46537,#46538,
#46539,#46540,#46541,#46542,#46543,#46544,#46545,#46546,#46547,#46548,#46549,
#46550,#46551,#46552,#46553,#46554,#46555,#46556,#46557,#46558,#46559,#46560,
#46561,#46562,#46563,#46564,#46565,#46566,#46567,#46568,#46569,#46570,#46571,
#46572,#46573,#46574,#46575,#46576,#46577,#46578,#46579,#46580,#46581,#46582,
#46583,#46584,#46585,#46586,#46587,#46588,#46589,#46590,#46591,#46592,#46593,
#46594,#46595,#46596,#46597,#46598,#46599,#46600,#46601,#46602,#46603,#46604,
#46605,#46606,#46607,#46608,#46609,#46610,#46611,#46612,#46613,#46614,#46615,
#46616,#46617,#46618,#46619,#46620,#46621,#46622,#46623,#46624,#46625,#46626,
#46627,#46628,#46629,#46630,#46631,#46632,#46633,#46634,#46635,#46636,#46637,
#46638,#46639,#46640,#46641,#46642,#46643,#46644,#46645,#46646,#46647,#46648,
#46649,#46650,#46651,#46652,#46653,#46654,#46655,#46656,#46657,#46658,#46659,
#46660,#46661,#46662,#46663,#46664,#46665,#46666,#46667,#46668,#46669,#46670,
#46671,#46672,#46673,#46674,#46675,#46676,#46677,#46678,#46679,#46680,#46681,
#46682,#46683,#46684,#46685,#46686,#46687,#46688,#46689,#46690,#46691,#46692,
#46693,#46694,#46695,#46696,#46697,#46698,#46699,#46700,#46701,#46702,#46703,
#46704,#46705,#46706,#46707,#46708,#46709,#46710,#46711,#46712,#46713,#46714,
#46715,#46716,#46717,#46718,#46719,#46720,#46721,#46722,#46723,#46724,#46725,
#46726,#46727,#46728,#46729,#46730,#46731,#46732,#46733,#46734,#46735,#46736,
#46737,#46738,#46739,#46740,#46741,#46742,#46743,#46744,#46745,#46746,#46747,
#46748,#46749,#46750,#46751,#46752,#46753,#46754,#46755,#46756,#46757,#46758,
#46759,#46760,#46761,#46762,#46763,#46764,#46765,#46766,#46767,#46768,#46769,
#46770,#46771,#46772,#46773,#46774,#46775,#46776,#46777,#46778,#46779,#46780,
#46781,#46782,#46783,#46784,#46785,#46786,#46787,#46788,#46789,#46790,#46791,
#46792,#46793,#46794,#46795,#46796,#46797,#46798,#46799,#46800,#46801,#46802,
#46803,#46804,#46805,#46806,#46807,#46808,#46809,#46810,#46811,#46812,#46813,
#46814,#46815,#46816,#46817,#46818,#46819,#46820,#46821,#46822,#46823,#46824,
#46825,#46826,#46827,#46828,#46829,#46830,#46831,#46832,#46833,#46834,#46835,
#46836,#46837,#46838,#46839,#46840),(#46841,#46842,#46843,#46844,#46845,
#46846,#46847,#46848,#46849,#46850,#46851,#46852,#46853,#46854,#46855,#46856,
#46857,#46858,#46859,#46860,#46861,#46862,#46863,#46864,#46865,#46866,#46867,
#46868,#46869,#46870,#46871,#46872,#46873,#46874,#46875,#46876,#46877,#46878,
#46879,#46880,#46881,#46882,#46883,#46884,#46885,#46886,#46887,#46888,#46889,
#46890,#46891,#46892,#46893,#46894,#46895,#46896,#46897,#46898,#46899,#46900,
#46901,#46902,#46903,#46904,#46905,#46906,#46907,#46908,#46909,#46910,#46911,
#46912,#46913,#46914,#46915,#46916,#46917,#46918,#46919,#46920,#46921,#46922,
#46923,#46924,#46925,#46926,#46927,#46928,#46929,#46930,#46931,#46932,#46933,
#46934,#46935,#46936,#46937,#46938,#46939,#46940,#46941,#46942,#46943,#46944,
#46945,#46946,#46947,#46948,#46949,#46950,#46951,#46952,#46953,#46954,#46955,
#46956,#46957,#46958,#46959,#46960,#46961,#46962,#46963,#46964,#46965,#46966,
#46967,#46968,#46969,#46970,#46971,#46972,#46973,#46974,#46975,#46976,#46977,
#46978,#46979,#46980,#46981,#46982,#46983,#46984,#46985,#46986,#46987,#46988,
#46989,#46990,#46991,#46992,#46993,#46994,#46995,#46996,#46997,#46998,#46999,
#47000,#47001,#47002,#47003,#47004,#47005,#47006,#47007,#47008,#47009,#47010,
#47011,#47012,#47013,#47014,#47015,#47016,#47017,#47018,#47019,#47020,#47021,
#47022,#47023,#47024,#47025,#47026,#47027,#47028,#47029,#47030,#47031,#47032,
#47033,#47034,#47035,#47036,#47037,#47038,#47039,#47040,#47041,#47042,#47043,
#47044,#47045,#47046,#47047,#47048,#47049,#47050,#47051,#47052,#47053,#47054,
#47055,#47056,#47057,#47058,#47059,#47060,#47061,#47062,#47063,#47064,#47065,
#47066,#47067,#47068,#47069,#47070,#47071,#47072,#47073,#47074,#47075,#47076,
#47077,#47078,#47079,#47080,#47081,#47082,#47083,#47084,#47085,#47086,#47087,
#47088,#47089,#47090,#47091,#47092,#47093,#47094,#47095,#47096,#47097,#47098,
#47099,#47100,#47101,#47102,#47103,#47104,#47105,#47106,#47107,#47108,#47109,
#47110,#47111,#47112,#47113,#47114,#47115,#47116,#47117,#47118,#47119,#47120,
#47121,#47122,#47123,#47124,#47125,#47126,#47127,#47128,#47129,#47130,#47131,
#47132,#47133,#47134,#47135,#47136,#47137,#47138,#47139,#47140,#47141,#47142,
#47143,#47144,#47145,#47146,#47147,#47148,#47149,#47150,#47151,#47152,#47153,
#47154,#47155,#47156,#47157,#47158,#47159,#47160,#47161,#47162,#47163,#47164,
#47165,#47166,#47167,#47168,#47169,#47170,#47171,#47172,#47173,#47174,#47175,
#47176,#47177,#47178,#47179,#47180,#47181,#47182,#47183,#47184,#47185,#47186,
#47187,#47188,#47189,#47190,#47191,#47192,#47193,#47194,#47195,#47196,#47197,
#47198,#47199,#47200,#47201,#47202,#47203,#47204,#47205,#47206,#47207,#47208,
#47209,#47210,#47211,#47212,#47213),(#47214,#47215,#47216,#47217,#47218,
#47219,#47220,#47221,#47222,#47223,#47224,#47225,#47226,#47227,#47228,#47229,
#47230,#47231,#47232,#47233,#47234,#47235,#47236,#47237,#47238,#47239,#47240,
#47241,#47242,#47243,#47244,#47245,#47246,#47247,#47248,#47249,#47250,#47251,
#47252,#47253,#47254,#47255,#47256,#47257,#47258,#47259,#47260,#47261,#47262,
#47263,#47264,#47265,#47266,#47267,#47268,#47269,#47270,#47271,#47272,#47273,
#47274,#47275,#47276,#47277,#47278,#47279,#47280,#47281,#47282,#47283,#47284,
#47285,#47286,#47287,#47288,#47289,#47290,#47291,#47292,#47293,#47294,#47295,
#47296,#47297,#47298,#47299,#47300,#47301,#47302,#47303,#47304,#47305,#47306,
#47307,#47308,#47309,#47310,#47311,#47312,#47313,#47314,#47315,#47316,#47317,
#47318,#47319,#47320,#47321,#47322,#47323,#47324,#47325,#47326,#47327,#47328,
#47329,#47330,#47331,#47332,#47333,#47334,#47335,#47336,#47337,#47338,#47339,
#47340,#47341,#47342,#47343,#47344,#47345,#47346,#47347,#47348,#47349,#47350,
#47351,#47352,#47353,#47354,#47355,#47356,#47357,#47358,#47359,#47360,#47361,
#47362,#47363,#47364,#47365,#47366,#47367,#47368,#47369,#47370,#47371,#47372,
#47373,#47374,#47375,#47376,#47377,#47378,#47379,#47380,#47381,#47382,#47383,
#47384,#47385,#47386,#47387,#47388,#47389,#47390,#47391,#47392,#47393,#47394,
#47395,#47396,#47397,#47398,#47399,#47400,#47401,#47402,#47403,#47404,#47405,
#47406,#47407,#47408,#47409,#47410,#47411,#47412,#47413,#47414,#47415,#47416,
#47417,#47418,#47419,#47420,#47421,#47422,#47423,#47424,#47425,#47426,#47427,
#47428,#47429,#47430,#47431,#47432,#47433,#47434,#47435,#47436,#47437,#47438,
#47439,#47440,#47441,#47442,#47443,#47444,#47445,#47446,#47447,#47448,#47449,
#47450,#47451,#47452,#47453,#47454,#47455,#47456,#47457,#47458,#47459,#47460,
#47461,#47462,#47463,#47464,#47465,#47466,#47467,#47468,#47469,#47470,#47471,
#47472,#47473,#47474,#47475,#47476,#47477,#47478,#47479,#47480,#47481,#47482,
#47483,#47484,#47485,#47486,#47487,#47488,#47489,#47490,#47491,#47492,#47493,
#47494,#47495,#47496,#47497,#47498,#47499,#47500,#47501,#47502,#47503,#47504,
#47505,#47506,#47507,#47508,#47509,#47510,#47511,#47512,#47513,#47514,#47515,
#47516,#47517,#47518,#47519,#47520,#47521,#47522,#47523,#47524,#47525,#47526,
#47527,#47528,#47529,#47530,#47531,#47532,#47533,#47534,#47535,#47536,#47537,
#47538,#47539,#47540,#47541,#47542,#47543,#47544,#47545,#47546,#47547,#47548,
#47549,#47550,#47551,#47552,#47553,#47554,#47555,#47556,#47557,#47558,#47559,
#47560,#47561,#47562,#47563,#47564,#47565,#47566,#47567,#47568,#47569,#47570,
#47571,#47572,#47573,#47574,#47575,#47576,#47577,#47578,#47579,#47580,#47581,
#47582,#47583,#47584,#47585,#47586)),.UNSPECIFIED.,.F.,.F.,.F.,(4,4),(4,
1,1,1,1,1,1,1,1,1,1,1,1,1,1,1,1,1,1,1,1,1,1,1,1,1,1,1,1,1,1,1,1,1,1,1,1,
1,1,1,1,1,1,1,1,1,1,1,1,1,1,1,1,1,1,1,1,1,1,1,1,1,1,1,1,1,1,1,1,1,1,1,1,
1,1,1,1,1,1,1,1,1,1,1,1,1,1,1,1,1,1,1,1,1,1,1,1,1,1,1,1,1,1,1,1,1,1,1,1,
1,1,1,1,1,1,1,1,1,1,1,1,1,1,1,1,1,1,1,1,1,1,1,1,1,1,1,1,1,1,1,1,1,1,1,1,
1,1,1,1,1,1,1,1,1,1,1,1,1,1,1,1,1,1,1,1,1,1,1,1,1,1,1,1,1,1,1,1,1,1,1,1,
1,1,1,1,1,1,1,1,1,1,1,1,1,1,1,1,1,1,1,1,1,1,1,1,1,1,1,1,1,1,1,1,1,1,1,1,
1,1,1,1,1,1,1,1,1,1,1,1,1,1,1,1,1,1,1,1,1,1,1,1,1,1,1,1,1,1,1,1,1,1,1,1,
1,1,1,1,1,1,1,1,1,1,1,1,1,1,1,1,1,1,1,1,1,1,1,1,1,1,1,1,1,1,1,1,1,1,1,1,
1,1,1,1,1,1,1,1,1,1,1,1,1,1,1,1,1,1,1,1,1,1,1,1,1,1,1,1,1,1,1,1,1,1,1,1,
1,1,1,1,1,1,1,1,1,1,1,1,1,1,1,1,1,1,1,1,1,1,1,1,1,1,1,1,1,1,1,1,1,1,1,1,
1,1,1,1,1,1,1,1,1,4),(0.,0.0329955678841869),(12.0719473386168,13.0706334181767,
14.0693194977367,15.0680055772966,16.0666916568566,17.0653777364165,18.0640638159765,
19.0627498955364,20.0614359750964,21.0601220546563,22.0588081342163,23.0574942137762,
24.0561802933362,25.0548663728961,26.0535524524561,27.052238532016,28.050924611576,
29.0496106911359,30.0482967706959,31.0469828502558,32.0456689298158,33.0443550093757,
34.0430410889357,35.0417271684956,36.0404132480556,37.0390993276155,38.0377854071755,
39.0364714867355,40.0351575662954,41.0338436458553,42.0325297254153,43.0312158049753,
44.0299018845352,45.0285879640952,46.0272740436551,47.0259601232151,48.024646202775,
49.023332282335,50.0220183618949,51.0207044414549,52.0193905210148,53.0180766005748,
54.0167626801347,55.0154487596947,56.0141348392546,57.0128209188146,58.0115069983745,
59.0101930779345,60.0088791574944,61.0075652370544,62.0062513166143,63.0049373961743,
64.0036234757342,65.0023095552942,66.0009956348541,66.9996817144141,67.998367793974,
68.997053873534,69.9957399530939,70.9944260326539,71.9931121122139,72.9917981917738,
73.9904842713337,74.9891703508937,75.9878564304536,76.9865425100136,77.9852285895736,
78.9839146691335,79.9826007486935,80.9812868282534,81.9799729078134,82.9786589873733,
83.9773450669333,84.9760311464932,85.9747172260532,86.9734033056131,87.9720893851731,
88.970775464733,89.969461544293,90.9681476238529,91.9668337034129,92.9655197829728,
93.9642058625328,94.9628919420927,95.9615780216527,96.9602641012126,97.9589501807726,
98.9576362603325,99.9563223398925,100.955008419452,101.953694499012,102.952380578572,
103.951066658132,104.949752737692,105.948438817252,106.947124896812,107.945810976372,
108.944497055932,109.943183135492,110.941869215052,111.940555294612,112.939241374172,
113.937927453732,114.936613533292,115.935299612852,116.933985692412,117.932671771972,
118.931357851532,119.930043931092,120.928730010651,121.927416090211,122.926102169771,
123.924788249331,124.923474328891,125.922160408451,126.920846488011,127.919532567571,
128.918218647131,129.916904726691,130.915590806251,131.914276885811,132.912962965371,
133.911649044931,134.910335124491,135.909021204051,136.907707283611,137.906393363171,
138.905079442731,139.903765522291,140.90245160185,141.90113768141,142.89982376097,
143.89850984053,144.89719592009,145.89588199965,146.89456807921,147.89325415877,
148.89194023833,149.89062631789,150.88931239745,151.88799847701,152.88668455657,
153.88537063613,154.88405671569,155.88274279525,156.88142887481,157.88011495437,
158.87880103393,159.87748711349,160.87617319305,161.874859272609,162.873545352169,
163.872231431729,164.870917511289,165.869603590849,166.868289670409,167.866975749969,
168.865661829529,169.864347909089,170.863033988649,171.861720068209,172.860406147769,
173.859092227329,174.857778306889,175.856464386449,176.855150466009,177.853836545569,
178.852522625129,179.851208704689,180.849894784249,181.848580863809,182.847266943368,
183.845953022928,184.844639102488,185.843325182048,186.842011261608,187.840697341168,
188.839383420728,189.838069500288,190.836755579848,191.835441659408,192.834127738968,
193.832813818528,194.831499898088,195.830185977648,196.828872057208,197.827558136768,
198.826244216328,199.824930295888,200.823616375448,201.822302455008,202.820988534567,
203.819674614127,204.818360693687,205.817046773247,206.815732852807,207.814418932367,
208.813105011927,209.811791091487,210.810477171047,211.809163250607,212.807849330167,
213.806535409727,214.805221489287,215.803907568847,216.802593648407,217.801279727967,
218.799965807527,219.798651887087,220.797337966647,221.796024046207,222.794710125767,
223.793396205326,224.792082284886,225.790768364446,226.789454444006,227.788140523566,
228.786826603126,229.785512682686,230.784198762246,231.782884841806,232.781570921366,
233.780257000926,234.778943080486,235.777629160046,236.776315239606,237.775001319166,
238.773687398726,239.772373478286,240.771059557846,241.769745637406,242.768431716966,
243.767117796525,244.765803876085,245.764489955645,246.763176035205,247.761862114765,
248.760548194325,249.759234273885,250.757920353445,251.756606433005,252.755292512565,
253.753978592125,254.752664671685,255.751350751245,256.750036830805,257.748722910365,
258.747408989925,259.746095069485,260.744781149045,261.743467228605,262.742153308165,
263.740839387725,264.739525467284,265.738211546844,266.736897626404,267.735583705964,
268.734269785524,269.732955865084,270.731641944644,271.730328024204,272.729014103764,
273.727700183324,274.726386262884,275.725072342444,276.723758422004,277.722444501564,
278.721130581124,279.719816660684,280.718502740244,281.717188819804,282.715874899364,
283.714560978924,284.713247058484,285.711933138043,286.710619217603,287.709305297163,
288.707991376723,289.706677456283,290.705363535843,291.704049615403,292.702735694963,
293.701421774523,294.700107854083,295.698793933643,296.697480013203,297.696166092763,
298.694852172323,299.693538251883,300.692224331443,301.690910411003,302.689596490563,
303.688282570123,304.686968649683,305.685654729243,306.684340808802,307.683026888362,
308.681712967922,309.680399047482,310.679085127042,311.677771206602,312.676457286162,
313.675143365722,314.673829445282,315.672515524842,316.671201604402,317.669887683962,
318.668573763522,319.667259843082,320.665945922642,321.664632002202,322.663318081762,
323.662004161322,324.660690240882,325.659376320442,326.658062400001,327.656748479561,
328.655434559121,329.654120638681,330.652806718241,331.651492797801,332.650178877361,
333.648864956921,334.647551036481,335.646237116041,336.644923195601,337.643609275161,
338.642295354721,339.640981434281,340.639667513841,341.638353593401,342.637039672961,
343.635725752521,344.634411832081,345.633097911641,346.631783991201,347.63047007076,
348.62915615032,349.62784222988,350.62652830944,351.625214389,352.62390046856,
353.62258654812,354.62127262768,355.61995870724,356.6186447868,357.61733086636,
358.61601694592,359.61470302548,360.61338910504,361.6120751846,362.61076126416,
363.60944734372,364.60813342328,365.60681950284,366.6055055824,367.60419166196,
368.602877741519,369.601563821079,370.600249900639,371.598935980199,372.597622059759,
373.596308139319,374.594994218879,375.593680298439,376.592366377999,377.591052457559,
378.589738537119,379.588424616679,380.587110696239,381.585796775799),
 .UNSPECIFIED.);
#370=B_SPLINE_SURFACE_WITH_KNOTS('',3,3,((#47724,#47725,#47726,#47727,#47728,
#47729,#47730,#47731,#47732,#47733,#47734,#47735,#47736,#47737,#47738,#47739,
#47740,#47741,#47742,#47743,#47744,#47745,#47746,#47747,#47748,#47749,#47750,
#47751,#47752,#47753,#47754,#47755,#47756,#47757,#47758,#47759,#47760,#47761,
#47762,#47763,#47764,#47765,#47766,#47767,#47768,#47769,#47770,#47771,#47772,
#47773,#47774,#47775,#47776,#47777,#47778,#47779,#47780,#47781,#47782,#47783,
#47784,#47785,#47786,#47787,#47788,#47789,#47790,#47791,#47792,#47793,#47794,
#47795,#47796,#47797,#47798,#47799,#47800,#47801,#47802,#47803,#47804,#47805,
#47806,#47807,#47808,#47809,#47810,#47811,#47812,#47813,#47814,#47815,#47816,
#47817,#47818,#47819,#47820,#47821,#47822,#47823,#47824,#47825,#47826,#47827,
#47828,#47829,#47830,#47831,#47832,#47833,#47834,#47835,#47836,#47837,#47838,
#47839,#47840,#47841,#47842,#47843,#47844,#47845,#47846,#47847,#47848,#47849,
#47850,#47851,#47852,#47853,#47854,#47855,#47856,#47857,#47858,#47859,#47860,
#47861,#47862,#47863,#47864,#47865,#47866,#47867,#47868,#47869,#47870,#47871,
#47872,#47873,#47874,#47875,#47876,#47877,#47878,#47879,#47880,#47881,#47882,
#47883,#47884,#47885,#47886,#47887,#47888,#47889,#47890,#47891,#47892,#47893,
#47894,#47895,#47896,#47897,#47898,#47899,#47900,#47901,#47902,#47903,#47904,
#47905,#47906,#47907,#47908,#47909,#47910,#47911,#47912,#47913,#47914,#47915,
#47916,#47917,#47918,#47919,#47920,#47921,#47922,#47923,#47924,#47925,#47926,
#47927,#47928,#47929,#47930,#47931,#47932,#47933,#47934,#47935,#47936,#47937,
#47938,#47939,#47940,#47941,#47942,#47943,#47944,#47945,#47946,#47947,#47948,
#47949,#47950,#47951,#47952,#47953,#47954,#47955,#47956,#47957,#47958,#47959,
#47960,#47961,#47962,#47963,#47964,#47965,#47966,#47967,#47968,#47969,#47970,
#47971,#47972,#47973,#47974,#47975,#47976,#47977,#47978,#47979,#47980,#47981,
#47982,#47983,#47984,#47985,#47986,#47987,#47988,#47989,#47990,#47991,#47992,
#47993,#47994,#47995,#47996,#47997,#47998,#47999,#48000,#48001,#48002,#48003,
#48004,#48005,#48006,#48007,#48008,#48009,#48010,#48011,#48012,#48013,#48014,
#48015,#48016,#48017,#48018,#48019,#48020,#48021,#48022,#48023,#48024,#48025,
#48026,#48027,#48028,#48029,#48030,#48031,#48032,#48033,#48034,#48035,#48036,
#48037,#48038,#48039,#48040,#48041,#48042,#48043,#48044,#48045,#48046,#48047,
#48048,#48049,#48050,#48051,#48052,#48053,#48054,#48055,#48056,#48057,#48058,
#48059,#48060,#48061,#48062,#48063,#48064,#48065,#48066,#48067,#48068,#48069,
#48070,#48071,#48072,#48073,#48074,#48075,#48076,#48077,#48078,#48079,#48080,
#48081,#48082,#48083,#48084,#48085,#48086,#48087,#48088,#48089,#48090,#48091,
#48092,#48093,#48094,#48095,#48096),(#48097,#48098,#48099,#48100,#48101,
#48102,#48103,#48104,#48105,#48106,#48107,#48108,#48109,#48110,#48111,#48112,
#48113,#48114,#48115,#48116,#48117,#48118,#48119,#48120,#48121,#48122,#48123,
#48124,#48125,#48126,#48127,#48128,#48129,#48130,#48131,#48132,#48133,#48134,
#48135,#48136,#48137,#48138,#48139,#48140,#48141,#48142,#48143,#48144,#48145,
#48146,#48147,#48148,#48149,#48150,#48151,#48152,#48153,#48154,#48155,#48156,
#48157,#48158,#48159,#48160,#48161,#48162,#48163,#48164,#48165,#48166,#48167,
#48168,#48169,#48170,#48171,#48172,#48173,#48174,#48175,#48176,#48177,#48178,
#48179,#48180,#48181,#48182,#48183,#48184,#48185,#48186,#48187,#48188,#48189,
#48190,#48191,#48192,#48193,#48194,#48195,#48196,#48197,#48198,#48199,#48200,
#48201,#48202,#48203,#48204,#48205,#48206,#48207,#48208,#48209,#48210,#48211,
#48212,#48213,#48214,#48215,#48216,#48217,#48218,#48219,#48220,#48221,#48222,
#48223,#48224,#48225,#48226,#48227,#48228,#48229,#48230,#48231,#48232,#48233,
#48234,#48235,#48236,#48237,#48238,#48239,#48240,#48241,#48242,#48243,#48244,
#48245,#48246,#48247,#48248,#48249,#48250,#48251,#48252,#48253,#48254,#48255,
#48256,#48257,#48258,#48259,#48260,#48261,#48262,#48263,#48264,#48265,#48266,
#48267,#48268,#48269,#48270,#48271,#48272,#48273,#48274,#48275,#48276,#48277,
#48278,#48279,#48280,#48281,#48282,#48283,#48284,#48285,#48286,#48287,#48288,
#48289,#48290,#48291,#48292,#48293,#48294,#48295,#48296,#48297,#48298,#48299,
#48300,#48301,#48302,#48303,#48304,#48305,#48306,#48307,#48308,#48309,#48310,
#48311,#48312,#48313,#48314,#48315,#48316,#48317,#48318,#48319,#48320,#48321,
#48322,#48323,#48324,#48325,#48326,#48327,#48328,#48329,#48330,#48331,#48332,
#48333,#48334,#48335,#48336,#48337,#48338,#48339,#48340,#48341,#48342,#48343,
#48344,#48345,#48346,#48347,#48348,#48349,#48350,#48351,#48352,#48353,#48354,
#48355,#48356,#48357,#48358,#48359,#48360,#48361,#48362,#48363,#48364,#48365,
#48366,#48367,#48368,#48369,#48370,#48371,#48372,#48373,#48374,#48375,#48376,
#48377,#48378,#48379,#48380,#48381,#48382,#48383,#48384,#48385,#48386,#48387,
#48388,#48389,#48390,#48391,#48392,#48393,#48394,#48395,#48396,#48397,#48398,
#48399,#48400,#48401,#48402,#48403,#48404,#48405,#48406,#48407,#48408,#48409,
#48410,#48411,#48412,#48413,#48414,#48415,#48416,#48417,#48418,#48419,#48420,
#48421,#48422,#48423,#48424,#48425,#48426,#48427,#48428,#48429,#48430,#48431,
#48432,#48433,#48434,#48435,#48436,#48437,#48438,#48439,#48440,#48441,#48442,
#48443,#48444,#48445,#48446,#48447,#48448,#48449,#48450,#48451,#48452,#48453,
#48454,#48455,#48456,#48457,#48458,#48459,#48460,#48461,#48462,#48463,#48464,
#48465,#48466,#48467,#48468,#48469),(#48470,#48471,#48472,#48473,#48474,
#48475,#48476,#48477,#48478,#48479,#48480,#48481,#48482,#48483,#48484,#48485,
#48486,#48487,#48488,#48489,#48490,#48491,#48492,#48493,#48494,#48495,#48496,
#48497,#48498,#48499,#48500,#48501,#48502,#48503,#48504,#48505,#48506,#48507,
#48508,#48509,#48510,#48511,#48512,#48513,#48514,#48515,#48516,#48517,#48518,
#48519,#48520,#48521,#48522,#48523,#48524,#48525,#48526,#48527,#48528,#48529,
#48530,#48531,#48532,#48533,#48534,#48535,#48536,#48537,#48538,#48539,#48540,
#48541,#48542,#48543,#48544,#48545,#48546,#48547,#48548,#48549,#48550,#48551,
#48552,#48553,#48554,#48555,#48556,#48557,#48558,#48559,#48560,#48561,#48562,
#48563,#48564,#48565,#48566,#48567,#48568,#48569,#48570,#48571,#48572,#48573,
#48574,#48575,#48576,#48577,#48578,#48579,#48580,#48581,#48582,#48583,#48584,
#48585,#48586,#48587,#48588,#48589,#48590,#48591,#48592,#48593,#48594,#48595,
#48596,#48597,#48598,#48599,#48600,#48601,#48602,#48603,#48604,#48605,#48606,
#48607,#48608,#48609,#48610,#48611,#48612,#48613,#48614,#48615,#48616,#48617,
#48618,#48619,#48620,#48621,#48622,#48623,#48624,#48625,#48626,#48627,#48628,
#48629,#48630,#48631,#48632,#48633,#48634,#48635,#48636,#48637,#48638,#48639,
#48640,#48641,#48642,#48643,#48644,#48645,#48646,#48647,#48648,#48649,#48650,
#48651,#48652,#48653,#48654,#48655,#48656,#48657,#48658,#48659,#48660,#48661,
#48662,#48663,#48664,#48665,#48666,#48667,#48668,#48669,#48670,#48671,#48672,
#48673,#48674,#48675,#48676,#48677,#48678,#48679,#48680,#48681,#48682,#48683,
#48684,#48685,#48686,#48687,#48688,#48689,#48690,#48691,#48692,#48693,#48694,
#48695,#48696,#48697,#48698,#48699,#48700,#48701,#48702,#48703,#48704,#48705,
#48706,#48707,#48708,#48709,#48710,#48711,#48712,#48713,#48714,#48715,#48716,
#48717,#48718,#48719,#48720,#48721,#48722,#48723,#48724,#48725,#48726,#48727,
#48728,#48729,#48730,#48731,#48732,#48733,#48734,#48735,#48736,#48737,#48738,
#48739,#48740,#48741,#48742,#48743,#48744,#48745,#48746,#48747,#48748,#48749,
#48750,#48751,#48752,#48753,#48754,#48755,#48756,#48757,#48758,#48759,#48760,
#48761,#48762,#48763,#48764,#48765,#48766,#48767,#48768,#48769,#48770,#48771,
#48772,#48773,#48774,#48775,#48776,#48777,#48778,#48779,#48780,#48781,#48782,
#48783,#48784,#48785,#48786,#48787,#48788,#48789,#48790,#48791,#48792,#48793,
#48794,#48795,#48796,#48797,#48798,#48799,#48800,#48801,#48802,#48803,#48804,
#48805,#48806,#48807,#48808,#48809,#48810,#48811,#48812,#48813,#48814,#48815,
#48816,#48817,#48818,#48819,#48820,#48821,#48822,#48823,#48824,#48825,#48826,
#48827,#48828,#48829,#48830,#48831,#48832,#48833,#48834,#48835,#48836,#48837,
#48838,#48839,#48840,#48841,#48842),(#48843,#48844,#48845,#48846,#48847,
#48848,#48849,#48850,#48851,#48852,#48853,#48854,#48855,#48856,#48857,#48858,
#48859,#48860,#48861,#48862,#48863,#48864,#48865,#48866,#48867,#48868,#48869,
#48870,#48871,#48872,#48873,#48874,#48875,#48876,#48877,#48878,#48879,#48880,
#48881,#48882,#48883,#48884,#48885,#48886,#48887,#48888,#48889,#48890,#48891,
#48892,#48893,#48894,#48895,#48896,#48897,#48898,#48899,#48900,#48901,#48902,
#48903,#48904,#48905,#48906,#48907,#48908,#48909,#48910,#48911,#48912,#48913,
#48914,#48915,#48916,#48917,#48918,#48919,#48920,#48921,#48922,#48923,#48924,
#48925,#48926,#48927,#48928,#48929,#48930,#48931,#48932,#48933,#48934,#48935,
#48936,#48937,#48938,#48939,#48940,#48941,#48942,#48943,#48944,#48945,#48946,
#48947,#48948,#48949,#48950,#48951,#48952,#48953,#48954,#48955,#48956,#48957,
#48958,#48959,#48960,#48961,#48962,#48963,#48964,#48965,#48966,#48967,#48968,
#48969,#48970,#48971,#48972,#48973,#48974,#48975,#48976,#48977,#48978,#48979,
#48980,#48981,#48982,#48983,#48984,#48985,#48986,#48987,#48988,#48989,#48990,
#48991,#48992,#48993,#48994,#48995,#48996,#48997,#48998,#48999,#49000,#49001,
#49002,#49003,#49004,#49005,#49006,#49007,#49008,#49009,#49010,#49011,#49012,
#49013,#49014,#49015,#49016,#49017,#49018,#49019,#49020,#49021,#49022,#49023,
#49024,#49025,#49026,#49027,#49028,#49029,#49030,#49031,#49032,#49033,#49034,
#49035,#49036,#49037,#49038,#49039,#49040,#49041,#49042,#49043,#49044,#49045,
#49046,#49047,#49048,#49049,#49050,#49051,#49052,#49053,#49054,#49055,#49056,
#49057,#49058,#49059,#49060,#49061,#49062,#49063,#49064,#49065,#49066,#49067,
#49068,#49069,#49070,#49071,#49072,#49073,#49074,#49075,#49076,#49077,#49078,
#49079,#49080,#49081,#49082,#49083,#49084,#49085,#49086,#49087,#49088,#49089,
#49090,#49091,#49092,#49093,#49094,#49095,#49096,#49097,#49098,#49099,#49100,
#49101,#49102,#49103,#49104,#49105,#49106,#49107,#49108,#49109,#49110,#49111,
#49112,#49113,#49114,#49115,#49116,#49117,#49118,#49119,#49120,#49121,#49122,
#49123,#49124,#49125,#49126,#49127,#49128,#49129,#49130,#49131,#49132,#49133,
#49134,#49135,#49136,#49137,#49138,#49139,#49140,#49141,#49142,#49143,#49144,
#49145,#49146,#49147,#49148,#49149,#49150,#49151,#49152,#49153,#49154,#49155,
#49156,#49157,#49158,#49159,#49160,#49161,#49162,#49163,#49164,#49165,#49166,
#49167,#49168,#49169,#49170,#49171,#49172,#49173,#49174,#49175,#49176,#49177,
#49178,#49179,#49180,#49181,#49182,#49183,#49184,#49185,#49186,#49187,#49188,
#49189,#49190,#49191,#49192,#49193,#49194,#49195,#49196,#49197,#49198,#49199,
#49200,#49201,#49202,#49203,#49204,#49205,#49206,#49207,#49208,#49209,#49210,
#49211,#49212,#49213,#49214,#49215)),.UNSPECIFIED.,.F.,.F.,.F.,(4,4),(4,
1,1,1,1,1,1,1,1,1,1,1,1,1,1,1,1,1,1,1,1,1,1,1,1,1,1,1,1,1,1,1,1,1,1,1,1,
1,1,1,1,1,1,1,1,1,1,1,1,1,1,1,1,1,1,1,1,1,1,1,1,1,1,1,1,1,1,1,1,1,1,1,1,
1,1,1,1,1,1,1,1,1,1,1,1,1,1,1,1,1,1,1,1,1,1,1,1,1,1,1,1,1,1,1,1,1,1,1,1,
1,1,1,1,1,1,1,1,1,1,1,1,1,1,1,1,1,1,1,1,1,1,1,1,1,1,1,1,1,1,1,1,1,1,1,1,
1,1,1,1,1,1,1,1,1,1,1,1,1,1,1,1,1,1,1,1,1,1,1,1,1,1,1,1,1,1,1,1,1,1,1,1,
1,1,1,1,1,1,1,1,1,1,1,1,1,1,1,1,1,1,1,1,1,1,1,1,1,1,1,1,1,1,1,1,1,1,1,1,
1,1,1,1,1,1,1,1,1,1,1,1,1,1,1,1,1,1,1,1,1,1,1,1,1,1,1,1,1,1,1,1,1,1,1,1,
1,1,1,1,1,1,1,1,1,1,1,1,1,1,1,1,1,1,1,1,1,1,1,1,1,1,1,1,1,1,1,1,1,1,1,1,
1,1,1,1,1,1,1,1,1,1,1,1,1,1,1,1,1,1,1,1,1,1,1,1,1,1,1,1,1,1,1,1,1,1,1,1,
1,1,1,1,1,1,1,1,1,1,1,1,1,1,1,1,1,1,1,1,1,1,1,1,1,1,1,1,1,1,1,1,1,1,1,1,
1,1,1,1,1,1,1,1,1,4),(0.,0.0329955678841869),(15.385850931809,16.3845370113689,
17.3832230909289,18.3819091704888,19.3805952500488,20.3792813296087,21.3779674091687,
22.3766534887286,23.3753395682886,24.3740256478485,25.3727117274085,26.3713978069684,
27.3700838865284,28.3687699660883,29.3674560456483,30.3661421252082,31.3648282047682,
32.3635142843282,33.3622003638881,34.3608864434481,35.359572523008,36.358258602568,
37.3569446821279,38.3556307616879,39.3543168412478,40.3530029208078,41.3516890003677,
42.3503750799277,43.3490611594876,44.3477472390476,45.3464333186075,46.3451193981675,
47.3438054777274,48.3424915572874,49.3411776368473,50.3398637164073,51.3385497959672,
52.3372358755272,53.3359219550871,54.3346080346471,55.333294114207,56.331980193767,
57.3306662733269,58.3293523528869,59.3280384324468,60.3267245120068,61.3254105915667,
62.3240966711267,63.3227827506866,64.3214688302466,65.3201549098065,66.3188409893665,
67.3175270689264,68.3162131484864,69.3148992280463,70.3135853076063,71.3122713871662,
72.3109574667262,73.3096435462861,74.3083296258461,75.307015705406,76.305701784966,
77.3043878645259,78.3030739440859,79.3017600236459,80.3004461032058,81.2991321827658,
82.2978182623257,83.2965043418857,84.2951904214456,85.2938765010056,86.2925625805655,
87.2912486601255,88.2899347396854,89.2886208192454,90.2873068988053,91.2859929783653,
92.2846790579252,93.2833651374852,94.2820512170451,95.2807372966051,96.279423376165,
97.278109455725,98.2767955352849,99.2754816148449,100.274167694405,101.272853773965,
102.271539853525,103.270225933085,104.268912012645,105.267598092205,106.266284171765,
107.264970251324,108.263656330884,109.262342410444,110.261028490004,111.259714569564,
112.258400649124,113.257086728684,114.255772808244,115.254458887804,116.253144967364,
117.251831046924,118.250517126484,119.249203206044,120.247889285604,121.246575365164,
122.245261444724,123.243947524284,124.242633603844,125.241319683404,126.240005762964,
127.238691842524,128.237377922083,129.236064001643,130.234750081203,131.233436160763,
132.232122240323,133.230808319883,134.229494399443,135.228180479003,136.226866558563,
137.225552638123,138.224238717683,139.222924797243,140.221610876803,141.220296956363,
142.218983035923,143.217669115483,144.216355195043,145.215041274603,146.213727354163,
147.212413433723,148.211099513282,149.209785592842,150.208471672402,151.207157751962,
152.205843831522,153.204529911082,154.203215990642,155.201902070202,156.200588149762,
157.199274229322,158.197960308882,159.196646388442,160.195332468002,161.194018547562,
162.192704627122,163.191390706682,164.190076786242,165.188762865802,166.187448945362,
167.186135024922,168.184821104482,169.183507184041,170.182193263601,171.180879343161,
172.179565422721,173.178251502281,174.176937581841,175.175623661401,176.174309740961,
177.172995820521,178.171681900081,179.170367979641,180.169054059201,181.167740138761,
182.166426218321,183.165112297881,184.163798377441,185.162484457001,186.161170536561,
187.159856616121,188.158542695681,189.15722877524,190.1559148548,191.15460093436,
192.15328701392,193.15197309348,194.15065917304,195.1493452526,196.14803133216,
197.14671741172,198.14540349128,199.14408957084,200.1427756504,201.14146172996,
202.14014780952,203.13883388908,204.13751996864,205.1362060482,206.13489212776,
207.13357820732,208.13226428688,209.130950366439,210.129636445999,211.128322525559,
212.127008605119,213.125694684679,214.124380764239,215.123066843799,216.121752923359,
217.120439002919,218.119125082479,219.117811162039,220.116497241599,221.115183321159,
222.113869400719,223.112555480279,224.111241559839,225.109927639399,226.108613718959,
227.107299798519,228.105985878079,229.104671957639,230.103358037198,231.102044116758,
232.100730196318,233.099416275878,234.098102355438,235.096788434998,236.095474514558,
237.094160594118,238.092846673678,239.091532753238,240.090218832798,241.088904912358,
242.087590991918,243.086277071478,244.084963151038,245.083649230598,246.082335310158,
247.081021389718,248.079707469278,249.078393548838,250.077079628397,251.075765707957,
252.074451787517,253.073137867077,254.071823946637,255.070510026197,256.069196105757,
257.067882185317,258.066568264877,259.065254344437,260.063940423997,261.062626503557,
262.061312583117,263.059998662677,264.058684742237,265.057370821797,266.056056901357,
267.054742980917,268.053429060477,269.052115140037,270.050801219597,271.049487299156,
272.048173378716,273.046859458276,274.045545537836,275.044231617396,276.042917696956,
277.041603776516,278.040289856076,279.038975935636,280.037662015196,281.036348094756,
282.035034174316,283.033720253876,284.032406333436,285.031092412996,286.029778492556,
287.028464572116,288.027150651676,289.025836731236,290.024522810796,291.023208890355,
292.021894969915,293.020581049475,294.019267129035,295.017953208595,296.016639288155,
297.015325367715,298.014011447275,299.012697526835,300.011383606395,301.010069685955,
302.008755765515,303.007441845075,304.006127924635,305.004814004195,306.003500083755,
307.002186163315,308.000872242875,308.999558322435,309.998244401995,310.996930481555,
311.995616561114,312.994302640674,313.992988720234,314.991674799794,315.990360879354,
316.989046958914,317.987733038474,318.986419118034,319.985105197594,320.983791277154,
321.982477356714,322.981163436274,323.979849515834,324.978535595394,325.977221674954,
326.975907754514,327.974593834074,328.973279913634,329.971965993194,330.970652072754,
331.969338152313,332.968024231873,333.966710311433,334.965396390993,335.964082470553,
336.962768550113,337.961454629673,338.960140709233,339.958826788793,340.957512868353,
341.956198947913,342.954885027473,343.953571107033,344.952257186593,345.950943266153,
346.949629345713,347.948315425273,348.947001504833,349.945687584393,350.944373663953,
351.943059743512,352.941745823072,353.940431902632,354.939117982192,355.937804061752,
356.936490141312,357.935176220872,358.933862300432,359.932548379992,360.931234459552,
361.929920539112,362.928606618672,363.927292698232,364.925978777792,365.924664857352,
366.923350936912,367.922037016472,368.920723096032,369.919409175592,370.918095255152,
371.916781334712,372.915467414271,373.914153493831,374.912839573391,375.911525652951,
376.910211732511,377.908897812071,378.907583891631,379.906269971191,380.904956050751,
381.903642130311,382.902328209871,383.901014289431,384.899700368991),
 .UNSPECIFIED.);
#371=B_SPLINE_SURFACE_WITH_KNOTS('',3,3,((#51566,#51567,#51568,#51569,#51570,
#51571,#51572,#51573,#51574,#51575,#51576,#51577,#51578,#51579,#51580,#51581,
#51582,#51583,#51584,#51585,#51586,#51587,#51588,#51589,#51590,#51591,#51592,
#51593,#51594,#51595,#51596,#51597,#51598,#51599,#51600,#51601,#51602,#51603,
#51604,#51605,#51606,#51607,#51608,#51609,#51610,#51611,#51612,#51613,#51614,
#51615,#51616,#51617,#51618,#51619,#51620,#51621,#51622,#51623,#51624,#51625,
#51626,#51627,#51628,#51629,#51630,#51631,#51632,#51633,#51634,#51635,#51636,
#51637,#51638,#51639,#51640,#51641,#51642,#51643,#51644,#51645,#51646,#51647,
#51648,#51649,#51650,#51651,#51652,#51653,#51654,#51655,#51656,#51657,#51658,
#51659,#51660,#51661,#51662,#51663,#51664,#51665,#51666,#51667,#51668,#51669,
#51670,#51671,#51672,#51673,#51674,#51675,#51676,#51677,#51678,#51679,#51680,
#51681,#51682,#51683,#51684,#51685,#51686,#51687,#51688),(#51689,#51690,
#51691,#51692,#51693,#51694,#51695,#51696,#51697,#51698,#51699,#51700,#51701,
#51702,#51703,#51704,#51705,#51706,#51707,#51708,#51709,#51710,#51711,#51712,
#51713,#51714,#51715,#51716,#51717,#51718,#51719,#51720,#51721,#51722,#51723,
#51724,#51725,#51726,#51727,#51728,#51729,#51730,#51731,#51732,#51733,#51734,
#51735,#51736,#51737,#51738,#51739,#51740,#51741,#51742,#51743,#51744,#51745,
#51746,#51747,#51748,#51749,#51750,#51751,#51752,#51753,#51754,#51755,#51756,
#51757,#51758,#51759,#51760,#51761,#51762,#51763,#51764,#51765,#51766,#51767,
#51768,#51769,#51770,#51771,#51772,#51773,#51774,#51775,#51776,#51777,#51778,
#51779,#51780,#51781,#51782,#51783,#51784,#51785,#51786,#51787,#51788,#51789,
#51790,#51791,#51792,#51793,#51794,#51795,#51796,#51797,#51798,#51799,#51800,
#51801,#51802,#51803,#51804,#51805,#51806,#51807,#51808,#51809,#51810,#51811),
(#51812,#51813,#51814,#51815,#51816,#51817,#51818,#51819,#51820,#51821,
#51822,#51823,#51824,#51825,#51826,#51827,#51828,#51829,#51830,#51831,#51832,
#51833,#51834,#51835,#51836,#51837,#51838,#51839,#51840,#51841,#51842,#51843,
#51844,#51845,#51846,#51847,#51848,#51849,#51850,#51851,#51852,#51853,#51854,
#51855,#51856,#51857,#51858,#51859,#51860,#51861,#51862,#51863,#51864,#51865,
#51866,#51867,#51868,#51869,#51870,#51871,#51872,#51873,#51874,#51875,#51876,
#51877,#51878,#51879,#51880,#51881,#51882,#51883,#51884,#51885,#51886,#51887,
#51888,#51889,#51890,#51891,#51892,#51893,#51894,#51895,#51896,#51897,#51898,
#51899,#51900,#51901,#51902,#51903,#51904,#51905,#51906,#51907,#51908,#51909,
#51910,#51911,#51912,#51913,#51914,#51915,#51916,#51917,#51918,#51919,#51920,
#51921,#51922,#51923,#51924,#51925,#51926,#51927,#51928,#51929,#51930,#51931,
#51932,#51933,#51934),(#51935,#51936,#51937,#51938,#51939,#51940,#51941,
#51942,#51943,#51944,#51945,#51946,#51947,#51948,#51949,#51950,#51951,#51952,
#51953,#51954,#51955,#51956,#51957,#51958,#51959,#51960,#51961,#51962,#51963,
#51964,#51965,#51966,#51967,#51968,#51969,#51970,#51971,#51972,#51973,#51974,
#51975,#51976,#51977,#51978,#51979,#51980,#51981,#51982,#51983,#51984,#51985,
#51986,#51987,#51988,#51989,#51990,#51991,#51992,#51993,#51994,#51995,#51996,
#51997,#51998,#51999,#52000,#52001,#52002,#52003,#52004,#52005,#52006,#52007,
#52008,#52009,#52010,#52011,#52012,#52013,#52014,#52015,#52016,#52017,#52018,
#52019,#52020,#52021,#52022,#52023,#52024,#52025,#52026,#52027,#52028,#52029,
#52030,#52031,#52032,#52033,#52034,#52035,#52036,#52037,#52038,#52039,#52040,
#52041,#52042,#52043,#52044,#52045,#52046,#52047,#52048,#52049,#52050,#52051,
#52052,#52053,#52054,#52055,#52056,#52057)),.UNSPECIFIED.,.F.,.F.,.F.,(4,
4),(4,1,1,1,1,1,1,1,1,1,1,1,1,1,1,1,1,1,1,1,1,1,1,1,1,1,1,1,1,1,1,1,1,1,
1,1,1,1,1,1,1,1,1,1,1,1,1,1,1,1,1,1,1,1,1,1,1,1,1,1,1,1,1,1,1,1,1,1,1,1,
1,1,1,1,1,1,1,1,1,1,1,1,1,1,1,1,1,1,1,1,1,1,1,1,1,1,1,1,1,1,1,1,1,1,1,1,
1,1,1,1,1,1,1,1,1,1,1,1,1,1,4),(0.,0.0526254770366343),(10.6643522173549,
11.6633215686903,12.6622909200256,13.661260271361,14.6602296226963,15.6591989740317,
16.658168325367,17.6571376767024,18.6561070280377,19.6550763793731,20.6540457307084,
21.6530150820438,22.6519844333791,23.6509537847144,24.6499231360498,25.6488924873851,
26.6478618387205,27.6468311900558,28.6458005413912,29.6447698927265,30.6437392440619,
31.6427085953972,32.6416779467326,33.6406472980679,34.6396166494033,35.6385860007386,
36.6375553520739,37.6365247034093,38.6354940547446,39.63446340608,40.6334327574153,
41.6324021087507,42.631371460086,43.6303408114214,44.6293101627567,45.6282795140921,
46.6272488654274,47.6262182167628,48.6251875680981,49.6241569194335,50.6231262707688,
51.6220956221041,52.6210649734395,53.6200343247748,54.6190036761102,55.6179730274455,
56.6169423787809,57.6159117301162,58.6148810814516,59.6138504327869,60.6128197841223,
61.6117891354576,62.610758486793,63.6097278381283,64.6086971894637,65.607666540799,
66.6066358921343,67.6056052434697,68.604574594805,69.6035439461404,70.6025132974757,
71.6014826488111,72.6004520001464,73.5994213514818,74.5983907028171,75.5973600541525,
76.5963294054878,77.5952987568232,78.5942681081585,79.5932374594938,80.5922068108292,
81.5911761621645,82.5901455134999,83.5891148648352,84.5880842161706,85.5870535675059,
86.5860229188413,87.5849922701766,88.583961621512,89.5829309728473,90.5819003241827,
91.580869675518,92.5798390268534,93.5788083781887,94.5777777295241,95.5767470808594,
96.5757164321948,97.5746857835301,98.5736551348654,99.5726244862008,100.571593837536,
101.570563188871,102.569532540207,103.568501891542,104.567471242878,105.566440594213,
106.565409945548,107.564379296884,108.563348648219,109.562317999554,110.56128735089,
111.560256702225,112.55922605356,113.558195404896,114.557164756231,115.556134107566,
116.555103458902,117.554072810237,118.553042161572,119.552011512908,120.550980864243,
121.549950215578,122.548919566914,123.547888918249,124.546858269584,125.54582762092,
126.544796972255,127.54376632359,128.542735674926,129.541705026261,130.540674377597),
 .UNSPECIFIED.);
#372=B_SPLINE_SURFACE_WITH_KNOTS('',3,3,((#52213,#52214,#52215,#52216,#52217,
#52218,#52219,#52220,#52221,#52222,#52223,#52224,#52225,#52226,#52227,#52228,
#52229,#52230,#52231,#52232,#52233,#52234,#52235,#52236,#52237,#52238,#52239,
#52240,#52241,#52242,#52243,#52244,#52245,#52246,#52247,#52248,#52249,#52250,
#52251,#52252,#52253,#52254,#52255,#52256,#52257,#52258,#52259,#52260,#52261,
#52262,#52263,#52264,#52265,#52266,#52267,#52268,#52269,#52270,#52271,#52272,
#52273,#52274,#52275,#52276,#52277,#52278,#52279,#52280,#52281,#52282,#52283,
#52284,#52285,#52286,#52287,#52288,#52289,#52290,#52291,#52292,#52293,#52294,
#52295,#52296,#52297,#52298,#52299,#52300,#52301,#52302,#52303,#52304,#52305,
#52306,#52307,#52308,#52309,#52310,#52311,#52312,#52313,#52314,#52315,#52316,
#52317,#52318,#52319,#52320,#52321,#52322,#52323,#52324,#52325,#52326,#52327,
#52328,#52329,#52330,#52331,#52332,#52333,#52334,#52335),(#52336,#52337,
#52338,#52339,#52340,#52341,#52342,#52343,#52344,#52345,#52346,#52347,#52348,
#52349,#52350,#52351,#52352,#52353,#52354,#52355,#52356,#52357,#52358,#52359,
#52360,#52361,#52362,#52363,#52364,#52365,#52366,#52367,#52368,#52369,#52370,
#52371,#52372,#52373,#52374,#52375,#52376,#52377,#52378,#52379,#52380,#52381,
#52382,#52383,#52384,#52385,#52386,#52387,#52388,#52389,#52390,#52391,#52392,
#52393,#52394,#52395,#52396,#52397,#52398,#52399,#52400,#52401,#52402,#52403,
#52404,#52405,#52406,#52407,#52408,#52409,#52410,#52411,#52412,#52413,#52414,
#52415,#52416,#52417,#52418,#52419,#52420,#52421,#52422,#52423,#52424,#52425,
#52426,#52427,#52428,#52429,#52430,#52431,#52432,#52433,#52434,#52435,#52436,
#52437,#52438,#52439,#52440,#52441,#52442,#52443,#52444,#52445,#52446,#52447,
#52448,#52449,#52450,#52451,#52452,#52453,#52454,#52455,#52456,#52457,#52458),
(#52459,#52460,#52461,#52462,#52463,#52464,#52465,#52466,#52467,#52468,
#52469,#52470,#52471,#52472,#52473,#52474,#52475,#52476,#52477,#52478,#52479,
#52480,#52481,#52482,#52483,#52484,#52485,#52486,#52487,#52488,#52489,#52490,
#52491,#52492,#52493,#52494,#52495,#52496,#52497,#52498,#52499,#52500,#52501,
#52502,#52503,#52504,#52505,#52506,#52507,#52508,#52509,#52510,#52511,#52512,
#52513,#52514,#52515,#52516,#52517,#52518,#52519,#52520,#52521,#52522,#52523,
#52524,#52525,#52526,#52527,#52528,#52529,#52530,#52531,#52532,#52533,#52534,
#52535,#52536,#52537,#52538,#52539,#52540,#52541,#52542,#52543,#52544,#52545,
#52546,#52547,#52548,#52549,#52550,#52551,#52552,#52553,#52554,#52555,#52556,
#52557,#52558,#52559,#52560,#52561,#52562,#52563,#52564,#52565,#52566,#52567,
#52568,#52569,#52570,#52571,#52572,#52573,#52574,#52575,#52576,#52577,#52578,
#52579,#52580,#52581),(#52582,#52583,#52584,#52585,#52586,#52587,#52588,
#52589,#52590,#52591,#52592,#52593,#52594,#52595,#52596,#52597,#52598,#52599,
#52600,#52601,#52602,#52603,#52604,#52605,#52606,#52607,#52608,#52609,#52610,
#52611,#52612,#52613,#52614,#52615,#52616,#52617,#52618,#52619,#52620,#52621,
#52622,#52623,#52624,#52625,#52626,#52627,#52628,#52629,#52630,#52631,#52632,
#52633,#52634,#52635,#52636,#52637,#52638,#52639,#52640,#52641,#52642,#52643,
#52644,#52645,#52646,#52647,#52648,#52649,#52650,#52651,#52652,#52653,#52654,
#52655,#52656,#52657,#52658,#52659,#52660,#52661,#52662,#52663,#52664,#52665,
#52666,#52667,#52668,#52669,#52670,#52671,#52672,#52673,#52674,#52675,#52676,
#52677,#52678,#52679,#52680,#52681,#52682,#52683,#52684,#52685,#52686,#52687,
#52688,#52689,#52690,#52691,#52692,#52693,#52694,#52695,#52696,#52697,#52698,
#52699,#52700,#52701,#52702,#52703,#52704)),.UNSPECIFIED.,.F.,.F.,.F.,(4,
4),(4,1,1,1,1,1,1,1,1,1,1,1,1,1,1,1,1,1,1,1,1,1,1,1,1,1,1,1,1,1,1,1,1,1,
1,1,1,1,1,1,1,1,1,1,1,1,1,1,1,1,1,1,1,1,1,1,1,1,1,1,1,1,1,1,1,1,1,1,1,1,
1,1,1,1,1,1,1,1,1,1,1,1,1,1,1,1,1,1,1,1,1,1,1,1,1,1,1,1,1,1,1,1,1,1,1,1,
1,1,1,1,1,1,1,1,1,1,1,1,1,1,4),(0.,0.0526254770366343),(13.9725876875337,
14.9715570388691,15.9705263902044,16.9694957415398,17.9684650928751,18.9674344442105,
19.9664037955458,20.9653731468812,21.9643424982165,22.9633118495519,23.9622812008872,
24.9612505522226,25.9602199035579,26.9591892548932,27.9581586062286,28.9571279575639,
29.9560973088993,30.9550666602346,31.95403601157,32.9530053629053,33.9519747142407,
34.950944065576,35.9499134169114,36.9488827682467,37.9478521195821,38.9468214709174,
39.9457908222528,40.9447601735881,41.9437295249234,42.9426988762588,43.9416682275941,
44.9406375789295,45.9396069302648,46.9385762816002,47.9375456329355,48.9365149842709,
49.9354843356062,50.9344536869416,51.9334230382769,52.9323923896123,53.9313617409476,
54.930331092283,55.9293004436183,56.9282697949536,57.927239146289,58.9262084976243,
59.9251778489597,60.924147200295,61.9231165516304,62.9220859029657,63.9210552543011,
64.9200246056364,65.9189939569718,66.9179633083071,67.9169326596425,68.9159020109778,
69.9148713623132,70.9138407136485,71.9128100649839,72.9117794163192,73.9107487676546,
74.9097181189899,75.9086874703252,76.9076568216606,77.9066261729959,78.9055955243313,
79.9045648756666,80.903534227002,81.9025035783373,82.9014729296727,83.900442281008,
84.8994116323434,85.8983809836787,86.8973503350141,87.8963196863494,88.8952890376847,
89.8942583890201,90.8932277403554,91.8921970916908,92.8911664430261,93.8901357943615,
94.8891051456968,95.8880744970322,96.8870438483675,97.8860131997029,98.8849825510382,
99.8839519023736,100.882921253709,101.881890605044,102.88085995638,103.879829307715,
104.87879865905,105.877768010386,106.876737361721,107.875706713056,108.874676064392,
109.873645415727,110.872614767062,111.871584118398,112.870553469733,113.869522821068,
114.868492172404,115.867461523739,116.866430875074,117.86540022641,118.864369577745,
119.863338929081,120.862308280416,121.861277631751,122.860246983087,123.859216334422,
124.858185685757,125.857155037093,126.856124388428,127.855093739763,128.854063091099,
129.853032442434,130.852001793769,131.850971145105,132.84994049644,133.848909847775),
 .UNSPECIFIED.);
#373=B_SPLINE_CURVE_WITH_KNOTS('',3,(#33239,#33240,#33241,#33242,#33243,
#33244,#33245,#33246,#33247,#33248,#33249,#33250,#33251,#33252,#33253,#33254,
#33255,#33256,#33257,#33258,#33259,#33260,#33261,#33262,#33263),
 .UNSPECIFIED.,.F.,.F.,(4,3,3,3,3,3,3,3,4),(-9.15304944749145,-8.88450116749033,
-7.89733437110252,-6.9101675747147,-5.92300077832689,-4.93583398193907,
-3.94866718555126,-2.96150038916344,-2.86986414031186),.UNSPECIFIED.);
#374=B_SPLINE_CURVE_WITH_KNOTS('',3,(#33268,#33269,#33270,#33271),
 .UNSPECIFIED.,.F.,.F.,(4,4),(-2.86986414031186,-2.08103247056473),
 .UNSPECIFIED.);
#375=B_SPLINE_CURVE_WITH_KNOTS('',3,(#33274,#33275,#33276,#33277,#33278,
#33279,#33280,#33281,#33282,#33283,#33284,#33285,#33286,#33287,#33288,#33289,
#33290,#33291,#33292,#33293,#33294,#33295),.UNSPECIFIED.,.F.,.F.,(4,3,3,
3,3,3,3,4),(0.,0.98716679638781,1.97433359277563,2.96150038916344,3.94866718555125,
4.93583398193907,5.92300077832688,6.18969281142703),.UNSPECIFIED.);
#376=B_SPLINE_CURVE_WITH_KNOTS('',3,(#33300,#33301,#33302,#33303,#33304,
#33305,#33306,#33307,#33308,#33309,#33310,#33311,#33312,#33313,#33314,#33315,
#33316,#33317,#33318,#33319,#33320,#33321),.UNSPECIFIED.,.F.,.F.,(4,3,3,
3,3,3,3,4),(-15.436234754671,-14.8075019458172,-13.8203351494294,-12.8331683530416,
-11.8460015566538,-10.858834760266,-9.87166796387814,-9.15304944749145),
 .UNSPECIFIED.);
#377=B_SPLINE_CURVE_WITH_KNOTS('',3,(#33322,#33323,#33324,#33325,#33326,
#33327,#33328,#33329,#33330,#33331,#33332,#33333,#33334,#33335,#33336,#33337,
#33338,#33339,#33340,#33341,#33342,#33343),.UNSPECIFIED.,.F.,.F.,(4,3,3,
3,3,3,3,4),(6.18969281142703,6.9101675747147,7.89733437110251,8.88450116749032,
9.87166796387814,10.858834760266,11.8460015566538,12.4728781186066),
 .UNSPECIFIED.);
#378=B_SPLINE_CURVE_WITH_KNOTS('',3,(#33348,#33349,#33350,#33351,#33352,
#33353,#33354,#33355,#33356,#33357,#33358,#33359,#33360,#33361,#33362,#33363,
#33364,#33365,#33366,#33367,#33368,#33369),.UNSPECIFIED.,.F.,.F.,(4,3,3,
3,3,3,3,4),(-21.7194200618506,-20.7305027241441,-19.7433359277563,-18.7561691313685,
-17.7690023349807,-16.7818355385928,-15.794668742205,-15.436234754671),
 .UNSPECIFIED.);
#379=B_SPLINE_CURVE_WITH_KNOTS('',3,(#33370,#33371,#33372,#33373,#33374,
#33375,#33376,#33377,#33378,#33379,#33380,#33381,#33382,#33383,#33384,#33385,
#33386,#33387,#33388,#33389,#33390,#33391),.UNSPECIFIED.,.F.,.F.,(4,3,3,
3,3,3,3,4),(12.4728781186066,12.8331683530416,13.8203351494294,14.8075019458172,
15.794668742205,16.7818355385928,17.7690023349807,18.7560634257862),
 .UNSPECIFIED.);
#380=B_SPLINE_CURVE_WITH_KNOTS('',3,(#33396,#33397,#33398,#33399,#33400,
#33401,#33402,#33403,#33404,#33405,#33406,#33407,#33408,#33409,#33410,#33411,
#33412,#33413,#33414,#33415,#33416,#33417),.UNSPECIFIED.,.F.,.F.,(4,3,3,
3,3,3,3,4),(-28.0026053690302,-27.6406702988588,-26.653503502471,-25.6663367060832,
-24.6791699096953,-23.6920031133075,-22.7048363169197,-21.7194200618506),
 .UNSPECIFIED.);
#381=B_SPLINE_CURVE_WITH_KNOTS('',3,(#33418,#33419,#33420,#33421,#33422,
#33423,#33424,#33425,#33426,#33427,#33428,#33429,#33430,#33431,#33432,#33433,
#33434,#33435,#33436,#33437,#33438,#33439),.UNSPECIFIED.,.F.,.F.,(4,3,3,
3,3,3,3,4),(18.7560634257862,19.7433359277563,20.7305027241441,21.7176695205319,
22.7048363169197,23.6920031133075,24.6791699096954,25.0392487329658),
 .UNSPECIFIED.);
#382=B_SPLINE_CURVE_WITH_KNOTS('',3,(#33444,#33445,#33446,#33447,#33448,
#33449,#33450,#33451,#33452,#33453,#33454,#33455,#33456,#33457,#33458,#33459,
#33460,#33461,#33462,#33463,#33464,#33465),.UNSPECIFIED.,.F.,.F.,(4,3,3,
3,3,3,3,4),(-34.2857906762098,-33.5636710771857,-32.5765042807979,-31.58933748441,
-30.6021706880222,-29.6150038916344,-28.6278370952466,-28.0026053690302),
 .UNSPECIFIED.);
#383=B_SPLINE_CURVE_WITH_KNOTS('',3,(#33466,#33467,#33468,#33469,#33470,
#33471,#33472,#33473,#33474,#33475,#33476,#33477,#33478,#33479,#33480,#33481,
#33482,#33483,#33484,#33485,#33486,#33487),.UNSPECIFIED.,.F.,.F.,(4,3,3,
3,3,3,3,4),(25.0392487329658,25.6663367060832,26.653503502471,27.6406702988588,
28.6278370952466,29.6150038916344,30.6021706880222,31.3224340401454),
 .UNSPECIFIED.);
#384=B_SPLINE_CURVE_WITH_KNOTS('',3,(#33492,#33493,#33494,#33495,#33496,
#33497,#33498,#33499,#33500,#33501,#33502,#33503,#33504,#33505,#33506,#33507,
#33508,#33509,#33510,#33511,#33512,#33513,#33514,#33515,#33516),
 .UNSPECIFIED.,.F.,.F.,(4,3,3,3,3,3,3,3,4),(-40.5689759833894,-40.4738386519004,
-39.4866718555126,-38.4995050591247,-37.5123382627369,-36.5251714663491,
-35.5380046699613,-34.5508378735735,-34.2857906762098),.UNSPECIFIED.);
#385=B_SPLINE_CURVE_WITH_KNOTS('',3,(#33517,#33518,#33519,#33520,#33521,
#33522,#33523,#33524,#33525,#33526,#33527,#33528,#33529,#33530,#33531,#33532,
#33533,#33534,#33535,#33536,#33537,#33538,#33539,#33540,#33541),
 .UNSPECIFIED.,.F.,.F.,(4,3,3,3,3,3,3,3,4),(31.3224340401454,31.58933748441,
32.5765042807979,33.5636710771857,34.5508378735735,35.5380046699613,36.5251714663491,
37.5123382627369,37.605619347325),.UNSPECIFIED.);
#386=B_SPLINE_CURVE_WITH_KNOTS('',3,(#33546,#33547,#33548,#33549,#33550,
#33551,#33552,#33553,#33554,#33555,#33556,#33557,#33558,#33559,#33560,#33561,
#33562,#33563,#33564,#33565,#33566,#33567),.UNSPECIFIED.,.F.,.F.,(4,3,3,
3,3,3,3,4),(-46.852161290569,-46.3968394302273,-45.4096726338394,-44.4225058374516,
-43.4353390410638,-42.448172244676,-41.4610054482882,-40.5689759833894),
 .UNSPECIFIED.);
#387=B_SPLINE_CURVE_WITH_KNOTS('',3,(#33568,#33569,#33570,#33571,#33572,
#33573,#33574,#33575,#33576,#33577,#33578,#33579,#33580,#33581,#33582,#33583,
#33584,#33585,#33586,#33587,#33588,#33589),.UNSPECIFIED.,.F.,.F.,(4,3,3,
3,3,3,3,4),(37.605619347325,38.4995050591248,39.4866718555126,40.4738386519004,
41.4610054482882,42.448172244676,43.4353390410638,43.8888046545046),
 .UNSPECIFIED.);
#388=B_SPLINE_CURVE_WITH_KNOTS('',3,(#33594,#33595,#33596,#33597,#33598,
#33599,#33600,#33601,#33602,#33603,#33604,#33605,#33606,#33607,#33608,#33609,
#33610,#33611,#33612,#33613,#33614,#33615),.UNSPECIFIED.,.F.,.F.,(4,3,3,
3,3,3,3,4),(-53.1353465977486,-52.3198402085541,-51.3326734121663,-50.3455066157785,
-49.3583398193907,-48.3711730230029,-47.3840062266151,-46.852161290569),
 .UNSPECIFIED.);
#389=B_SPLINE_CURVE_WITH_KNOTS('',3,(#33616,#33617,#33618,#33619,#33620,
#33621,#33622,#33623,#33624,#33625,#33626,#33627,#33628,#33629,#33630,#33631,
#33632,#33633,#33634,#33635,#33636,#33637),.UNSPECIFIED.,.F.,.F.,(4,3,3,
3,3,3,3,4),(43.8888046545046,44.4225058374516,45.4096726338394,46.3968394302273,
47.3840062266151,48.3711730230029,49.3583398193907,50.1719899616841),
 .UNSPECIFIED.);
#390=B_SPLINE_CURVE_WITH_KNOTS('',3,(#33642,#33643,#33644,#33645,#33646,
#33647,#33648,#33649,#33650,#33651,#33652,#33653,#33654,#33655,#33656,#33657,
#33658,#33659,#33660,#33661,#33662,#33663,#33664,#33665,#33666),
 .UNSPECIFIED.,.F.,.F.,(4,3,3,3,3,3,3,3,4),(-59.4185319049282,-59.2300077832689,
-58.242840986881,-57.2556741904932,-56.2685073941054,-55.2813405977176,
-54.2941738013298,-53.307007004942,-53.1353465977486),.UNSPECIFIED.);
#391=B_SPLINE_CURVE_WITH_KNOTS('',3,(#33667,#33668,#33669,#33670,#33671,
#33672,#33673,#33674,#33675,#33676,#33677,#33678,#33679,#33680,#33681,#33682,
#33683,#33684,#33685,#33686,#33687,#33688,#33689,#33690,#33691),
 .UNSPECIFIED.,.F.,.F.,(4,3,3,3,3,3,3,3,4),(50.1719899616841,50.3455066157785,
51.3326734121663,52.3198402085541,53.307007004942,54.2941738013298,55.2813405977176,
56.2685073941054,56.4551752688637),.UNSPECIFIED.);
#392=B_SPLINE_CURVE_WITH_KNOTS('',3,(#33696,#33697,#33698,#33699,#33700,
#33701,#33702,#33703,#33704,#33705,#33706,#33707,#33708,#33709,#33710,#33711,
#33712,#33713,#33714,#33715,#33716,#33717),.UNSPECIFIED.,.F.,.F.,(4,3,3,
3,3,3,3,4),(-65.7017172121077,-65.1530085615957,-64.1658417652079,-63.1786749688201,
-62.1915081724323,-61.2043413760445,-60.2171745796567,-59.4185319049282),
 .UNSPECIFIED.);
#393=B_SPLINE_CURVE_WITH_KNOTS('',3,(#33718,#33719,#33720,#33721,#33722,
#33723,#33724,#33725,#33726,#33727,#33728,#33729,#33730,#33731,#33732,#33733,
#33734,#33735,#33736,#33737,#33738,#33739),.UNSPECIFIED.,.F.,.F.,(4,3,3,
3,3,3,3,4),(56.4551752688637,57.2556741904932,58.242840986881,59.2300077832688,
60.2171745796566,61.2043413760445,62.1915081724323,62.7383605760433),
 .UNSPECIFIED.);
#394=B_SPLINE_CURVE_WITH_KNOTS('',3,(#33745,#33746,#33747,#33748,#33749),
 .UNSPECIFIED.,.F.,.F.,(4,1,4),(78.5398163397448,78.9782744856206,79.8587424042193),
 .UNSPECIFIED.);
#395=B_SPLINE_CURVE_WITH_KNOTS('',3,(#33752,#33753,#33754,#33755),
 .UNSPECIFIED.,.F.,.F.,(4,4),(78.5398163397448,78.6199462036688),
 .UNSPECIFIED.);
#396=B_SPLINE_CURVE_WITH_KNOTS('',3,(#33760,#33761,#33762,#33763,#33764,
#33765,#33766,#33767,#33768,#33769),.UNSPECIFIED.,.F.,.F.,(4,1,1,1,1,1,
1,4),(72.2566310325652,73.0552737072937,74.0424405036815,75.0296073000693,
76.0167740964572,77.003940892845,77.9911076892328,78.5398163397448),
 .UNSPECIFIED.);
#397=B_SPLINE_CURVE_WITH_KNOTS('',3,(#33770,#33771,#33772,#33773,#33774,
#33775,#33776,#33777,#33778,#33779),.UNSPECIFIED.,.F.,.F.,(4,1,1,1,1,1,
1,4),(72.2566310325652,72.696945425342,73.6841122217298,74.6712790181176,
75.6584458145054,76.6456126108932,77.632779407281,78.5398163397448),
 .UNSPECIFIED.);
#398=B_SPLINE_CURVE_WITH_KNOTS('',3,(#33784,#33785,#33786,#33787,#33788,
#33789,#33790,#33791,#33792,#33793,#33794),.UNSPECIFIED.,.F.,.F.,(4,1,1,
1,1,1,1,1,4),(65.9734457253856,66.145106132579,67.1322729289668,68.1194397253546,
69.1066065217424,70.0937733181303,71.0809401145181,72.0681069109059,72.2566310325652),
 .UNSPECIFIED.);
#399=B_SPLINE_CURVE_WITH_KNOTS('',3,(#33795,#33796,#33797,#33798,#33799,
#33800,#33801,#33802,#33803,#33804),.UNSPECIFIED.,.F.,.F.,(4,1,1,1,1,1,
1,4),(65.9734457253856,66.7739446470151,67.7611114434029,68.7482782397907,
69.7354450361785,70.7226118325663,71.7097786289541,72.2566310325652),
 .UNSPECIFIED.);
#400=B_SPLINE_CURVE_WITH_KNOTS('',3,(#33809,#33810,#33811,#33812,#33813,
#33814,#33815,#33816,#33817,#33818),.UNSPECIFIED.,.F.,.F.,(4,1,1,1,1,1,
1,4),(59.6902604182061,60.2221053542521,61.2092721506399,62.1964389470278,
63.1836057434156,64.1707725398034,65.1579393361912,65.9734457253856),
 .UNSPECIFIED.);
#401=B_SPLINE_CURVE_WITH_KNOTS('',3,(#33819,#33820,#33821,#33822,#33823,
#33824,#33825,#33826,#33827,#33828,#33829),.UNSPECIFIED.,.F.,.F.,(4,1,1,
1,1,1,1,1,4),(59.6902604182061,59.8637770723004,60.8509438686882,61.838110665076,
62.8252774614638,63.8124442578516,64.7996110542394,65.7867778506272,65.9734457253856),
 .UNSPECIFIED.);
#402=B_SPLINE_CURVE_WITH_KNOTS('',3,(#33834,#33835,#33836,#33837,#33838,
#33839,#33840,#33841,#33842,#33843),.UNSPECIFIED.,.F.,.F.,(4,1,1,1,1,1,
1,4),(53.4070751110265,54.2991045759252,55.2862713723131,56.2734381687009,
57.2606049650887,58.2477717614765,59.2349385578643,59.6902604182061),
 .UNSPECIFIED.);
#403=B_SPLINE_CURVE_WITH_KNOTS('',3,(#33844,#33845,#33846,#33847,#33848,
#33849,#33850,#33851,#33852,#33853),.UNSPECIFIED.,.F.,.F.,(4,1,1,1,1,1,
1,4),(53.4070751110265,53.9407762939735,54.9279430903613,55.9151098867491,
56.9022766831369,57.8894434795247,58.8766102759126,59.6902604182061),
 .UNSPECIFIED.);
#404=B_SPLINE_CURVE_WITH_KNOTS('',3,(#33858,#33859,#33860,#33861,#33862,
#33863,#33864,#33865,#33866,#33867,#33868),.UNSPECIFIED.,.F.,.F.,(4,1,1,
1,1,1,1,1,4),(47.1238898038469,47.3889370012105,48.3761037975984,49.3632705939862,
50.350437390374,51.3376041867618,52.3247709831496,53.3119377795374,53.4070751110265),
 .UNSPECIFIED.);
#405=B_SPLINE_CURVE_WITH_KNOTS('',3,(#33869,#33870,#33871,#33872,#33873,
#33874,#33875,#33876,#33877,#33878),.UNSPECIFIED.,.F.,.F.,(4,1,1,1,1,1,
1,4),(47.1238898038469,48.0177755156466,49.0049423120344,49.9921091084222,
50.97927590481,51.9664427011978,52.9536094975857,53.4070751110265),
 .UNSPECIFIED.);
#406=B_SPLINE_CURVE_WITH_KNOTS('',3,(#33883,#33884,#33885,#33886,#33887,
#33888,#33889,#33890,#33891,#33892),.UNSPECIFIED.,.F.,.F.,(4,1,1,1,1,1,
1,4),(40.8407044966673,41.4659362228837,42.4531030192715,43.4402698156593,
44.4274366120471,45.4146034084349,46.4017702048227,47.1238898038469),
 .UNSPECIFIED.);
#407=B_SPLINE_CURVE_WITH_KNOTS('',3,(#33893,#33894,#33895,#33896,#33897,
#33898,#33899,#33900,#33901,#33902,#33903),.UNSPECIFIED.,.F.,.F.,(4,1,1,
1,1,1,1,1,4),(40.8407044966673,41.1076079409319,42.0947747373197,43.0819415337075,
44.0691083300953,45.0562751264832,46.043441922871,47.0306087192588,47.1238898038469),
 .UNSPECIFIED.);
#408=B_SPLINE_CURVE_WITH_KNOTS('',3,(#33908,#33909,#33910,#33911,#33912,
#33913,#33914,#33915,#33916,#33917),.UNSPECIFIED.,.F.,.F.,(4,1,1,1,1,1,
1,4),(34.5575191894877,35.5429354445568,36.5301022409446,37.5172690373324,
38.5044358337202,39.491602630108,40.4787694264959,40.8407044966673),
 .UNSPECIFIED.);
#409=B_SPLINE_CURVE_WITH_KNOTS('',3,(#33918,#33919,#33920,#33921,#33922,
#33923,#33924,#33925,#33926,#33927),.UNSPECIFIED.,.F.,.F.,(4,1,1,1,1,1,
1,4),(34.5575191894877,35.184607162605,36.1717739589928,37.1589407553806,
38.1461075517685,39.1332743481563,40.1204411445441,40.8407044966673),
 .UNSPECIFIED.);
#410=B_SPLINE_CURVE_WITH_KNOTS('',3,(#33932,#33933,#33934,#33935,#33936,
#33937,#33938,#33939,#33940,#33941,#33942),.UNSPECIFIED.,.F.,.F.,(4,1,1,
1,1,1,1,1,4),(28.2743338823081,28.6327678698421,29.6199346662299,30.6071014626177,
31.5942682590055,32.5814350553933,33.5686018517812,34.555768648169,34.5575191894877),
 .UNSPECIFIED.);
#411=B_SPLINE_CURVE_WITH_KNOTS('',3,(#33943,#33944,#33945,#33946,#33947,
#33948,#33949,#33950,#33951,#33952,#33953),.UNSPECIFIED.,.F.,.F.,(4,1,1,
1,1,1,1,1,4),(28.2743338823081,28.2744395878903,29.2616063842781,30.2487731806659,
31.2359399770538,32.2231067734416,33.2102735698294,34.1974403662172,34.5575191894877),
 .UNSPECIFIED.);
#412=B_SPLINE_CURVE_WITH_KNOTS('',3,(#33958,#33959,#33960,#33961,#33962,
#33963,#33964,#33965,#33966,#33967),.UNSPECIFIED.,.F.,.F.,(4,1,1,1,1,1,
1,4),(21.9911485751285,22.7097670915152,23.696933887903,24.6841006842908,
25.6712674806786,26.6584342770665,27.6456010734543,28.2743338823081),
 .UNSPECIFIED.);
#413=B_SPLINE_CURVE_WITH_KNOTS('',3,(#33968,#33969,#33970,#33971,#33972,
#33973,#33974,#33975,#33976,#33977),.UNSPECIFIED.,.F.,.F.,(4,1,1,1,1,1,
1,4),(21.9911485751285,22.3514388095634,23.3386056059513,24.3257724023391,
25.3129391987269,26.3001059951147,27.2872727915025,28.2743338823081),
 .UNSPECIFIED.);
#414=B_SPLINE_CURVE_WITH_KNOTS('',3,(#33982,#33983,#33984,#33985,#33986,
#33987,#33988,#33989,#33990,#33991,#33992),.UNSPECIFIED.,.F.,.F.,(4,1,1,
1,1,1,1,1,4),(15.7079632679489,15.7995995168005,16.7867663131883,17.7739331095761,
18.7610999059639,19.7482667023518,20.7354334987396,21.7226002951274,21.9911485751285),
 .UNSPECIFIED.);
#415=B_SPLINE_CURVE_WITH_KNOTS('',3,(#33993,#33994,#33995,#33996,#33997,
#33998,#33999,#34000,#34001,#34002),.UNSPECIFIED.,.F.,.F.,(4,1,1,1,1,1,
1,4),(15.7079632679489,16.4284380312366,17.4156048276244,18.4027716240122,
19.3899384204,20.3771052167878,21.3642720131756,21.9911485751285),
 .UNSPECIFIED.);
#416=B_SPLINE_CURVE_WITH_KNOTS('',3,(#34296,#34297,#34298,#34299,#34300,
#34301,#34302,#34303,#34304,#34305,#34306,#34307,#34308,#34309,#34310,#34311,
#34312,#34313,#34314,#34315,#34316,#34317,#34318,#34319,#34320,#34321,#34322,
#34323,#34324,#34325,#34326,#34327,#34328,#34329,#34330,#34331,#34332,#34333,
#34334,#34335,#34336,#34337,#34338,#34339,#34340,#34341,#34342,#34343,#34344,
#34345,#34346,#34347,#34348,#34349,#34350,#34351,#34352,#34353,#34354,#34355,
#34356),.UNSPECIFIED.,.F.,.F.,(4,3,3,3,3,3,3,3,3,3,3,3,3,3,3,3,3,3,3,3,
4),(-0.780432929098612,-0.738338012777856,-0.683834258573259,-0.663838565476387,
-0.598169338795401,-0.577510604236597,-0.562119826273733,-0.497408932506566,
-0.451782302166264,-0.430327346583771,-0.415002532446257,-0.359442543267042,
-0.314512225358661,-0.29120578257896,-0.270249996878916,-0.207616527572625,
-0.155712395679469,-0.140396343062156,-0.123829552848863,-0.0619147764244314,
0.),.UNSPECIFIED.);
#417=B_SPLINE_CURVE_WITH_KNOTS('',3,(#34357,#34358,#34359,#34360,#34361,
#34362,#34363,#34364,#34365,#34366,#34367,#34368,#34369,#34370,#34371,#34372),
 .UNSPECIFIED.,.F.,.F.,(4,3,3,3,3,4),(62.7383605760433,63.1786749688201,
64.1658417652079,65.1530085615957,66.1401753579835,67.0206432765822),
 .UNSPECIFIED.);
#418=B_SPLINE_CURVE_WITH_KNOTS('',3,(#34374,#34375,#34376,#34377,#34378,
#34379,#34380,#34381,#34382,#34383,#34384,#34385,#34386,#34387,#34388,#34389,
#34390,#34391,#34392,#34393,#34394,#34395,#34396,#34397,#34398,#34399,#34400,
#34401,#34402,#34403,#34404,#34405,#34406,#34407,#34408,#34409,#34410,#34411,
#34412,#34413,#34414,#34415,#34416,#34417,#34418,#34419,#34420,#34421,#34422,
#34423,#34424,#34425,#34426,#34427,#34428,#34429,#34430,#34431,#34432,#34433,
#34434,#34435,#34436,#34437),.UNSPECIFIED.,.F.,.F.,(4,3,3,3,3,3,3,3,3,3,
3,3,3,3,3,3,3,3,3,3,3,4),(-0.782320427274649,-0.744412510134687,-0.688529792301629,
-0.669642910660232,-0.618424444943536,-0.597739729117171,-0.580869545572353,
-0.517475334412603,-0.472408188284826,-0.451438075940233,-0.43660958913821,
-0.382241417220766,-0.33446124006817,-0.310889038365519,-0.29130300268306,
-0.227103495746363,-0.170327621809772,-0.152876921934579,-0.137524083313296,
-0.0687620416566481,-0.00415757966036404,0.),.UNSPECIFIED.);
#419=B_SPLINE_CURVE_WITH_KNOTS('',3,(#34438,#34439,#34440,#34441,#34442,
#34443,#34444,#34445),.UNSPECIFIED.,.F.,.F.,(4,1,1,1,1,4),(11.5993029270866,
12.4797708456853,13.4669376420731,14.4541044384609,15.4412712348487,15.7079632679489),
 .UNSPECIFIED.);
#420=B_SPLINE_CURVE_WITH_KNOTS('',3,(#34448,#34449,#34450,#34451,#34452,
#34453,#34454,#34455,#34456,#34457,#34458,#34459,#34460,#34461,#34462,#34463,
#34464,#34465,#34466,#34467,#34468,#34469,#34470,#34471,#34472,#34473,#34474,
#34475,#34476,#34477,#34478,#34479,#34480,#34481,#34482,#34483,#34484,#34485,
#34486,#34487,#34488,#34489,#34490,#34491,#34492,#34493,#34494,#34495,#34496,
#34497,#34498,#34499,#34500,#34501,#34502,#34503,#34504,#34505,#34506,#34507,
#34508),.UNSPECIFIED.,.F.,.F.,(4,3,3,3,3,3,3,3,3,3,3,3,3,3,3,3,3,3,3,3,
4),(-0.780432929098611,-0.738338012777859,-0.683834237462397,-0.663838555047122,
-0.598169328522835,-0.577510488075,-0.562119617951329,-0.497408718040529,
-0.45178193717698,-0.430324802159164,-0.415000406365485,-0.359442543267047,
-0.314512225358666,-0.29120578372101,-0.27024999961834,-0.207616508984274,
-0.155712381738205,-0.140396296964378,-0.123829546509967,-0.0619147732549836,
0.),.UNSPECIFIED.);
#421=B_SPLINE_CURVE_WITH_KNOTS('',3,(#34511,#34512,#34513,#34514,#34515,
#34516),.UNSPECIFIED.,.F.,.F.,(4,1,1,4),(12.8380991276371,13.8252659240249,
14.8124327204127,15.7079632679489),.UNSPECIFIED.);
#422=B_SPLINE_CURVE_WITH_KNOTS('',3,(#34810,#34811,#34812,#34813,#34814,
#34815,#34816,#34817,#34818,#34819,#34820,#34821,#34822,#34823,#34824,#34825,
#34826,#34827,#34828,#34829,#34830,#34831,#34832,#34833,#34834,#34835,#34836,
#34837,#34838,#34839,#34840,#34841,#34842,#34843,#34844,#34845,#34846,#34847,
#34848,#34849,#34850,#34851,#34852,#34853,#34854,#34855,#34856,#34857,#34858,
#34859,#34860,#34861,#34862,#34863,#34864,#34865,#34866,#34867,#34868,#34869,
#34870,#34871,#34872,#34873),.UNSPECIFIED.,.F.,.F.,(4,3,3,3,3,3,3,3,3,3,
3,3,3,3,3,3,3,3,3,3,3,4),(-0.782320427274647,-0.744412510134681,-0.688529784827506,
-0.669642900569953,-0.618424486060736,-0.597739627606828,-0.580869476506375,
-0.5174752643267,-0.472408127669552,-0.451437419639239,-0.436608276654843,
-0.38224141722077,-0.334461240068174,-0.310889049141467,-0.291303007297222,
-0.227103471436237,-0.170327603577178,-0.152876814667526,-0.137524066743929,
-0.0687620333719644,-0.00415763970634024,0.),.UNSPECIFIED.);
#423=B_SPLINE_CURVE_WITH_KNOTS('',3,(#34874,#34875,#34876,#34877,#34878,
#34879,#34880,#34881,#34882,#34883,#34884,#34885,#34886),.UNSPECIFIED.,
 .F.,.F.,(4,3,3,3,4),(-69.101675747147,-68.1145089507592,-67.1273421543714,
-66.1401753579836,-65.7017172121077),.UNSPECIFIED.);
#424=B_SPLINE_CURVE_WITH_KNOTS('',3,(#36162,#36163,#36164,#36165,#36166,
#36167,#36168,#36169,#36170,#36171,#36172,#36173,#36174),.UNSPECIFIED.,
 .F.,.F.,(4,3,3,3,4),(-5.47484251641785,-4.99048533890455,-3.99238827112364,
-2.99429120334273,-2.06514013327811),.UNSPECIFIED.);
#425=B_SPLINE_CURVE_WITH_KNOTS('',3,(#36182,#36183,#36184,#36185,#36186,
#36187,#36188,#36189,#36190,#36191),.UNSPECIFIED.,.F.,.F.,(4,3,3,4),(0.,
0.998097067780899,1.99619413556182,2.49649180560904),.UNSPECIFIED.);
#426=B_SPLINE_CURVE_WITH_KNOTS('',3,(#36196,#36197,#36198,#36199,#36200,
#36201,#36202,#36203,#36204,#36205,#36206,#36207,#36208,#36209,#36210,#36211,
#36212,#36213,#36214,#36215,#36216,#36217),.UNSPECIFIED.,.F.,.F.,(4,3,3,
3,3,3,3,4),(-11.7580278235974,-10.97906774559,-9.9809706778091,-8.98287361002818,
-7.98477654224727,-6.98667947446637,-5.98858240668546,-5.47484251641785),
 .UNSPECIFIED.);
#427=B_SPLINE_CURVE_WITH_KNOTS('',3,(#36218,#36219,#36220,#36221,#36222,
#36223,#36224,#36225,#36226,#36227,#36228,#36229,#36230,#36231,#36232,#36233,
#36234,#36235,#36236,#36237,#36238,#36239),.UNSPECIFIED.,.F.,.F.,(4,3,3,
3,3,3,3,4),(2.49649180560904,2.99429120334273,3.99238827112364,4.99048533890454,
5.98858240668546,6.98667947446636,7.98477654224727,8.77967711278862),
 .UNSPECIFIED.);
#428=B_SPLINE_CURVE_WITH_KNOTS('',3,(#36244,#36245,#36246,#36247,#36248,
#36249,#36250,#36251,#36252,#36253,#36254,#36255,#36256,#36257,#36258,#36259,
#36260,#36261,#36262,#36263,#36264,#36265,#36266,#36267,#36268),
 .UNSPECIFIED.,.F.,.F.,(4,3,3,3,3,3,3,3,4),(-18.041213130777,-17.9657472200564,
-16.9676501522755,-15.9695530844945,-14.9714560167136,-13.9733589489327,
-12.9752618811518,-11.9771648133709,-11.7580278235974),.UNSPECIFIED.);
#429=B_SPLINE_CURVE_WITH_KNOTS('',3,(#36269,#36270,#36271,#36272,#36273,
#36274,#36275,#36276,#36277,#36278,#36279,#36280,#36281,#36282,#36283,#36284,
#36285,#36286,#36287,#36288,#36289,#36290,#36291,#36292,#36293),
 .UNSPECIFIED.,.F.,.F.,(4,3,3,3,3,3,3,3,4),(8.77967711278862,8.98287361002818,
9.98097067780909,10.97906774559,11.9771648133709,12.9752618811518,13.9733589489327,
14.9714560167136,15.0628624199682),.UNSPECIFIED.);
#430=B_SPLINE_CURVE_WITH_KNOTS('',3,(#36298,#36299,#36300,#36301,#36302,
#36303,#36304,#36305,#36306,#36307,#36308,#36309,#36310,#36311,#36312,#36313,
#36314,#36315,#36316,#36317,#36318,#36319),.UNSPECIFIED.,.F.,.F.,(4,3,3,
3,3,3,3,4),(-24.3243984379566,-23.9543296267418,-22.9562325589609,-21.95813549118,
-20.9600384233991,-19.9619413556182,-18.9638442878373,-18.041213130777),
 .UNSPECIFIED.);
#431=B_SPLINE_CURVE_WITH_KNOTS('',3,(#36320,#36321,#36322,#36323,#36324,
#36325,#36326,#36327,#36328,#36329,#36330,#36331,#36332,#36333,#36334,#36335,
#36336,#36337,#36338,#36339,#36340,#36341),.UNSPECIFIED.,.F.,.F.,(4,3,3,
3,3,3,3,4),(15.0628624199682,15.9695530844945,16.9676501522755,17.9657472200564,
18.9638442878373,19.9619413556182,20.9600384233991,21.3460477271478),
 .UNSPECIFIED.);
#432=B_SPLINE_CURVE_WITH_KNOTS('',3,(#36346,#36347,#36348,#36349,#36350,
#36351,#36352,#36353,#36354,#36355,#36356,#36357,#36358,#36359,#36360,#36361,
#36362,#36363,#36364,#36365,#36366,#36367),.UNSPECIFIED.,.F.,.F.,(4,3,3,
3,3,3,3,4),(-30.6075837451362,-29.9429120334273,-28.9448149656464,-27.9467178978655,
-26.9486208300846,-25.9505237623036,-24.9524266945227,-24.3243984379566),
 .UNSPECIFIED.);
#433=B_SPLINE_CURVE_WITH_KNOTS('',3,(#36368,#36369,#36370,#36371,#36372,
#36373,#36374,#36375,#36376,#36377,#36378,#36379,#36380,#36381,#36382,#36383,
#36384,#36385,#36386,#36387,#36388,#36389),.UNSPECIFIED.,.F.,.F.,(4,3,3,
3,3,3,3,4),(21.3460477271478,21.95813549118,22.9562325589609,23.9543296267418,
24.9524266945227,25.9505237623036,26.9486208300845,27.6292330343274),
 .UNSPECIFIED.);
#434=B_SPLINE_CURVE_WITH_KNOTS('',3,(#36394,#36395,#36396,#36397,#36398,
#36399,#36400,#36401,#36402,#36403,#36404,#36405,#36406,#36407,#36408,#36409,
#36410,#36411,#36412,#36413,#36414,#36415),.UNSPECIFIED.,.F.,.F.,(4,3,3,
3,3,3,3,4),(-36.8907690523158,-35.9314944401127,-34.9333973723318,-33.9353003045509,
-32.93720323677,-31.9391061689891,-30.9410091012082,-30.6075837451362),
 .UNSPECIFIED.);
#435=B_SPLINE_CURVE_WITH_KNOTS('',3,(#36416,#36417,#36418,#36419,#36420,
#36421,#36422,#36423,#36424,#36425,#36426,#36427,#36428,#36429,#36430,#36431,
#36432,#36433,#36434,#36435,#36436,#36437),.UNSPECIFIED.,.F.,.F.,(4,3,3,
3,3,3,3,4),(27.6292330343274,27.9467178978654,28.9448149656464,29.9429120334273,
30.9410091012082,31.9391061689891,32.93720323677,33.912418341507),
 .UNSPECIFIED.);
#436=B_SPLINE_CURVE_WITH_KNOTS('',3,(#36442,#36443,#36444,#36445,#36446,
#36447,#36448,#36449,#36450,#36451,#36452,#36453,#36454,#36455,#36456,#36457,
#36458,#36459,#36460,#36461,#36462,#36463,#36464,#36465,#36466),
 .UNSPECIFIED.,.F.,.F.,(4,3,3,3,3,3,3,3,4),(-43.1739543594954,-42.9181739145791,
-41.9200768467982,-40.9219797790173,-39.9238827112364,-38.9257856434555,
-37.9276885756746,-36.9295915078936,-36.8907690523158),.UNSPECIFIED.);
#437=B_SPLINE_CURVE_WITH_KNOTS('',3,(#36467,#36468,#36469,#36470,#36471,
#36472,#36473,#36474,#36475,#36476,#36477,#36478,#36479,#36480,#36481,#36482,
#36483,#36484,#36485,#36486,#36487,#36488,#36489,#36490,#36491),
 .UNSPECIFIED.,.F.,.F.,(4,3,3,3,3,3,3,3,4),(33.912418341507,33.9353003045509,
34.9333973723318,35.9314944401127,36.9295915078936,37.9276885756745,38.9257856434555,
39.9238827112364,40.1956036486866),.UNSPECIFIED.);
#438=B_SPLINE_CURVE_WITH_KNOTS('',3,(#36496,#36497,#36498,#36499,#36500,
#36501,#36502,#36503,#36504,#36505,#36506,#36507,#36508,#36509,#36510,#36511,
#36512,#36513,#36514,#36515,#36516,#36517),.UNSPECIFIED.,.F.,.F.,(4,3,3,
3,3,3,3,4),(-49.457139666675,-48.9067563212645,-47.9086592534836,-46.9105621857027,
-45.9124651179218,-44.9143680501409,-43.91627098236,-43.1739543594954),
 .UNSPECIFIED.);
#439=B_SPLINE_CURVE_WITH_KNOTS('',3,(#36518,#36519,#36520,#36521,#36522,
#36523,#36524,#36525,#36526,#36527,#36528,#36529,#36530,#36531,#36532,#36533,
#36534,#36535,#36536,#36537,#36538,#36539),.UNSPECIFIED.,.F.,.F.,(4,3,3,
3,3,3,3,4),(40.1956036486866,40.9219797790173,41.9200768467982,42.9181739145791,
43.91627098236,44.9143680501409,45.9124651179218,46.4787889558661),
 .UNSPECIFIED.);
#440=B_SPLINE_CURVE_WITH_KNOTS('',3,(#36544,#36545,#36546,#36547,#36548,
#36549,#36550,#36551,#36552,#36553,#36554,#36555,#36556,#36557,#36558,#36559,
#36560,#36561,#36562,#36563,#36564,#36565),.UNSPECIFIED.,.F.,.F.,(4,3,3,
3,3,3,3,4),(-55.7403249738546,-54.89533872795,-53.8972416601691,-52.8991445923882,
-51.9010475246073,-50.9029504568264,-49.9048533890454,-49.457139666675),
 .UNSPECIFIED.);
#441=B_SPLINE_CURVE_WITH_KNOTS('',3,(#36566,#36567,#36568,#36569,#36570,
#36571,#36572,#36573,#36574,#36575,#36576,#36577,#36578,#36579,#36580,#36581,
#36582,#36583,#36584,#36585,#36586,#36587),.UNSPECIFIED.,.F.,.F.,(4,3,3,
3,3,3,3,4),(46.4787889558661,46.9105621857027,47.9086592534836,48.9067563212645,
49.9048533890454,50.9029504568264,51.9010475246073,52.7619742630458),
 .UNSPECIFIED.);
#442=B_SPLINE_CURVE_WITH_KNOTS('',3,(#36592,#36593,#36594,#36595,#36596,
#36597,#36598,#36599,#36600,#36601,#36602,#36603,#36604,#36605,#36606,#36607,
#36608,#36609,#36610,#36611,#36612,#36613,#36614,#36615,#36616),
 .UNSPECIFIED.,.F.,.F.,(4,3,3,3,3,3,3,3,4),(-62.0235102810341,-61.8820182024164,
-60.8839211346355,-59.8858240668546,-58.8877269990736,-57.8896299312927,
-56.8915328635118,-55.8934357957309,-55.7403249738546),.UNSPECIFIED.);
#443=B_SPLINE_CURVE_WITH_KNOTS('',3,(#36617,#36618,#36619,#36620,#36621,
#36622,#36623,#36624,#36625,#36626,#36627,#36628,#36629,#36630,#36631,#36632,
#36633,#36634,#36635,#36636,#36637,#36638,#36639,#36640,#36641),
 .UNSPECIFIED.,.F.,.F.,(4,3,3,3,3,3,3,3,4),(52.7619742630458,52.8991445923882,
53.8972416601691,54.89533872795,55.8934357957309,56.8915328635118,57.8896299312927,
58.8877269990736,59.0451595702253),.UNSPECIFIED.);
#444=B_SPLINE_CURVE_WITH_KNOTS('',3,(#36646,#36647,#36648,#36649,#36650,
#36651,#36652,#36653,#36654,#36655,#36656,#36657,#36658,#36659,#36660,#36661,
#36662,#36663,#36664,#36665,#36666,#36667),.UNSPECIFIED.,.F.,.F.,(4,3,3,
3,3,3,3,4),(-68.3066955882137,-67.8706006091018,-66.8725035413209,-65.87440647354,
-64.8763094057591,-63.8782123379782,-62.8801152701973,-62.0235102810341),
 .UNSPECIFIED.);
#445=B_SPLINE_CURVE_WITH_KNOTS('',3,(#36668,#36669,#36670,#36671,#36672,
#36673,#36674,#36675,#36676,#36677,#36678,#36679,#36680,#36681,#36682,#36683,
#36684,#36685,#36686,#36687,#36688,#36689),.UNSPECIFIED.,.F.,.F.,(4,3,3,
3,3,3,3,4),(59.0451595702253,59.8858240668545,60.8839211346355,61.8820182024164,
62.8801152701973,63.8782123379782,64.8763094057591,65.3283448774049),
 .UNSPECIFIED.);
#446=B_SPLINE_CURVE_WITH_KNOTS('',3,(#36694,#36695,#36696,#36697,#36698,
#36699,#36700,#36701,#36702,#36703,#36704,#36705,#36706,#36707,#36708,#36709,
#36710,#36711,#36712,#36713,#36714,#36715),.UNSPECIFIED.,.F.,.F.,(4,3,3,
3,3,3,3,4),(-74.5898808953933,-73.8591830157873,-72.8610859480063,-71.8629888802254,
-70.8648918124445,-69.8667947446636,-68.8686976768827,-68.3066955882137),
 .UNSPECIFIED.);
#447=B_SPLINE_CURVE_WITH_KNOTS('',3,(#36716,#36717,#36718,#36719,#36720,
#36721,#36722,#36723,#36724,#36725,#36726,#36727,#36728,#36729,#36730,#36731,
#36732,#36733,#36734,#36735,#36736,#36737),.UNSPECIFIED.,.F.,.F.,(4,3,3,
3,3,3,3,4),(65.3283448774049,65.87440647354,66.8725035413209,67.8706006091018,
68.8686976768827,69.8667947446636,70.8648918124445,71.6115301845845),
 .UNSPECIFIED.);
#448=B_SPLINE_CURVE_WITH_KNOTS('',3,(#36742,#36743,#36744,#36745,#36746,
#36747,#36748,#36749,#36750,#36751,#36752,#36753,#36754,#36755,#36756,#36757,
#36758,#36759,#36760,#36761,#36762,#36763,#36764,#36765,#36766),
 .UNSPECIFIED.,.F.,.F.,(4,3,3,3,3,3,3,3,4),(-80.8730662025729,-80.8458624902537,
-79.8477654224727,-78.8496683546918,-77.8515712869109,-76.85347421913,-75.8553771513491,
-74.8572800835682,-74.5898808953933),.UNSPECIFIED.);
#449=B_SPLINE_CURVE_WITH_KNOTS('',3,(#36767,#36768,#36769,#36770,#36771,
#36772,#36773,#36774,#36775,#36776,#36777,#36778,#36779,#36780,#36781,#36782,
#36783,#36784,#36785,#36786,#36787,#36788,#36789,#36790,#36791),
 .UNSPECIFIED.,.F.,.F.,(4,3,3,3,3,3,3,3,4),(71.6115301845845,71.8629888802254,
72.8610859480063,73.8591830157873,74.8572800835682,75.8553771513491,76.85347421913,
77.8515712869109,77.8947154917641),.UNSPECIFIED.);
#450=B_SPLINE_CURVE_WITH_KNOTS('',3,(#36796,#36797,#36798,#36799,#36800,
#36801,#36802,#36803,#36804,#36805,#36806,#36807,#36808,#36809,#36810,#36811,
#36812,#36813,#36814,#36815,#36816,#36817),.UNSPECIFIED.,.F.,.F.,(4,3,3,
3,3,3,3,4),(-87.1562515097525,-86.8344448969391,-85.8363478291582,-84.8382507613773,
-83.8401536935964,-82.8420566258155,-81.8439595580345,-80.8730662025729),
 .UNSPECIFIED.);
#451=B_SPLINE_CURVE_WITH_KNOTS('',3,(#36818,#36819,#36820,#36821,#36822,
#36823,#36824,#36825,#36826,#36827,#36828,#36829,#36830,#36831,#36832,#36833,
#36834,#36835,#36836,#36837,#36838,#36839),.UNSPECIFIED.,.F.,.F.,(4,3,3,
3,3,3,3,4),(77.8947154917641,78.8496683546918,79.8477654224727,80.8458624902536,
81.8439595580346,82.8420566258154,83.8401536935964,84.1779007989437),
 .UNSPECIFIED.);
#452=B_SPLINE_CURVE_WITH_KNOTS('',3,(#36845,#36846,#36847,#36848,#36849,
#36850),.UNSPECIFIED.,.F.,.F.,(4,1,1,4),(103.672557568463,104.348848023431,
105.346945091212,106.276096161276),.UNSPECIFIED.);
#453=B_SPLINE_CURVE_WITH_KNOTS('',3,(#36853,#36854,#36855,#36856,#36857),
 .UNSPECIFIED.,.F.,.F.,(4,1,4),(103.672557568463,104.038304630403,105.036401698183),
 .UNSPECIFIED.);
#454=B_SPLINE_CURVE_WITH_KNOTS('',3,(#36862,#36863,#36864,#36865,#36866,
#36867,#36868,#36869,#36870,#36871),.UNSPECIFIED.,.F.,.F.,(4,1,1,1,1,1,
1,4),(97.3893722612836,98.3602656167452,99.3583626845261,100.356459752307,
101.354556820088,102.352653887869,103.35075095565,103.672557568463),
 .UNSPECIFIED.);
#455=B_SPLINE_CURVE_WITH_KNOTS('',3,(#36872,#36873,#36874,#36875,#36876,
#36877,#36878,#36879,#36880,#36881),.UNSPECIFIED.,.F.,.F.,(4,1,1,1,1,1,
1,4),(97.3893722612836,98.0497222237171,99.047819291498,100.045916359279,
101.04401342706,102.042110494841,103.040207562622,103.672557568463),
 .UNSPECIFIED.);
#456=B_SPLINE_CURVE_WITH_KNOTS('',3,(#36886,#36887,#36888,#36889,#36890,
#36891,#36892,#36893,#36894,#36895,#36896),.UNSPECIFIED.,.F.,.F.,(4,1,1,
1,1,1,1,1,4),(91.106186954104,91.3735861422788,92.3716832100597,93.3697802778406,
94.3678773456216,95.3659744134025,96.3640714811834,97.3621685489643,97.3893722612836),
 .UNSPECIFIED.);
#457=B_SPLINE_CURVE_WITH_KNOTS('',3,(#36897,#36898,#36899,#36900,#36901,
#36902,#36903,#36904,#36905,#36906),.UNSPECIFIED.,.F.,.F.,(4,1,1,1,1,1,
1,4),(91.106186954104,92.0611398170316,93.0592368848125,94.0573339525934,
95.0554310203743,96.0535280881552,97.0516251559362,97.3893722612836),
 .UNSPECIFIED.);
#458=B_SPLINE_CURVE_WITH_KNOTS('',3,(#36911,#36912,#36913,#36914,#36915,
#36916,#36917,#36918,#36919,#36920),.UNSPECIFIED.,.F.,.F.,(4,1,1,1,1,1,
1,4),(84.8230016469244,85.3850037355934,86.3831008033743,87.3811978711552,
88.3792949389361,89.377392006717,90.3754890744979,91.106186954104),
 .UNSPECIFIED.);
#459=B_SPLINE_CURVE_WITH_KNOTS('',3,(#36921,#36922,#36923,#36924,#36925,
#36926,#36927,#36928,#36929,#36930,#36931),.UNSPECIFIED.,.F.,.F.,(4,1,1,
1,1,1,1,1,4),(84.8230016469244,85.0744603425652,86.0725574103461,87.0706544781271,
88.068751545908,89.0668486136889,90.0649456814698,91.0630427492507,91.106186954104),
 .UNSPECIFIED.);
#460=B_SPLINE_CURVE_WITH_KNOTS('',3,(#36936,#36937,#36938,#36939,#36940,
#36941,#36942,#36943,#36944,#36945),.UNSPECIFIED.,.F.,.F.,(4,1,1,1,1,1,
1,4),(78.5398163397448,79.3964213289079,80.3945183966888,81.3926154644697,
82.3907125322506,83.3888096000315,84.3869066678125,84.8230016469244),
 .UNSPECIFIED.);
#461=B_SPLINE_CURVE_WITH_KNOTS('',3,(#36946,#36947,#36948,#36949,#36950,
#36951,#36952,#36953,#36954,#36955),.UNSPECIFIED.,.F.,.F.,(4,1,1,1,1,1,
1,4),(78.5398163397448,79.0858779358798,80.0839750036607,81.0820720714416,
82.0801691392225,83.0782662070034,84.0763632747843,84.8230016469244),
 .UNSPECIFIED.);
#462=B_SPLINE_CURVE_WITH_KNOTS('',3,(#36960,#36961,#36962,#36963,#36964,
#36965,#36966,#36967,#36968,#36969,#36970),.UNSPECIFIED.,.F.,.F.,(4,1,1,
1,1,1,1,1,4),(72.2566310325652,72.4097418544415,73.4078389222225,74.4059359900034,
75.4040330577843,76.4021301255652,77.4002271933461,78.398324261127,78.5398163397448),
 .UNSPECIFIED.);
#463=B_SPLINE_CURVE_WITH_KNOTS('',3,(#36971,#36972,#36973,#36974,#36975,
#36976,#36977,#36978,#36979,#36980),.UNSPECIFIED.,.F.,.F.,(4,1,1,1,1,1,
1,4),(72.2566310325652,73.0972955291943,74.0953925969752,75.0934896647561,
76.0915867325371,77.089683800318,78.0877808680989,78.5398163397448),
 .UNSPECIFIED.);
#464=B_SPLINE_CURVE_WITH_KNOTS('',3,(#36985,#36986,#36987,#36988,#36989,
#36990,#36991,#36992,#36993,#36994),.UNSPECIFIED.,.F.,.F.,(4,1,1,1,1,1,
1,4),(65.9734457253856,66.4211594477561,67.419256515537,68.4173535833179,
69.4154506510988,70.4135477188797,71.4116447866606,72.2566310325652),
 .UNSPECIFIED.);
#465=B_SPLINE_CURVE_WITH_KNOTS('',3,(#36995,#36996,#36997,#36998,#36999,
#37000,#37001,#37002,#37003,#37004,#37005),.UNSPECIFIED.,.F.,.F.,(4,1,1,
1,1,1,1,1,4),(65.9734457253856,66.110616054728,67.1087131225089,68.1068101902898,
69.1049072580707,70.1030043258516,71.1011013936325,72.0991984614134,72.2566310325652),
 .UNSPECIFIED.);
#466=B_SPLINE_CURVE_WITH_KNOTS('',3,(#37010,#37011,#37012,#37013,#37014,
#37015,#37016,#37017,#37018,#37019),.UNSPECIFIED.,.F.,.F.,(4,1,1,1,1,1,
1,4),(59.690260418206,60.4325770410706,61.4306741088515,62.4287711766325,
63.4268682444134,64.4249653121943,65.4230623799752,65.9734457253856),
 .UNSPECIFIED.);
#467=B_SPLINE_CURVE_WITH_KNOTS('',3,(#37020,#37021,#37022,#37023,#37024,
#37025,#37026,#37027,#37028,#37029),.UNSPECIFIED.,.F.,.F.,(4,1,1,1,1,1,
1,4),(59.690260418206,60.1220336480425,61.1201307158234,62.1182277836043,
63.1163248513852,64.1144219191661,65.1125189869471,65.9734457253856),
 .UNSPECIFIED.);
#468=B_SPLINE_CURVE_WITH_KNOTS('',3,(#37034,#37035,#37036,#37037,#37038,
#37039,#37040,#37041,#37042,#37043,#37044),.UNSPECIFIED.,.F.,.F.,(4,1,1,
1,1,1,1,1,4),(53.4070751110265,53.4458975666043,54.4439946343852,55.4420917021661,
56.440188769947,57.4382858377279,58.4363829055088,59.4344799732897,59.690260418206),
 .UNSPECIFIED.);
#469=B_SPLINE_CURVE_WITH_KNOTS('',3,(#37045,#37046,#37047,#37048,#37049,
#37050,#37051,#37052,#37053,#37054),.UNSPECIFIED.,.F.,.F.,(4,1,1,1,1,1,
1,4),(53.4070751110264,54.1334512413571,55.131548309138,56.1296453769189,
57.1277424446998,58.1258395124807,59.1239365802616,59.690260418206),
 .UNSPECIFIED.);
#470=B_SPLINE_CURVE_WITH_KNOTS('',3,(#37059,#37060,#37061,#37062,#37063,
#37064,#37065,#37066,#37067,#37068),.UNSPECIFIED.,.F.,.F.,(4,1,1,1,1,1,
1,4),(47.1238898038469,47.4573151599188,48.4554122276997,49.4535092954806,
50.4516063632615,51.4497034310425,52.4478004988234,53.4070751110265),
 .UNSPECIFIED.);
#471=B_SPLINE_CURVE_WITH_KNOTS('',3,(#37069,#37070,#37071,#37072,#37073,
#37074,#37075,#37076,#37077,#37078,#37079),.UNSPECIFIED.,.F.,.F.,(4,1,1,
1,1,1,1,1,4),(47.1238898038468,47.1467717668907,48.1448688346716,49.1429659024525,
50.1410629702334,51.1391600380143,52.1372571057952,53.1353541735761,53.4070751110264),
 .UNSPECIFIED.);
#472=B_SPLINE_CURVE_WITH_KNOTS('',3,(#37084,#37085,#37086,#37087,#37088,
#37089,#37090,#37091,#37092,#37093),.UNSPECIFIED.,.F.,.F.,(4,1,1,1,1,1,
1,4),(40.8407044966673,41.4687327532334,42.4668298210143,43.4649268887952,
44.4630239565761,45.461121024357,46.4592180921379,47.1238898038469),
 .UNSPECIFIED.);
#473=B_SPLINE_CURVE_WITH_KNOTS('',3,(#37094,#37095,#37096,#37097,#37098,
#37099,#37100,#37101,#37102,#37103),.UNSPECIFIED.,.F.,.F.,(4,1,1,1,1,1,
1,4),(40.8407044966673,41.1581893602052,42.1562864279861,43.1543834957671,
44.152480563548,45.1505776313289,46.1486746991098,47.1238898038468),
 .UNSPECIFIED.);
#474=B_SPLINE_CURVE_WITH_KNOTS('',3,(#37108,#37109,#37110,#37111,#37112,
#37113,#37114,#37115,#37116,#37117),.UNSPECIFIED.,.F.,.F.,(4,1,1,1,1,1,
1,4),(34.5575191894877,35.4801503465479,36.4782474143288,37.4763444821097,
38.4744415498906,39.4725386176716,40.4706356854525,40.8407044966673),
 .UNSPECIFIED.);
#475=B_SPLINE_CURVE_WITH_KNOTS('',3,(#37118,#37119,#37120,#37121,#37122,
#37123,#37124,#37125,#37126,#37127),.UNSPECIFIED.,.F.,.F.,(4,1,1,1,1,1,
1,4),(34.5575191894876,35.1696069535198,36.1677040213007,37.1658010890816,
38.1638981568625,39.1619952246434,40.1600922924243,40.8407044966673),
 .UNSPECIFIED.);
#476=B_SPLINE_CURVE_WITH_KNOTS('',3,(#37132,#37133,#37134,#37135,#37136,
#37137,#37138,#37139,#37140,#37141,#37142),.UNSPECIFIED.,.F.,.F.,(4,1,1,
1,1,1,1,1,4),(28.2743338823081,28.4934708720816,29.4915679398625,30.4896650076434,
31.4877620754243,32.4858591432052,33.4839562109861,34.482053278767,34.5575191894877),
 .UNSPECIFIED.);
#477=B_SPLINE_CURVE_WITH_KNOTS('',3,(#37143,#37144,#37145,#37146,#37147,
#37148,#37149,#37150,#37151,#37152),.UNSPECIFIED.,.F.,.F.,(4,1,1,1,1,1,
1,4),(28.2743338823081,29.1810245468343,30.1791216146152,31.1772186823961,
32.1753157501771,33.173412817958,34.1715098857389,34.5575191894876),
 .UNSPECIFIED.);
#478=B_SPLINE_CURVE_WITH_KNOTS('',3,(#37157,#37158,#37159,#37160,#37161,
#37162,#37163,#37164,#37165,#37166),.UNSPECIFIED.,.F.,.F.,(4,1,1,1,1,1,
1,4),(21.9911485751285,22.5048884653961,23.502985533177,24.5010826009579,
25.4991796687388,26.4972767365197,27.4953738043006,28.2743338823081),
 .UNSPECIFIED.);
#479=B_SPLINE_CURVE_WITH_KNOTS('',3,(#37167,#37168,#37169,#37170,#37171,
#37172,#37173,#37174,#37175,#37176,#37177),.UNSPECIFIED.,.F.,.F.,(4,1,1,
1,1,1,1,1,4),(21.9911485751285,22.194345072368,23.1924421401489,24.1905392079298,
25.1886362757107,26.1867333434916,27.1848304112725,28.1829274790534,28.2743338823081),
 .UNSPECIFIED.);
#480=B_SPLINE_CURVE_WITH_KNOTS('',3,(#37184,#37185,#37186,#37187,#37188,
#37189,#37190,#37191,#37192),.UNSPECIFIED.,.F.,.F.,(4,1,1,1,1,1,4),(16.5163060587106,
17.5144031264916,18.5125001942725,19.5105972620534,20.5086943298343,21.5067913976152,
21.9911485751285),.UNSPECIFIED.);
#481=B_SPLINE_CURVE_WITH_KNOTS('',3,(#37193,#37194,#37195,#37196,#37197,
#37198,#37199,#37200,#37201,#37202),.UNSPECIFIED.,.F.,.F.,(4,1,1,1,1,1,
1,4),(15.7079632679489,16.2057626656825,17.2038597334634,18.2019568012443,
19.2000538690252,20.1981509368061,21.1962480045871,21.9911485751285),
 .UNSPECIFIED.);
#482=B_SPLINE_CURVE_WITH_KNOTS('',3,(#37584,#37585,#37586,#37587,#37588,
#37589,#37590,#37591,#37592,#37593,#37594,#37595,#37596,#37597,#37598,#37599,
#37600,#37601,#37602,#37603,#37604,#37605,#37606,#37607,#37608,#37609,#37610,
#37611,#37612,#37613,#37614,#37615,#37616,#37617,#37618,#37619,#37620,#37621,
#37622,#37623,#37624,#37625,#37626,#37627,#37628,#37629,#37630,#37631,#37632,
#37633,#37634,#37635),.UNSPECIFIED.,.F.,.F.,(4,3,3,3,3,3,3,3,3,3,3,3,3,
3,3,3,3,4),(-0.364629307890681,-0.351181914845152,-0.324753851954228,-0.31145962862552,
-0.274713453807112,-0.262559121200167,-0.225887319857606,-0.201681225023098,
-0.18621980244873,-0.166307755252122,-0.130572805038765,-0.119339783412349,
-0.0895048375592621,-0.072935651299665,-0.0625561387419937,-0.0518706549961582,
-0.019619443813511,0.),.UNSPECIFIED.);
#483=B_SPLINE_CURVE_WITH_KNOTS('',3,(#37636,#37637,#37638,#37639,#37640,
#37641,#37642,#37643,#37644,#37645,#37646,#37647,#37648,#37649,#37650,#37651,
#37652,#37653,#37654),.UNSPECIFIED.,.F.,.F.,(4,3,3,3,3,3,4),(84.1779007989437,
84.8382507613773,85.8363478291582,86.8344448969391,87.83254196472,88.8306390325009,
89.7597901025655),.UNSPECIFIED.);
#484=B_SPLINE_CURVE_WITH_KNOTS('',3,(#37656,#37657,#37658,#37659,#37660,
#37661,#37662,#37663,#37664,#37665,#37666,#37667,#37668,#37669,#37670,#37671,
#37672,#37673,#37674,#37675,#37676,#37677,#37678,#37679,#37680,#37681,#37682,
#37683,#37684,#37685,#37686,#37687,#37688,#37689,#37690,#37691,#37692,#37693,
#37694,#37695,#37696,#37697,#37698,#37699,#37700,#37701,#37702,#37703,#37704,
#37705,#37706,#37707),.UNSPECIFIED.,.F.,.F.,(4,3,3,3,3,3,3,3,3,3,3,3,3,
3,3,3,3,4),(-0.36639757900585,-0.355489874273349,-0.328849435073975,-0.31597973424817,
-0.292469703717351,-0.280219243073488,-0.245242540668626,-0.218587119974093,
-0.20792985214368,-0.187225496763673,-0.163822309668214,-0.149605700274317,
-0.13878185835336,-0.10408639376502,-0.0828199205047292,-0.0667724235854585,
-0.0282787680692534,0.),.UNSPECIFIED.);
#485=B_SPLINE_CURVE_WITH_KNOTS('',3,(#37708,#37709,#37710,#37711),
 .UNSPECIFIED.,.F.,.F.,(4,4),(15.2766115956179,15.7079632679489),
 .UNSPECIFIED.);
#486=B_SPLINE_CURVE_WITH_KNOTS('',3,(#37713,#37714,#37715,#37716,#37717,
#37718,#37719,#37720,#37721,#37722,#37723,#37724,#37725,#37726,#37727,#37728,
#37729,#37730,#37731,#37732,#37733,#37734,#37735,#37736,#37737,#37738,#37739,
#37740,#37741,#37742,#37743,#37744,#37745,#37746,#37747,#37748,#37749,#37750,
#37751,#37752,#37753,#37754,#37755,#37756,#37757,#37758,#37759,#37760,#37761,
#37762,#37763,#37764),.UNSPECIFIED.,.F.,.F.,(4,3,3,3,3,3,3,3,3,3,3,3,3,
3,3,3,3,4),(-0.36462930789066,-0.351181914845128,-0.324753847158882,-0.311459613184419,
-0.27471342084418,-0.262559086408708,-0.225887280111663,-0.20168112730567,
-0.18621981366523,-0.166307755252114,-0.130572803308094,-0.119339784451787,
-0.0895048383388406,-0.072935654322955,-0.0625561487919195,-0.0518706577021471,
-0.0196194685578637,0.),.UNSPECIFIED.);
#487=B_SPLINE_CURVE_WITH_KNOTS('',3,(#38148,#38149,#38150,#38151,#38152,
#38153,#38154,#38155,#38156,#38157,#38158,#38159,#38160,#38161,#38162,#38163,
#38164,#38165,#38166,#38167,#38168,#38169,#38170,#38171,#38172,#38173,#38174,
#38175,#38176,#38177,#38178,#38179,#38180,#38181,#38182,#38183,#38184,#38185,
#38186,#38187,#38188,#38189,#38190,#38191,#38192,#38193,#38194,#38195,#38196,
#38197,#38198,#38199),.UNSPECIFIED.,.F.,.F.,(4,3,3,3,3,3,3,3,3,3,3,3,3,
3,3,3,3,4),(-0.366397579005837,-0.355489874273339,-0.328849434310144,-0.315979731231902,
-0.292469839731824,-0.280219291818356,-0.245242586893988,-0.218587212262585,
-0.207929893305042,-0.187225496763668,-0.16382230966821,-0.149605709635192,
-0.138781865725635,-0.104086399294226,-0.0828199340175651,-0.0667724231415902,
-0.0282787740817212,0.),.UNSPECIFIED.);
#488=B_SPLINE_CURVE_WITH_KNOTS('',3,(#38200,#38201,#38202,#38203,#38204,
#38205,#38206,#38207,#38208,#38209,#38210,#38211,#38212,#38213,#38214,#38215),
 .UNSPECIFIED.,.F.,.F.,(4,3,3,3,3,4),(-91.8249302358436,-90.8268331680627,
-89.8287361002818,-88.8306390325009,-87.83254196472,-87.1562515097525),
 .UNSPECIFIED.);
#489=B_SPLINE_CURVE_WITH_KNOTS('',3,(#38711,#38712,#38713,#38714,#38715,
#38716,#38717,#38718,#38719,#38720,#38721,#38722,#38723,#38724,#38725,#38726),
 .UNSPECIFIED.,.F.,.F.,(4,3,3,3,3,4),(-6.60529764332039,-5.93959761199661,
-4.94966467666384,-3.95973174133107,-2.9697988059983,-2.07317267331972),
 .UNSPECIFIED.);
#490=B_SPLINE_CURVE_WITH_KNOTS('',3,(#38734,#38735,#38736,#38737,#38738,
#38739,#38740,#38741,#38742,#38743,#38744,#38745,#38746),.UNSPECIFIED.,
 .F.,.F.,(4,3,3,3,4),(0.,0.989932935332755,1.97986587066553,2.9697988059983,
3.63601592933276),.UNSPECIFIED.);
#491=B_SPLINE_CURVE_WITH_KNOTS('',3,(#38751,#38752,#38753,#38754,#38755,
#38756,#38757,#38758,#38759,#38760,#38761,#38762,#38763,#38764,#38765,#38766,
#38767,#38768,#38769,#38770,#38771,#38772,#38773,#38774,#38775),
 .UNSPECIFIED.,.F.,.F.,(4,3,3,3,3,3,3,3,4),(-12.8884829505,-12.869128159326,
-11.8791952239932,-10.8892622886604,-9.89932935332768,-8.90939641799491,
-7.91946348266214,-6.92953054732937,-6.60529764332039),.UNSPECIFIED.);
#492=B_SPLINE_CURVE_WITH_KNOTS('',3,(#38776,#38777,#38778,#38779,#38780,
#38781,#38782,#38783,#38784,#38785,#38786,#38787,#38788,#38789,#38790,#38791,
#38792,#38793,#38794,#38795,#38796,#38797,#38798,#38799,#38800),
 .UNSPECIFIED.,.F.,.F.,(4,3,3,3,3,3,3,3,4),(3.63601592933276,3.95973174133107,
4.94966467666384,5.93959761199661,6.92953054732937,7.91946348266214,8.90939641799491,
9.89932935332767,9.91920123651235),.UNSPECIFIED.);
#493=B_SPLINE_CURVE_WITH_KNOTS('',3,(#38805,#38806,#38807,#38808,#38809,
#38810,#38811,#38812,#38813,#38814,#38815,#38816,#38817,#38818,#38819,#38820,
#38821,#38822,#38823,#38824,#38825,#38826),.UNSPECIFIED.,.F.,.F.,(4,3,3,
3,3,3,3,4),(-19.1716682576796,-18.8087257713226,-17.8187928359898,-16.8288599006571,
-15.8389269653243,-14.8489940299915,-13.8590610946588,-12.8884829505),
 .UNSPECIFIED.);
#494=B_SPLINE_CURVE_WITH_KNOTS('',3,(#38827,#38828,#38829,#38830,#38831,
#38832,#38833,#38834,#38835,#38836,#38837,#38838,#38839,#38840,#38841,#38842,
#38843,#38844,#38845,#38846,#38847,#38848),.UNSPECIFIED.,.F.,.F.,(4,3,3,
3,3,3,3,4),(9.91920123651235,10.8892622886604,11.8791952239932,12.869128159326,
13.8590610946587,14.8489940299915,15.8389269653243,16.2023865436919),
 .UNSPECIFIED.);
#495=B_SPLINE_CURVE_WITH_KNOTS('',3,(#38853,#38854,#38855,#38856,#38857,
#38858,#38859,#38860,#38861,#38862,#38863,#38864,#38865,#38866,#38867,#38868,
#38869,#38870,#38871,#38872,#38873,#38874),.UNSPECIFIED.,.F.,.F.,(4,3,3,
3,3,3,3,4),(-25.4548535648592,-24.7483233833192,-23.7583904479864,-22.7684575126537,
-21.7785245773209,-20.7885916419881,-19.7986587066553,-19.1716682576796),
 .UNSPECIFIED.);
#496=B_SPLINE_CURVE_WITH_KNOTS('',3,(#38875,#38876,#38877,#38878,#38879,
#38880,#38881,#38882,#38883,#38884,#38885,#38886,#38887,#38888,#38889,#38890,
#38891,#38892,#38893,#38894,#38895,#38896),.UNSPECIFIED.,.F.,.F.,(4,3,3,
3,3,3,3,4),(16.2023865436919,16.828859900657,17.8187928359898,18.8087257713226,
19.7986587066553,20.7885916419881,21.7785245773209,22.4855718508715),
 .UNSPECIFIED.);
#497=B_SPLINE_CURVE_WITH_KNOTS('',3,(#38901,#38902,#38903,#38904,#38905,
#38906,#38907,#38908,#38909,#38910,#38911,#38912,#38913,#38914,#38915,#38916,
#38917,#38918,#38919,#38920,#38921,#38922,#38923,#38924,#38925),
 .UNSPECIFIED.,.F.,.F.,(4,3,3,3,3,3,3,3,4),(-31.7380388720387,-31.6778539306486,
-30.6879209953158,-29.697988059983,-28.7080551246503,-27.7181221893175,
-26.7281892539847,-25.738256318652,-25.4548535648592),.UNSPECIFIED.);
#498=B_SPLINE_CURVE_WITH_KNOTS('',3,(#38926,#38927,#38928,#38929,#38930,
#38931,#38932,#38933,#38934,#38935,#38936,#38937,#38938,#38939,#38940,#38941,
#38942,#38943,#38944,#38945,#38946,#38947,#38948,#38949,#38950),
 .UNSPECIFIED.,.F.,.F.,(4,3,3,3,3,3,3,3,4),(22.4855718508715,22.7684575126537,
23.7583904479864,24.7483233833192,25.738256318652,26.7281892539847,27.7181221893175,
28.7080551246503,28.7687571580511),.UNSPECIFIED.);
#499=B_SPLINE_CURVE_WITH_KNOTS('',3,(#38955,#38956,#38957,#38958,#38959,
#38960,#38961,#38962,#38963,#38964,#38965,#38966,#38967,#38968,#38969,#38970,
#38971,#38972,#38973,#38974,#38975,#38976),.UNSPECIFIED.,.F.,.F.,(4,3,3,
3,3,3,3,4),(-38.0212241792183,-37.6174515426452,-36.6275186073124,-35.6375856719796,
-34.6476527366469,-33.6577198013141,-32.6677868659813,-31.7380388720387),
 .UNSPECIFIED.);
#500=B_SPLINE_CURVE_WITH_KNOTS('',3,(#38977,#38978,#38979,#38980,#38981,
#38982,#38983,#38984,#38985,#38986,#38987,#38988,#38989,#38990,#38991,#38992,
#38993,#38994,#38995,#38996,#38997,#38998),.UNSPECIFIED.,.F.,.F.,(4,3,3,
3,3,3,3,4),(28.7687571580511,29.697988059983,30.6879209953158,31.6778539306486,
32.6677868659813,33.6577198013141,34.6476527366469,35.0519424652307),
 .UNSPECIFIED.);
#501=B_SPLINE_CURVE_WITH_KNOTS('',3,(#39003,#39004,#39005,#39006,#39007,
#39008,#39009,#39010,#39011,#39012,#39013,#39014,#39015,#39016,#39017,#39018,
#39019,#39020,#39021,#39022,#39023,#39024),.UNSPECIFIED.,.F.,.F.,(4,3,3,
3,3,3,3,4),(-44.3044094863979,-43.5570491546418,-42.567116219309,-41.5771832839762,
-40.5872503486435,-39.5973174133107,-38.6073844779779,-38.0212241792183),
 .UNSPECIFIED.);
#502=B_SPLINE_CURVE_WITH_KNOTS('',3,(#39025,#39026,#39027,#39028,#39029,
#39030,#39031,#39032,#39033,#39034,#39035,#39036,#39037,#39038,#39039,#39040,
#39041,#39042,#39043,#39044,#39045,#39046),.UNSPECIFIED.,.F.,.F.,(4,3,3,
3,3,3,3,4),(35.0519424652307,35.6375856719796,36.6275186073124,37.6174515426452,
38.6073844779779,39.5973174133107,40.5872503486435,41.3351277724103),
 .UNSPECIFIED.);
#503=B_SPLINE_CURVE_WITH_KNOTS('',3,(#39051,#39052,#39053,#39054,#39055,
#39056,#39057,#39058,#39059,#39060,#39061,#39062,#39063,#39064,#39065,#39066,
#39067,#39068,#39069,#39070,#39071,#39072,#39073,#39074,#39075),
 .UNSPECIFIED.,.F.,.F.,(4,3,3,3,3,3,3,3,4),(-50.5875947935775,-50.4865797019712,
-49.4966467666384,-48.5067138313056,-47.5167808959729,-46.5268479606401,
-45.5369150253073,-44.5469820899746,-44.3044094863979),.UNSPECIFIED.);
#504=B_SPLINE_CURVE_WITH_KNOTS('',3,(#39076,#39077,#39078,#39079,#39080,
#39081,#39082,#39083,#39084,#39085,#39086,#39087,#39088,#39089,#39090,#39091,
#39092,#39093,#39094,#39095,#39096,#39097,#39098,#39099,#39100),
 .UNSPECIFIED.,.F.,.F.,(4,3,3,3,3,3,3,3,4),(41.3351277724103,41.5771832839762,
42.567116219309,43.5570491546418,44.5469820899745,45.5369150253073,46.5268479606401,
47.5167808959728,47.6183130795899),.UNSPECIFIED.);
#505=B_SPLINE_CURVE_WITH_KNOTS('',3,(#39105,#39106,#39107,#39108,#39109,
#39110,#39111,#39112,#39113,#39114,#39115,#39116,#39117,#39118,#39119,#39120,
#39121,#39122,#39123,#39124,#39125,#39126),.UNSPECIFIED.,.F.,.F.,(4,3,3,
3,3,3,3,4),(-56.8707801007571,-56.4261773139678,-55.436244378635,-54.4463114433022,
-53.4563785079695,-52.4664455726367,-51.4765126373039,-50.5875947935775),
 .UNSPECIFIED.);
#506=B_SPLINE_CURVE_WITH_KNOTS('',3,(#39127,#39128,#39129,#39130,#39131,
#39132,#39133,#39134,#39135,#39136,#39137,#39138,#39139,#39140,#39141,#39142,
#39143,#39144,#39145,#39146,#39147,#39148),.UNSPECIFIED.,.F.,.F.,(4,3,3,
3,3,3,3,4),(47.6183130795899,48.5067138313056,49.4966467666384,50.4865797019711,
51.4765126373039,52.4664455726367,53.4563785079694,53.9014983867695),
 .UNSPECIFIED.);
#507=B_SPLINE_CURVE_WITH_KNOTS('',3,(#39153,#39154,#39155,#39156,#39157,
#39158,#39159,#39160,#39161,#39162,#39163,#39164,#39165,#39166,#39167,#39168,
#39169,#39170,#39171,#39172,#39173,#39174),.UNSPECIFIED.,.F.,.F.,(4,3,3,
3,3,3,3,4),(-63.1539654079367,-62.3657749259644,-61.3758419906316,-60.3859090552988,
-59.3959761199661,-58.4060431846333,-57.4161102493005,-56.8707801007571),
 .UNSPECIFIED.);
#508=B_SPLINE_CURVE_WITH_KNOTS('',3,(#39175,#39176,#39177,#39178,#39179,
#39180,#39181,#39182,#39183,#39184,#39185,#39186,#39187,#39188,#39189,#39190,
#39191,#39192,#39193,#39194,#39195,#39196),.UNSPECIFIED.,.F.,.F.,(4,3,3,
3,3,3,3,4),(53.9014983867695,54.4463114433022,55.436244378635,56.4261773139677,
57.4161102493005,58.4060431846333,59.3959761199661,60.1846836939491),
 .UNSPECIFIED.);
#509=B_SPLINE_CURVE_WITH_KNOTS('',3,(#39201,#39202,#39203,#39204,#39205,
#39206,#39207,#39208,#39209,#39210,#39211,#39212,#39213,#39214,#39215,#39216,
#39217,#39218,#39219,#39220,#39221,#39222,#39223,#39224,#39225),
 .UNSPECIFIED.,.F.,.F.,(4,3,3,3,3,3,3,3,4),(-69.4371507151163,-69.2953054732937,
-68.305372537961,-67.3154396026282,-66.3255066672954,-65.3355737319627,
-64.3456407966299,-63.3557078612971,-63.1539654079367),.UNSPECIFIED.);
#510=B_SPLINE_CURVE_WITH_KNOTS('',3,(#39226,#39227,#39228,#39229,#39230,
#39231,#39232,#39233,#39234,#39235,#39236,#39237,#39238,#39239,#39240,#39241,
#39242,#39243,#39244,#39245,#39246,#39247,#39248,#39249,#39250),
 .UNSPECIFIED.,.F.,.F.,(4,3,3,3,3,3,3,3,4),(60.1846836939491,60.3859090552988,
61.3758419906316,62.3657749259644,63.3557078612971,64.3456407966299,65.3355737319627,
66.3255066672954,66.4678690011287),.UNSPECIFIED.);
#511=B_SPLINE_CURVE_WITH_KNOTS('',3,(#39255,#39256,#39257,#39258,#39259,
#39260,#39261,#39262,#39263,#39264,#39265,#39266,#39267,#39268,#39269,#39270,
#39271,#39272,#39273,#39274,#39275,#39276),.UNSPECIFIED.,.F.,.F.,(4,3,3,
3,3,3,3,4),(-75.7203360222959,-75.2349030852904,-74.2449701499576,-73.2550372146248,
-72.2651042792921,-71.2751713439593,-70.2852384086265,-69.4371507151163),
 .UNSPECIFIED.);
#512=B_SPLINE_CURVE_WITH_KNOTS('',3,(#39277,#39278,#39279,#39280,#39281,
#39282,#39283,#39284,#39285,#39286,#39287,#39288,#39289,#39290,#39291,#39292,
#39293,#39294,#39295,#39296,#39297,#39298),.UNSPECIFIED.,.F.,.F.,(4,3,3,
3,3,3,3,4),(66.4678690011287,67.3154396026282,68.3053725379609,69.2953054732937,
70.2852384086265,71.2751713439593,72.265104279292,72.7510543083083),
 .UNSPECIFIED.);
#513=B_SPLINE_CURVE_WITH_KNOTS('',3,(#39303,#39304,#39305,#39306,#39307,
#39308,#39309,#39310,#39311,#39312,#39313,#39314,#39315,#39316,#39317,#39318,
#39319,#39320,#39321,#39322,#39323,#39324),.UNSPECIFIED.,.F.,.F.,(4,3,3,
3,3,3,3,4),(-82.0035213294755,-81.174500697287,-80.1845677619542,-79.1946348266214,
-78.2047018912887,-77.2147689559559,-76.2248360206231,-75.7203360222959),
 .UNSPECIFIED.);
#514=B_SPLINE_CURVE_WITH_KNOTS('',3,(#39325,#39326,#39327,#39328,#39329,
#39330,#39331,#39332,#39333,#39334,#39335,#39336,#39337,#39338,#39339,#39340,
#39341,#39342,#39343,#39344,#39345,#39346),.UNSPECIFIED.,.F.,.F.,(4,3,3,
3,3,3,3,4),(72.7510543083083,73.2550372146248,74.2449701499576,75.2349030852903,
76.2248360206231,77.2147689559559,78.2047018912886,79.0342396154878),
 .UNSPECIFIED.);
#515=B_SPLINE_CURVE_WITH_KNOTS('',3,(#39351,#39352,#39353,#39354,#39355,
#39356,#39357,#39358,#39359,#39360,#39361,#39362,#39363,#39364,#39365,#39366,
#39367,#39368,#39369,#39370,#39371,#39372,#39373,#39374,#39375),
 .UNSPECIFIED.,.F.,.F.,(4,3,3,3,3,3,3,3,4),(-88.2867066366551,-88.1040312446163,
-87.1140983092836,-86.1241653739508,-85.134232438618,-84.1442995032853,
-83.1543665679525,-82.1644336326197,-82.0035213294755),.UNSPECIFIED.);
#516=B_SPLINE_CURVE_WITH_KNOTS('',3,(#39376,#39377,#39378,#39379,#39380,
#39381,#39382,#39383,#39384,#39385,#39386,#39387,#39388,#39389,#39390,#39391,
#39392,#39393,#39394,#39395,#39396,#39397,#39398,#39399,#39400),
 .UNSPECIFIED.,.F.,.F.,(4,3,3,3,3,3,3,3,4),(79.0342396154878,79.1946348266214,
80.1845677619542,81.1745006972869,82.1644336326197,83.1543665679525,84.1442995032852,
85.134232438618,85.3174249226674),.UNSPECIFIED.);
#517=B_SPLINE_CURVE_WITH_KNOTS('',3,(#39406,#39407,#39408,#39409,#39410,
#39411),.UNSPECIFIED.,.F.,.F.,(4,1,1,4),(103.672557568463,104.479815111757,
105.46974804709,106.366374179769),.UNSPECIFIED.);
#518=B_SPLINE_CURVE_WITH_KNOTS('',3,(#39414,#39415,#39416,#39417,#39418),
 .UNSPECIFIED.,.F.,.F.,(4,1,4),(103.672557568463,104.135710324563,105.125643259896),
 .UNSPECIFIED.);
#519=B_SPLINE_CURVE_WITH_KNOTS('',3,(#39423,#39424,#39425,#39426,#39427,
#39428,#39429,#39430,#39431,#39432,#39433),.UNSPECIFIED.,.F.,.F.,(4,1,1,
1,1,1,1,1,4),(97.3893722612836,97.5502845644278,98.5402174997606,99.5301504350933,
100.520083370426,101.510016305759,102.499949241092,103.489882176424,103.672557568463),
 .UNSPECIFIED.);
#520=B_SPLINE_CURVE_WITH_KNOTS('',3,(#39434,#39435,#39436,#39437,#39438,
#39439,#39440,#39441,#39442,#39443),.UNSPECIFIED.,.F.,.F.,(4,1,1,1,1,1,
1,4),(97.3893722612836,98.1961127125668,99.1860456478996,100.175978583232,
101.165911518565,102.155844453898,103.145777389231,103.672557568463),
 .UNSPECIFIED.);
#521=B_SPLINE_CURVE_WITH_KNOTS('',3,(#39448,#39449,#39450,#39451,#39452,
#39453,#39454,#39455,#39456,#39457),.UNSPECIFIED.,.F.,.F.,(4,1,1,1,1,1,
1,4),(91.106186954104,91.6106869524312,92.600619887764,93.5905528230967,
94.5804857584295,95.5704186937623,96.560351629095,97.3893722612836),
 .UNSPECIFIED.);
#522=B_SPLINE_CURVE_WITH_KNOTS('',3,(#39458,#39459,#39460,#39461,#39462,
#39463,#39464,#39465,#39466,#39467,#39468),.UNSPECIFIED.,.F.,.F.,(4,1,1,
1,1,1,1,1,4),(91.106186954104,91.2665821652374,92.2565151005702,93.246448035903,
94.2363809712357,95.2263139065685,96.2162468419013,97.206179777234,97.3893722612836),
 .UNSPECIFIED.);
#523=B_SPLINE_CURVE_WITH_KNOTS('',3,(#39473,#39474,#39475,#39476,#39477,
#39478,#39479,#39480,#39481,#39482),.UNSPECIFIED.,.F.,.F.,(4,1,1,1,1,1,
1,4),(84.8230016469244,85.6710893404346,86.6610222757674,87.6509552111001,
88.6408881464329,89.6308210817657,90.6207540170984,91.106186954104),
 .UNSPECIFIED.);
#524=B_SPLINE_CURVE_WITH_KNOTS('',3,(#39483,#39484,#39485,#39486,#39487,
#39488,#39489,#39490,#39491,#39492),.UNSPECIFIED.,.F.,.F.,(4,1,1,1,1,1,
1,4),(84.8230016469244,85.3269845532408,86.3169174885736,87.3068504239064,
88.2967833592391,89.2867162945719,90.2766492299047,91.106186954104),
 .UNSPECIFIED.);
#525=B_SPLINE_CURVE_WITH_KNOTS('',3,(#39497,#39498,#39499,#39500,#39501,
#39502,#39503,#39504,#39505,#39506,#39507),.UNSPECIFIED.,.F.,.F.,(4,1,1,
1,1,1,1,1,4),(78.5398163397448,78.7415587931052,79.731491728438,80.7214246637707,
81.7113575991035,82.7012905344363,83.6912234697691,84.6811564051018,84.8230016469244),
 .UNSPECIFIED.);
#526=B_SPLINE_CURVE_WITH_KNOTS('',3,(#39508,#39509,#39510,#39511,#39512,
#39513,#39514,#39515,#39516,#39517),.UNSPECIFIED.,.F.,.F.,(4,1,1,1,1,1,
1,4),(78.5398163397448,79.3873869412442,80.377319876577,81.3672528119098,
82.3571857472425,83.3471186825753,84.3370516179081,84.8230016469244),
 .UNSPECIFIED.);
#527=B_SPLINE_CURVE_WITH_KNOTS('',3,(#39522,#39523,#39524,#39525,#39526,
#39527,#39528,#39529,#39530,#39531),.UNSPECIFIED.,.F.,.F.,(4,1,1,1,1,1,
1,4),(72.2566310325652,72.8019611811086,73.7918941164414,74.7818270517741,
75.7717599871069,76.7616929224397,77.7516258577724,78.5398163397448),
 .UNSPECIFIED.);
#528=B_SPLINE_CURVE_WITH_KNOTS('',3,(#39532,#39533,#39534,#39535,#39536,
#39537,#39538,#39539,#39540,#39541,#39542),.UNSPECIFIED.,.F.,.F.,(4,1,1,
1,1,1,1,1,4),(72.2566310325652,72.4578563939149,73.4477893292476,74.4377222645804,
75.4276551999132,76.4175881352459,77.4075210705787,78.3974540059115,78.5398163397448),
 .UNSPECIFIED.);
#529=B_SPLINE_CURVE_WITH_KNOTS('',3,(#39547,#39548,#39549,#39550,#39551,
#39552,#39553,#39554,#39555,#39556),.UNSPECIFIED.,.F.,.F.,(4,1,1,1,1,1,
1,4),(65.9734457253856,66.862363569112,67.8522965044448,68.8422294397775,
69.8321623751103,70.8220953104431,71.8120282457758,72.2566310325652),
 .UNSPECIFIED.);
#530=B_SPLINE_CURVE_WITH_KNOTS('',3,(#39557,#39558,#39559,#39560,#39561,
#39562,#39563,#39564,#39565,#39566),.UNSPECIFIED.,.F.,.F.,(4,1,1,1,1,1,
1,4),(65.9734457253856,66.5182587819182,67.508191717251,68.4981246525838,
69.4880575879166,70.4779905232493,71.4679234585821,72.2566310325652),
 .UNSPECIFIED.);
#531=B_SPLINE_CURVE_WITH_KNOTS('',3,(#39571,#39572,#39573,#39574,#39575,
#39576,#39577,#39578,#39579,#39580,#39581),.UNSPECIFIED.,.F.,.F.,(4,1,1,
1,1,1,1,1,4),(59.690260418206,59.9328330217826,60.9227659571154,61.9126988924482,
62.9026318277809,63.8925647631137,64.8824976984465,65.8724306337792,65.9734457253856),
 .UNSPECIFIED.);
#532=B_SPLINE_CURVE_WITH_KNOTS('',3,(#39582,#39583,#39584,#39585,#39586,
#39587,#39588,#39589,#39590,#39591),.UNSPECIFIED.,.F.,.F.,(4,1,1,1,1,1,
1,4),(59.690260418206,60.5786611699216,61.5685941052544,62.5585270405872,
63.54845997592,64.5383929112527,65.5283258465855,65.9734457253856),
 .UNSPECIFIED.);
#533=B_SPLINE_CURVE_WITH_KNOTS('',3,(#39596,#39597,#39598,#39599,#39600,
#39601,#39602,#39603,#39604,#39605),.UNSPECIFIED.,.F.,.F.,(4,1,1,1,1,1,
1,4),(53.4070751110264,53.993235409786,54.9831683451188,55.9731012804516,
56.9630342157843,57.9529671511171,58.9429000864499,59.690260418206),
 .UNSPECIFIED.);
#534=B_SPLINE_CURVE_WITH_KNOTS('',3,(#39606,#39607,#39608,#39609,#39610,
#39611,#39612,#39613,#39614,#39615,#39616),.UNSPECIFIED.,.F.,.F.,(4,1,1,
1,1,1,1,1,4),(53.4070751110264,53.6491306225923,54.639063557925,55.6289964932578,
56.6189294285906,57.6088623639234,58.5987952992561,59.5887282345889,59.690260418206),
 .UNSPECIFIED.);
#535=B_SPLINE_CURVE_WITH_KNOTS('',3,(#39621,#39622,#39623,#39624,#39625,
#39626,#39627,#39628,#39629,#39630),.UNSPECIFIED.,.F.,.F.,(4,1,1,1,1,1,
1,4),(47.1238898038469,48.0536377977894,49.0435707331222,50.0335036684549,
51.0234366037877,52.0133695391205,53.0033024744532,53.4070751110264),
 .UNSPECIFIED.);
#536=B_SPLINE_CURVE_WITH_KNOTS('',3,(#39631,#39632,#39633,#39634,#39635,
#39636,#39637,#39638,#39639,#39640),.UNSPECIFIED.,.F.,.F.,(4,1,1,1,1,1,
1,4),(47.1238898038468,47.7095330105957,48.6994659459284,49.6893988812612,
50.679331816594,51.6692647519267,52.6591976872595,53.4070751110264),
 .UNSPECIFIED.);
#537=B_SPLINE_CURVE_WITH_KNOTS('',3,(#39645,#39646,#39647,#39648,#39649,
#39650,#39651,#39652,#39653,#39654,#39655),.UNSPECIFIED.,.F.,.F.,(4,1,1,
1,1,1,1,1,4),(40.8407044966673,41.12410725046,42.1140401857928,43.1039731211256,
44.0939060564583,45.0838389917911,46.0737719271239,47.0637048624566,47.1238898038469),
 .UNSPECIFIED.);
#538=B_SPLINE_CURVE_WITH_KNOTS('',3,(#39656,#39657,#39658,#39659,#39660,
#39661,#39662,#39663,#39664,#39665),.UNSPECIFIED.,.F.,.F.,(4,1,1,1,1,1,
1,4),(40.8407044966672,41.7699353985991,42.7598683339318,43.7498012692646,
44.7397342045974,45.7296671399301,46.7196000752629,47.1238898038468),
 .UNSPECIFIED.);
#539=B_SPLINE_CURVE_WITH_KNOTS('',3,(#39670,#39671,#39672,#39673,#39674,
#39675,#39676,#39677,#39678,#39679),.UNSPECIFIED.,.F.,.F.,(4,1,1,1,1,1,
1,4),(34.5575191894877,35.1845096384634,36.1744425737962,37.164375509129,
38.1543084444617,39.1442413797945,40.1341743151273,40.8407044966673),
 .UNSPECIFIED.);
#540=B_SPLINE_CURVE_WITH_KNOTS('',3,(#39680,#39681,#39682,#39683,#39684,
#39685,#39686,#39687,#39688,#39689,#39690),.UNSPECIFIED.,.F.,.F.,(4,1,1,
1,1,1,1,1,4),(34.5575191894876,34.8404048512697,35.8303377866025,36.8202707219352,
37.810203657268,38.8001365926008,39.7900695279335,40.7800024632663,40.8407044966672),
 .UNSPECIFIED.);
#541=B_SPLINE_CURVE_WITH_KNOTS('',3,(#39695,#39696,#39697,#39698,#39699,
#39700,#39701,#39702,#39703,#39704),.UNSPECIFIED.,.F.,.F.,(4,1,1,1,1,1,
1,4),(28.2743338823081,29.2449120264668,30.2348449617996,31.2247778971324,
32.2147108324651,33.2046437677979,34.1945767031307,34.5575191894877),
 .UNSPECIFIED.);
#542=B_SPLINE_CURVE_WITH_KNOTS('',3,(#39705,#39706,#39707,#39708,#39709,
#39710,#39711,#39712,#39713,#39714),.UNSPECIFIED.,.F.,.F.,(4,1,1,1,1,1,
1,4),(28.2743338823081,28.9008072392731,29.8907401746059,30.8806731099386,
31.8706060452714,32.8605389806042,33.8504719159369,34.5575191894876),
 .UNSPECIFIED.);
#543=B_SPLINE_CURVE_WITH_KNOTS('',3,(#39719,#39720,#39721,#39722,#39723,
#39724,#39725,#39726,#39727,#39728,#39729),.UNSPECIFIED.,.F.,.F.,(4,1,1,
1,1,1,1,1,4),(21.9911485751285,22.3153814791375,23.3053144144702,24.295247349803,
25.2851802851358,26.2751132204685,27.2650461558013,28.2549790911341,28.2743338823081),
 .UNSPECIFIED.);
#544=B_SPLINE_CURVE_WITH_KNOTS('',3,(#39730,#39731,#39732,#39733,#39734,
#39735,#39736,#39737,#39738,#39739),.UNSPECIFIED.,.F.,.F.,(4,1,1,1,1,1,
1,4),(21.9911485751285,22.9612096272765,23.9511425626093,24.941075497942,
25.9310084332748,26.9209413686076,27.9108743039403,28.2743338823081),
 .UNSPECIFIED.);
#545=B_SPLINE_CURVE_WITH_KNOTS('',3,(#39744,#39745,#39746,#39747,#39748,
#39749,#39750,#39751,#39752,#39753),.UNSPECIFIED.,.F.,.F.,(4,1,1,1,1,1,
1,4),(15.7079632679489,16.3757838671408,17.3657168024736,18.3556497378064,
19.3455826731391,20.3355156084719,21.3254485438047,21.9911485751285),
 .UNSPECIFIED.);
#546=B_SPLINE_CURVE_WITH_KNOTS('',3,(#39754,#39755,#39756,#39757,#39758,
#39759,#39760,#39761,#39762,#39763,#39764),.UNSPECIFIED.,.F.,.F.,(4,1,1,
1,1,1,1,1,4),(15.7079632679489,16.0316790799471,17.0216120152799,18.0115449506126,
19.0014778859454,19.9914108212782,20.981343756611,21.9712766919437,21.9911485751285),
 .UNSPECIFIED.);
#547=B_SPLINE_CURVE_WITH_KNOTS('',3,(#39767,#39768,#39769,#39770,#39771,
#39772,#39773,#39774,#39775,#39776,#39777,#39778,#39779,#39780,#39781,#39782,
#39783,#39784,#39785,#39786,#39787,#39788,#39789,#39790,#39791,#39792,#39793,
#39794,#39795,#39796,#39797,#39798,#39799,#39800,#39801,#39802,#39803,#39804,
#39805,#39806,#39807,#39808,#39809,#39810,#39811,#39812,#39813,#39814,#39815,
#39816,#39817,#39818),.UNSPECIFIED.,.F.,.F.,(4,3,3,3,3,3,3,3,3,3,3,3,3,
3,3,3,3,4),(-0.276631791712713,-0.265450615480059,-0.249264708457004,-0.237962300703026,
-0.216900919589401,-0.204366916455402,-0.175872487121073,-0.164709026212586,
-0.155425879325222,-0.139389331983085,-0.119813112264589,-0.110539977009441,
-0.100714351836302,-0.0755357638772264,-0.0587460506531512,-0.0492722354456899,
-0.0182560868482527,0.),.UNSPECIFIED.);
#548=B_SPLINE_CURVE_WITH_KNOTS('',3,(#39823,#39824,#39825,#39826,#39827,
#39828,#39829,#39830,#39831,#39832,#39833,#39834,#39835,#39836,#39837,#39838,
#39839,#39840,#39841,#39842,#39843,#39844,#39845,#39846,#39847,#39848,#39849,
#39850,#39851,#39852,#39853,#39854,#39855,#39856,#39857,#39858,#39859,#39860,
#39861,#39862,#39863,#39864,#39865,#39866,#39867,#39868,#39869,#39870,#39871,
#39872,#39873,#39874),.UNSPECIFIED.,.F.,.F.,(4,3,3,3,3,3,3,3,3,3,3,3,3,
3,3,3,3,4),(-0.275362278356883,-0.261744724725805,-0.238870913782049,-0.228431829105,
-0.208394802250592,-0.19788610598297,-0.168242095210859,-0.148132070239196,
-0.139871540977981,-0.124344332175051,-0.106149246467418,-0.0967155779587869,
-0.0875515981565891,-0.0656636986174418,-0.0485611810495529,-0.0406387966505317,
-0.0143836439341371,0.),.UNSPECIFIED.);
#549=B_SPLINE_CURVE_WITH_KNOTS('',3,(#40263,#40264,#40265,#40266,#40267,
#40268,#40269,#40270,#40271,#40272,#40273,#40274,#40275,#40276,#40277,#40278,
#40279,#40280,#40281),.UNSPECIFIED.,.F.,.F.,(4,3,3,3,3,3,4),(85.3174249226674,
86.1241653739508,87.1140983092835,88.1040312446163,89.0939641799491,90.0838971152818,
90.9805232479604),.UNSPECIFIED.);
#550=B_SPLINE_CURVE_WITH_KNOTS('',3,(#40283,#40284,#40285,#40286,#40287,
#40288,#40289,#40290,#40291,#40292,#40293,#40294,#40295,#40296,#40297,#40298,
#40299,#40300,#40301,#40302,#40303,#40304,#40305,#40306,#40307,#40308,#40309,
#40310,#40311,#40312,#40313,#40314,#40315,#40316,#40317,#40318,#40319,#40320,
#40321,#40322,#40323,#40324,#40325,#40326,#40327,#40328,#40329,#40330,#40331,
#40332,#40333,#40334),.UNSPECIFIED.,.F.,.F.,(4,3,3,3,3,3,3,3,3,3,3,3,3,
3,3,3,3,4),(-0.276631791712722,-0.265450615480067,-0.249264709520642,-0.237962301509632,
-0.216900855800476,-0.204366904493779,-0.175872475394542,-0.164708998571383,
-0.15542586941425,-0.139389331983089,-0.119813107263836,-0.110539960157763,
-0.100714348698858,-0.0755357615241436,-0.0587460364870724,-0.0492722247833334,
-0.0182560727479066,0.),.UNSPECIFIED.);
#551=B_SPLINE_CURVE_WITH_KNOTS('',3,(#40335,#40336,#40337,#40338,#40339),
 .UNSPECIFIED.,.F.,.F.,(4,1,4),(14.1451200119358,15.0417461446143,15.7079632679489),
 .UNSPECIFIED.);
#552=B_SPLINE_CURVE_WITH_KNOTS('',3,(#40342,#40343,#40344,#40345,#40346,
#40347,#40348,#40349,#40350,#40351,#40352,#40353,#40354,#40355,#40356,#40357,
#40358,#40359,#40360,#40361,#40362,#40363,#40364,#40365,#40366,#40367,#40368,
#40369,#40370,#40371,#40372,#40373,#40374,#40375,#40376,#40377,#40378,#40379,
#40380,#40381,#40382,#40383,#40384,#40385,#40386,#40387,#40388,#40389,#40390,
#40391,#40392,#40393),.UNSPECIFIED.,.F.,.F.,(4,3,3,3,3,3,3,3,3,3,3,3,3,
3,3,3,3,4),(-0.275362278356887,-0.261744724725805,-0.238870910786292,-0.228431821713149,
-0.208394774728337,-0.197886061305117,-0.168242048891388,-0.148131926718763,
-0.139871336754713,-0.124344332175047,-0.106149407076155,-0.0967158838367153,
-0.0875520936665209,-0.0656640702498907,-0.0485622287413132,-0.0406402635470369,
-0.0143850804576057,0.),.UNSPECIFIED.);
#553=B_SPLINE_CURVE_WITH_KNOTS('',3,(#40396,#40397,#40398,#40399),
 .UNSPECIFIED.,.F.,.F.,(4,4),(15.3858509318081,15.7079632679489),
 .UNSPECIFIED.);
#554=B_SPLINE_CURVE_WITH_KNOTS('',3,(#40788,#40789,#40790,#40791,#40792,
#40793,#40794,#40795,#40796,#40797,#40798,#40799,#40800,#40801,#40802,#40803),
 .UNSPECIFIED.,.F.,.F.,(4,3,3,3,3,4),(-93.0536959212802,-92.0637629859474,
-91.0738300506146,-90.0838971152819,-89.0939641799491,-88.2867066366551),
 .UNSPECIFIED.);
#555=B_SPLINE_CURVE_WITH_KNOTS('',3,(#41667,#41668,#41669,#41670,#41671,
#41672,#41673,#41674,#41675,#41676,#41677,#41678,#41679,#41680,#41681,#41682),
 .UNSPECIFIED.,.F.,.F.,(4,3,3,3,3,4),(-6.60529764332032,-5.99211647735971,
-4.99343039779975,-3.9947443182398,-2.99605823867985,-2.07317267331967),
 .UNSPECIFIED.);
#556=B_SPLINE_CURVE_WITH_KNOTS('',3,(#41690,#41691,#41692,#41693,#41694,
#41695,#41696,#41697,#41698,#41699,#41700,#41701,#41702),.UNSPECIFIED.,
 .F.,.F.,(4,3,3,3,4),(0.,0.998686079559959,1.99737215911992,2.99605823867988,
3.63601592933386),.UNSPECIFIED.);
#557=B_SPLINE_CURVE_WITH_KNOTS('',3,(#41707,#41708,#41709,#41710,#41711,
#41712,#41713,#41714,#41715,#41716,#41717,#41718,#41719,#41720,#41721,#41722,
#41723,#41724,#41725,#41726,#41727,#41728),.UNSPECIFIED.,.F.,.F.,(4,3,3,
3,3,3,3,4),(-12.8884829504999,-11.9842329547194,-10.9855468751595,-9.98686079559951,
-8.98817471603956,-7.98948863647961,-6.99080255691966,-6.60529764332032),
 .UNSPECIFIED.);
#558=B_SPLINE_CURVE_WITH_KNOTS('',3,(#41729,#41730,#41731,#41732,#41733,
#41734,#41735,#41736,#41737,#41738,#41739,#41740,#41741,#41742,#41743,#41744,
#41745,#41746,#41747,#41748,#41749,#41750),.UNSPECIFIED.,.F.,.F.,(4,3,3,
3,3,3,3,4),(3.63601592933386,3.99474431823983,4.99343039779978,5.99211647735973,
6.99080255691967,7.98948863647962,8.98817471603956,9.91920123651348),
 .UNSPECIFIED.);
#559=B_SPLINE_CURVE_WITH_KNOTS('',3,(#41755,#41756,#41757,#41758,#41759,
#41760,#41761,#41762,#41763,#41764,#41765,#41766,#41767,#41768,#41769,#41770,
#41771,#41772,#41773,#41774,#41775,#41776,#41777,#41778,#41779),
 .UNSPECIFIED.,.F.,.F.,(4,3,3,3,3,3,3,3,4),(-19.1716682576795,-18.9750355116391,
-17.9763494320791,-16.9776633525192,-15.9789772729592,-14.9802911933993,
-13.9816051138393,-12.9829190342794,-12.8884829504999),.UNSPECIFIED.);
#560=B_SPLINE_CURVE_WITH_KNOTS('',3,(#41780,#41781,#41782,#41783,#41784,
#41785,#41786,#41787,#41788,#41789,#41790,#41791,#41792,#41793,#41794,#41795,
#41796,#41797,#41798,#41799,#41800,#41801,#41802,#41803,#41804),
 .UNSPECIFIED.,.F.,.F.,(4,3,3,3,3,3,3,3,4),(9.91920123651348,9.9868607955995,
10.9855468751595,11.9842329547194,12.9829190342794,13.9816051138393,14.9802911933993,
15.9789772729592,16.202386543693),.UNSPECIFIED.);
#561=B_SPLINE_CURVE_WITH_KNOTS('',3,(#41809,#41810,#41811,#41812,#41813,
#41814,#41815,#41816,#41817,#41818,#41819,#41820,#41821,#41822,#41823,#41824,
#41825,#41826,#41827,#41828,#41829,#41830),.UNSPECIFIED.,.F.,.F.,(4,3,3,
3,3,3,3,4),(-25.4548535648591,-24.9671519889988,-23.9684659094388,-22.9697798298789,
-21.9710937503189,-20.972407670759,-19.973721591199,-19.1716682576795),
 .UNSPECIFIED.);
#562=B_SPLINE_CURVE_WITH_KNOTS('',3,(#41831,#41832,#41833,#41834,#41835,
#41836,#41837,#41838,#41839,#41840,#41841,#41842,#41843,#41844,#41845,#41846,
#41847,#41848,#41849,#41850,#41851,#41852),.UNSPECIFIED.,.F.,.F.,(4,3,3,
3,3,3,3,4),(16.202386543693,16.9776633525192,17.9763494320791,18.9750355116391,
19.973721591199,20.972407670759,21.9710937503189,22.4855718508726),
 .UNSPECIFIED.);
#563=B_SPLINE_CURVE_WITH_KNOTS('',3,(#41857,#41858,#41859,#41860,#41861,
#41862,#41863,#41864,#41865,#41866,#41867,#41868,#41869,#41870,#41871,#41872,
#41873,#41874,#41875,#41876,#41877,#41878),.UNSPECIFIED.,.F.,.F.,(4,3,3,
3,3,3,3,4),(-31.7380388720387,-30.9592684663585,-29.9605823867985,-28.9618963072386,
-27.9632102276786,-26.9645241481187,-25.9658380685587,-25.4548535648591),
 .UNSPECIFIED.);
#564=B_SPLINE_CURVE_WITH_KNOTS('',3,(#41879,#41880,#41881,#41882,#41883,
#41884,#41885,#41886,#41887,#41888,#41889,#41890,#41891,#41892,#41893,#41894,
#41895,#41896,#41897,#41898,#41899,#41900),.UNSPECIFIED.,.F.,.F.,(4,3,3,
3,3,3,3,4),(22.4855718508726,22.9697798298789,23.9684659094388,24.9671519889988,
25.9658380685587,26.9645241481187,27.9632102276786,28.7687571580522),
 .UNSPECIFIED.);
#565=B_SPLINE_CURVE_WITH_KNOTS('',3,(#41905,#41906,#41907,#41908,#41909,
#41910,#41911,#41912,#41913,#41914,#41915,#41916,#41917,#41918,#41919,#41920,
#41921,#41922,#41923,#41924,#41925,#41926,#41927,#41928,#41929),
 .UNSPECIFIED.,.F.,.F.,(4,3,3,3,3,3,3,3,4),(-38.0212241792183,-37.9500710232781,
-36.9513849437182,-35.9526988641582,-34.9540127845983,-33.9553267050383,
-32.9566406254784,-31.9579545459184,-31.7380388720387),.UNSPECIFIED.);
#566=B_SPLINE_CURVE_WITH_KNOTS('',3,(#41930,#41931,#41932,#41933,#41934,
#41935,#41936,#41937,#41938,#41939,#41940,#41941,#41942,#41943,#41944,#41945,
#41946,#41947,#41948,#41949,#41950,#41951,#41952,#41953,#41954),
 .UNSPECIFIED.,.F.,.F.,(4,3,3,3,3,3,3,3,4),(28.7687571580522,28.9618963072386,
29.9605823867985,30.9592684663585,31.9579545459184,32.9566406254784,33.9553267050383,
34.9540127845983,35.0519424652318),.UNSPECIFIED.);
#567=B_SPLINE_CURVE_WITH_KNOTS('',3,(#41959,#41960,#41961,#41962,#41963,
#41964,#41965,#41966,#41967,#41968,#41969,#41970,#41971,#41972,#41973,#41974,
#41975,#41976,#41977,#41978,#41979,#41980),.UNSPECIFIED.,.F.,.F.,(4,3,3,
3,3,3,3,4),(-44.3044094863979,-43.9421875006378,-42.9435014210779,-41.9448153415179,
-40.946129261958,-39.947443182398,-38.9487571028381,-38.0212241792183),
 .UNSPECIFIED.);
#568=B_SPLINE_CURVE_WITH_KNOTS('',3,(#41981,#41982,#41983,#41984,#41985,
#41986,#41987,#41988,#41989,#41990,#41991,#41992,#41993,#41994,#41995,#41996,
#41997,#41998,#41999,#42000,#42001,#42002),.UNSPECIFIED.,.F.,.F.,(4,3,3,
3,3,3,3,4),(35.0519424652318,35.9526988641582,36.9513849437182,37.9500710232781,
38.9487571028381,39.947443182398,40.946129261958,41.3351277724114),
 .UNSPECIFIED.);
#569=B_SPLINE_CURVE_WITH_KNOTS('',3,(#42007,#42008,#42009,#42010,#42011,
#42012,#42013,#42014,#42015,#42016,#42017,#42018,#42019,#42020,#42021,#42022,
#42023,#42024,#42025,#42026,#42027,#42028),.UNSPECIFIED.,.F.,.F.,(4,3,3,
3,3,3,3,4),(-50.5875947935774,-49.9343039779976,-48.9356178984376,-47.9369318188777,
-46.9382457393177,-45.9395596597578,-44.9408735801978,-44.3044094863979),
 .UNSPECIFIED.);
#570=B_SPLINE_CURVE_WITH_KNOTS('',3,(#42029,#42030,#42031,#42032,#42033,
#42034,#42035,#42036,#42037,#42038,#42039,#42040,#42041,#42042,#42043,#42044,
#42045,#42046,#42047,#42048,#42049,#42050),.UNSPECIFIED.,.F.,.F.,(4,3,3,
3,3,3,3,4),(41.3351277724114,41.9448153415179,42.9435014210779,43.9421875006379,
44.9408735801978,45.9395596597578,46.9382457393177,47.618313079591),
 .UNSPECIFIED.);
#571=B_SPLINE_CURVE_WITH_KNOTS('',3,(#42055,#42056,#42057,#42058,#42059,
#42060,#42061,#42062,#42063,#42064,#42065,#42066,#42067,#42068,#42069,#42070,
#42071,#42072,#42073,#42074,#42075,#42076),.UNSPECIFIED.,.F.,.F.,(4,3,3,
3,3,3,3,4),(-56.8707801007571,-55.9264204553573,-54.9277343757973,-53.9290482962374,
-52.9303622166774,-51.9316761371175,-50.9329900575575,-50.5875947935774),
 .UNSPECIFIED.);
#572=B_SPLINE_CURVE_WITH_KNOTS('',3,(#42077,#42078,#42079,#42080,#42081,
#42082,#42083,#42084,#42085,#42086,#42087,#42088,#42089,#42090,#42091,#42092,
#42093,#42094,#42095,#42096,#42097,#42098),.UNSPECIFIED.,.F.,.F.,(4,3,3,
3,3,3,3,4),(47.618313079591,47.9369318188777,48.9356178984376,49.9343039779976,
50.9329900575575,51.9316761371175,52.9303622166774,53.9014983867706),
 .UNSPECIFIED.);
#573=B_SPLINE_CURVE_WITH_KNOTS('',3,(#42103,#42104,#42105,#42106,#42107,
#42108,#42109,#42110,#42111,#42112,#42113,#42114,#42115,#42116,#42117,#42118,
#42119,#42120,#42121,#42122,#42123,#42124,#42125,#42126,#42127),
 .UNSPECIFIED.,.F.,.F.,(4,3,3,3,3,3,3,3,4),(-63.1539654079367,-62.9172230122769,
-61.918536932717,-60.919850853157,-59.9211647735971,-58.9224786940371,-57.9237926144772,
-56.9251065349172,-56.8707801007571),.UNSPECIFIED.);
#574=B_SPLINE_CURVE_WITH_KNOTS('',3,(#42128,#42129,#42130,#42131,#42132,
#42133,#42134,#42135,#42136,#42137,#42138,#42139,#42140,#42141,#42142,#42143,
#42144,#42145,#42146,#42147,#42148,#42149,#42150,#42151,#42152),
 .UNSPECIFIED.,.F.,.F.,(4,3,3,3,3,3,3,3,4),(53.9014983867706,53.9290482962374,
54.9277343757973,55.9264204553573,56.9251065349172,57.9237926144772,58.9224786940371,
59.9211647735971,60.1846836939502),.UNSPECIFIED.);
#575=B_SPLINE_CURVE_WITH_KNOTS('',3,(#42157,#42158,#42159,#42160,#42161,
#42162,#42163,#42164,#42165,#42166,#42167,#42168,#42169,#42170,#42171,#42172,
#42173,#42174,#42175,#42176,#42177,#42178),.UNSPECIFIED.,.F.,.F.,(4,3,3,
3,3,3,3,4),(-69.4371507151162,-68.9093394896366,-67.9106534100767,-66.9119673305167,
-65.9132812509568,-64.9145951713968,-63.9159090918369,-63.1539654079367),
 .UNSPECIFIED.);
#576=B_SPLINE_CURVE_WITH_KNOTS('',3,(#42179,#42180,#42181,#42182,#42183,
#42184,#42185,#42186,#42187,#42188,#42189,#42190,#42191,#42192,#42193,#42194,
#42195,#42196,#42197,#42198,#42199,#42200),.UNSPECIFIED.,.F.,.F.,(4,3,3,
3,3,3,3,4),(60.1846836939502,60.919850853157,61.918536932717,62.9172230122769,
63.9159090918369,64.9145951713968,65.9132812509568,66.4678690011298),
 .UNSPECIFIED.);
#577=B_SPLINE_CURVE_WITH_KNOTS('',3,(#42205,#42206,#42207,#42208,#42209,
#42210,#42211,#42212,#42213,#42214,#42215,#42216,#42217,#42218,#42219,#42220,
#42221,#42222,#42223,#42224,#42225,#42226),.UNSPECIFIED.,.F.,.F.,(4,3,3,
3,3,3,3,4),(-75.7203360222958,-74.9014559669963,-73.9027698874364,-72.9040838078764,
-71.9053977283165,-70.9067116487565,-69.9080255691966,-69.4371507151162),
 .UNSPECIFIED.);
#578=B_SPLINE_CURVE_WITH_KNOTS('',3,(#42227,#42228,#42229,#42230,#42231,
#42232,#42233,#42234,#42235,#42236,#42237,#42238,#42239,#42240,#42241,#42242,
#42243,#42244,#42245,#42246,#42247,#42248),.UNSPECIFIED.,.F.,.F.,(4,3,3,
3,3,3,3,4),(66.4678690011298,66.9119673305167,67.9106534100767,68.9093394896366,
69.9080255691966,70.9067116487565,71.9053977283165,72.7510543083093),
 .UNSPECIFIED.);
#579=B_SPLINE_CURVE_WITH_KNOTS('',3,(#42253,#42254,#42255,#42256,#42257,
#42258,#42259,#42260,#42261,#42262,#42263,#42264,#42265,#42266,#42267,#42268,
#42269,#42270,#42271,#42272,#42273,#42274,#42275,#42276,#42277),
 .UNSPECIFIED.,.F.,.F.,(4,3,3,3,3,3,3,3,4),(-82.0035213294754,-81.892258523916,
-80.8935724443561,-79.8948863647961,-78.8962002852361,-77.8975142056762,
-76.8988281261162,-75.9001420465563,-75.7203360222958),.UNSPECIFIED.);
#580=B_SPLINE_CURVE_WITH_KNOTS('',3,(#42278,#42279,#42280,#42281,#42282,
#42283,#42284,#42285,#42286,#42287,#42288,#42289,#42290,#42291,#42292,#42293,
#42294,#42295,#42296,#42297,#42298,#42299,#42300,#42301,#42302),
 .UNSPECIFIED.,.F.,.F.,(4,3,3,3,3,3,3,3,4),(72.7510543083093,72.9040838078765,
73.9027698874364,74.9014559669964,75.9001420465563,76.8988281261163,77.8975142056762,
78.8962002852362,79.034239615489),.UNSPECIFIED.);
#581=B_SPLINE_CURVE_WITH_KNOTS('',3,(#42307,#42308,#42309,#42310,#42311,
#42312,#42313,#42314,#42315,#42316,#42317,#42318,#42319,#42320,#42321,#42322,
#42323,#42324,#42325,#42326,#42327,#42328),.UNSPECIFIED.,.F.,.F.,(4,3,3,
3,3,3,3,4),(-88.286706636655,-87.8843750012757,-86.8856889217157,-85.8870028421558,
-84.8883167625958,-83.8896306830359,-82.8909446034759,-82.0035213294754),
 .UNSPECIFIED.);
#582=B_SPLINE_CURVE_WITH_KNOTS('',3,(#42329,#42330,#42331,#42332,#42333,
#42334,#42335,#42336,#42337,#42338,#42339,#42340,#42341,#42342,#42343,#42344,
#42345,#42346,#42347,#42348,#42349,#42350),.UNSPECIFIED.,.F.,.F.,(4,3,3,
3,3,3,3,4),(79.034239615489,79.8948863647961,80.8935724443561,81.892258523916,
82.890944603476,83.8896306830359,84.8883167625959,85.3174249226685),
 .UNSPECIFIED.);
#583=B_SPLINE_CURVE_WITH_KNOTS('',3,(#42355,#42356,#42357,#42358,#42359,
#42360,#42361,#42362,#42363,#42364,#42365,#42366,#42367,#42368,#42369,#42370,
#42371,#42372,#42373,#42374,#42375,#42376),.UNSPECIFIED.,.F.,.F.,(4,3,3,
3,3,3,3,4),(-94.5698919438346,-93.8764914786354,-92.8778053990754,-91.8791193195155,
-90.8804332399556,-89.8817471603956,-88.8830610808356,-88.286706636655),
 .UNSPECIFIED.);
#584=B_SPLINE_CURVE_WITH_KNOTS('',3,(#42377,#42378,#42379,#42380,#42381,
#42382,#42383,#42384,#42385,#42386,#42387,#42388,#42389,#42390,#42391,#42392,
#42393,#42394,#42395,#42396,#42397,#42398),.UNSPECIFIED.,.F.,.F.,(4,3,3,
3,3,3,3,4),(85.3174249226685,85.8870028421558,86.8856889217158,87.8843750012757,
88.8830610808357,89.8817471603956,90.8804332399556,91.6006102298481),
 .UNSPECIFIED.);
#585=B_SPLINE_CURVE_WITH_KNOTS('',3,(#42403,#42404,#42405,#42406,#42407,
#42408,#42409,#42410,#42411,#42412,#42413,#42414,#42415,#42416,#42417,#42418,
#42419,#42420,#42421,#42422,#42423,#42424),.UNSPECIFIED.,.F.,.F.,(4,3,3,
3,3,3,3,4),(-100.853077251014,-99.8686079559951,-98.8699218764352,-97.8712357968752,
-96.8725497173153,-95.8738636377553,-94.8751775581954,-94.5698919438346),
 .UNSPECIFIED.);
#586=B_SPLINE_CURVE_WITH_KNOTS('',3,(#42425,#42426,#42427,#42428,#42429,
#42430,#42431,#42432,#42433,#42434,#42435,#42436,#42437,#42438,#42439,#42440,
#42441,#42442,#42443,#42444,#42445,#42446,#42447,#42448,#42449),
 .UNSPECIFIED.,.F.,.F.,(4,3,3,3,3,3,3,3,4),(91.6006102298481,91.8791193195155,
92.8778053990755,93.8764914786354,94.8751775581954,95.8738636377553,96.8725497173153,
97.8712357968752,97.8837955370278),.UNSPECIFIED.);
#587=B_SPLINE_CURVE_WITH_KNOTS('',3,(#42454,#42455,#42456,#42457,#42458,
#42459,#42460,#42461,#42462,#42463,#42464,#42465,#42466,#42467,#42468,#42469,
#42470,#42471,#42472,#42473,#42474,#42475,#42476,#42477,#42478),
 .UNSPECIFIED.,.F.,.F.,(4,3,3,3,3,3,3,3,4),(-107.136262558194,-106.859410512915,
-105.860724433355,-104.862038353795,-103.863352274235,-102.864666194675,
-101.865980115115,-100.867294035555,-100.853077251014),.UNSPECIFIED.);
#588=B_SPLINE_CURVE_WITH_KNOTS('',3,(#42479,#42480,#42481,#42482,#42483,
#42484,#42485,#42486,#42487,#42488,#42489,#42490,#42491,#42492,#42493,#42494,
#42495,#42496,#42497,#42498,#42499,#42500),.UNSPECIFIED.,.F.,.F.,(4,3,3,
3,3,3,3,4),(97.8837955370278,98.8699218764352,99.8686079559951,100.867294035555,
101.865980115115,102.864666194675,103.863352274235,104.166980844207),
 .UNSPECIFIED.);
#589=B_SPLINE_CURVE_WITH_KNOTS('',3,(#42505,#42506,#42507,#42508,#42509,
#42510,#42511,#42512,#42513,#42514,#42515,#42516,#42517,#42518,#42519,#42520,
#42521,#42522,#42523,#42524,#42525,#42526),.UNSPECIFIED.,.F.,.F.,(4,3,3,
3,3,3,3,4),(-113.419447865373,-112.851526990274,-111.852840910715,-110.854154831155,
-109.855468751595,-108.856782672035,-107.858096592475,-107.136262558194),
 .UNSPECIFIED.);
#590=B_SPLINE_CURVE_WITH_KNOTS('',3,(#42527,#42528,#42529,#42530,#42531,
#42532,#42533,#42534,#42535,#42536,#42537,#42538,#42539,#42540,#42541,#42542,
#42543,#42544,#42545,#42546,#42547,#42548),.UNSPECIFIED.,.F.,.F.,(4,3,3,
3,3,3,3,4),(104.166980844207,104.862038353795,105.860724433355,106.859410512915,
107.858096592475,108.856782672035,109.855468751595,110.450166151387),
 .UNSPECIFIED.);
#591=B_SPLINE_CURVE_WITH_KNOTS('',3,(#42553,#42554,#42555,#42556,#42557,
#42558,#42559,#42560,#42561,#42562,#42563,#42564,#42565,#42566,#42567,#42568,
#42569,#42570,#42571,#42572,#42573,#42574),.UNSPECIFIED.,.F.,.F.,(4,3,3,
3,3,3,3,4),(-119.702633172553,-118.843643467634,-117.844957388074,-116.846271308514,
-115.847585228954,-114.848899149394,-113.850213069834,-113.419447865373),
 .UNSPECIFIED.);
#592=B_SPLINE_CURVE_WITH_KNOTS('',3,(#42575,#42576,#42577,#42578,#42579,
#42580,#42581,#42582,#42583,#42584,#42585,#42586,#42587,#42588,#42589,#42590,
#42591,#42592,#42593,#42594,#42595,#42596),.UNSPECIFIED.,.F.,.F.,(4,3,3,
3,3,3,3,4),(110.450166151387,110.854154831155,111.852840910715,112.851526990275,
113.850213069834,114.848899149394,115.847585228954,116.733351458567),
 .UNSPECIFIED.);
#593=B_SPLINE_CURVE_WITH_KNOTS('',3,(#42601,#42602,#42603,#42604,#42605,
#42606,#42607,#42608,#42609,#42610,#42611,#42612,#42613,#42614,#42615,#42616,
#42617,#42618,#42619,#42620,#42621,#42622,#42623,#42624,#42625),
 .UNSPECIFIED.,.F.,.F.,(4,3,3,3,3,3,3,3,4),(-125.985818479733,-125.834446024554,
-124.835759944994,-123.837073865434,-122.838387785874,-121.839701706314,
-120.841015626754,-119.842329547194,-119.702633172553),.UNSPECIFIED.);
#594=B_SPLINE_CURVE_WITH_KNOTS('',3,(#42626,#42627,#42628,#42629,#42630,
#42631,#42632,#42633,#42634,#42635,#42636,#42637,#42638,#42639,#42640,#42641,
#42642,#42643,#42644,#42645,#42646,#42647,#42648,#42649,#42650),
 .UNSPECIFIED.,.F.,.F.,(4,3,3,3,3,3,3,3,4),(116.733351458567,116.846271308514,
117.844957388074,118.843643467634,119.842329547194,120.841015626754,121.839701706314,
122.838387785874,123.016536765746),.UNSPECIFIED.);
#595=B_SPLINE_CURVE_WITH_KNOTS('',3,(#42655,#42656,#42657,#42658,#42659,
#42660,#42661,#42662,#42663,#42664,#42665,#42666,#42667,#42668,#42669,#42670,
#42671,#42672,#42673,#42674,#42675,#42676),.UNSPECIFIED.,.F.,.F.,(4,3,3,
3,3,3,3,4),(-132.269003786912,-131.826562501914,-130.827876422354,-129.829190342794,
-128.830504263234,-127.831818183674,-126.833132104114,-125.985818479733),
 .UNSPECIFIED.);
#596=B_SPLINE_CURVE_WITH_KNOTS('',3,(#42677,#42678,#42679,#42680,#42681,
#42682,#42683,#42684,#42685,#42686,#42687,#42688,#42689,#42690,#42691,#42692,
#42693,#42694,#42695,#42696,#42697,#42698),.UNSPECIFIED.,.F.,.F.,(4,3,3,
3,3,3,3,4),(123.016536765746,123.837073865434,124.835759944994,125.834446024554,
126.833132104114,127.831818183674,128.830504263234,129.299722072926),
 .UNSPECIFIED.);
#597=B_SPLINE_CURVE_WITH_KNOTS('',3,(#42703,#42704,#42705,#42706,#42707,
#42708,#42709,#42710,#42711,#42712,#42713,#42714,#42715,#42716,#42717,#42718,
#42719,#42720,#42721,#42722,#42723,#42724),.UNSPECIFIED.,.F.,.F.,(4,3,3,
3,3,3,3,4),(-138.552189094092,-137.818678979273,-136.819992899713,-135.821306820153,
-134.822620740593,-133.823934661033,-132.825248581473,-132.269003786912),
 .UNSPECIFIED.);
#598=B_SPLINE_CURVE_WITH_KNOTS('',3,(#42725,#42726,#42727,#42728,#42729,
#42730,#42731,#42732,#42733,#42734,#42735,#42736,#42737,#42738,#42739,#42740,
#42741,#42742,#42743,#42744,#42745,#42746),.UNSPECIFIED.,.F.,.F.,(4,3,3,
3,3,3,3,4),(129.299722072926,129.829190342794,130.827876422354,131.826562501914,
132.825248581474,133.823934661033,134.822620740593,135.582907380105),
 .UNSPECIFIED.);
#599=B_SPLINE_CURVE_WITH_KNOTS('',3,(#42751,#42752,#42753,#42754,#42755,
#42756,#42757,#42758,#42759,#42760,#42761,#42762,#42763,#42764,#42765,#42766,
#42767,#42768,#42769,#42770,#42771,#42772,#42773,#42774,#42775),
 .UNSPECIFIED.,.F.,.F.,(4,3,3,3,3,3,3,3,4),(-144.835374401271,-144.809481536193,
-143.810795456633,-142.812109377073,-141.813423297513,-140.814737217953,
-139.816051138393,-138.817365058833,-138.552189094092),.UNSPECIFIED.);
#600=B_SPLINE_CURVE_WITH_KNOTS('',3,(#42776,#42777,#42778,#42779,#42780,
#42781,#42782,#42783,#42784,#42785,#42786,#42787,#42788,#42789,#42790,#42791,
#42792,#42793,#42794,#42795,#42796,#42797,#42798,#42799,#42800),
 .UNSPECIFIED.,.F.,.F.,(4,3,3,3,3,3,3,3,4),(135.582907380105,135.821306820153,
136.819992899713,137.818678979273,138.817365058833,139.816051138393,140.814737217953,
141.813423297513,141.866092687285),.UNSPECIFIED.);
#601=B_SPLINE_CURVE_WITH_KNOTS('',3,(#42805,#42806,#42807,#42808,#42809,
#42810,#42811,#42812,#42813,#42814,#42815,#42816,#42817,#42818,#42819,#42820,
#42821,#42822,#42823,#42824,#42825,#42826),.UNSPECIFIED.,.F.,.F.,(4,3,3,
3,3,3,3,4),(-151.118559708451,-150.801598013553,-149.802911933993,-148.804225854433,
-147.805539774873,-146.806853695313,-145.808167615753,-144.835374401271),
 .UNSPECIFIED.);
#602=B_SPLINE_CURVE_WITH_KNOTS('',3,(#42827,#42828,#42829,#42830,#42831,
#42832,#42833,#42834,#42835,#42836,#42837,#42838,#42839,#42840,#42841,#42842,
#42843,#42844,#42845,#42846,#42847,#42848),.UNSPECIFIED.,.F.,.F.,(4,3,3,
3,3,3,3,4),(141.866092687285,142.812109377073,143.810795456633,144.809481536193,
145.808167615753,146.806853695313,147.805539774873,148.149277994464),
 .UNSPECIFIED.);
#603=B_SPLINE_CURVE_WITH_KNOTS('',3,(#42853,#42854,#42855,#42856,#42857,
#42858,#42859,#42860,#42861,#42862,#42863,#42864,#42865,#42866,#42867,#42868,
#42869,#42870,#42871,#42872,#42873,#42874),.UNSPECIFIED.,.F.,.F.,(4,3,3,
3,3,3,3,4),(-157.40174501563,-156.793714490912,-155.795028411352,-154.796342331792,
-153.797656252232,-152.798970172673,-151.800284093113,-151.118559708451),
 .UNSPECIFIED.);
#604=B_SPLINE_CURVE_WITH_KNOTS('',3,(#42875,#42876,#42877,#42878,#42879,
#42880,#42881,#42882,#42883,#42884,#42885,#42886,#42887,#42888,#42889,#42890,
#42891,#42892,#42893,#42894,#42895,#42896),.UNSPECIFIED.,.F.,.F.,(4,3,3,
3,3,3,3,4),(148.149277994464,148.804225854433,149.802911933993,150.801598013553,
151.800284093113,152.798970172673,153.797656252233,154.432463301644),
 .UNSPECIFIED.);
#605=B_SPLINE_CURVE_WITH_KNOTS('',3,(#42901,#42902,#42903,#42904,#42905,
#42906,#42907,#42908,#42909,#42910,#42911,#42912,#42913,#42914,#42915,#42916,
#42917,#42918,#42919,#42920,#42921,#42922),.UNSPECIFIED.,.F.,.F.,(4,3,3,
3,3,3,3,4),(-163.68493032281,-162.785830968272,-161.787144888712,-160.788458809152,
-159.789772729592,-158.791086650032,-157.792400570472,-157.40174501563),
 .UNSPECIFIED.);
#606=B_SPLINE_CURVE_WITH_KNOTS('',3,(#42923,#42924,#42925,#42926,#42927,
#42928,#42929,#42930,#42931,#42932,#42933,#42934,#42935,#42936,#42937,#42938,
#42939,#42940,#42941,#42942,#42943,#42944),.UNSPECIFIED.,.F.,.F.,(4,3,3,
3,3,3,3,4),(154.432463301644,154.796342331793,155.795028411352,156.793714490912,
157.792400570472,158.791086650032,159.789772729592,160.715648608824),
 .UNSPECIFIED.);
#607=B_SPLINE_CURVE_WITH_KNOTS('',3,(#42949,#42950,#42951,#42952,#42953,
#42954,#42955,#42956,#42957,#42958,#42959,#42960,#42961,#42962,#42963,#42964,
#42965,#42966,#42967,#42968,#42969,#42970,#42971,#42972,#42973),
 .UNSPECIFIED.,.F.,.F.,(4,3,3,3,3,3,3,3,4),(-169.96811562999,-169.776633525192,
-168.777947445632,-167.779261366072,-166.780575286512,-165.781889206952,
-164.783203127392,-163.784517047832,-163.68493032281),.UNSPECIFIED.);
#608=B_SPLINE_CURVE_WITH_KNOTS('',3,(#42974,#42975,#42976,#42977,#42978,
#42979,#42980,#42981,#42982,#42983,#42984,#42985,#42986,#42987,#42988,#42989,
#42990,#42991,#42992,#42993,#42994,#42995,#42996,#42997,#42998),
 .UNSPECIFIED.,.F.,.F.,(4,3,3,3,3,3,3,3,4),(160.715648608824,160.788458809152,
161.787144888712,162.785830968272,163.784517047832,164.783203127392,165.781889206952,
166.780575286512,166.998833916003),.UNSPECIFIED.);
#609=B_SPLINE_CURVE_WITH_KNOTS('',3,(#43003,#43004,#43005,#43006,#43007,
#43008,#43009,#43010,#43011,#43012,#43013,#43014,#43015,#43016,#43017,#43018,
#43019,#43020,#43021,#43022,#43023,#43024),.UNSPECIFIED.,.F.,.F.,(4,3,3,
3,3,3,3,4),(-176.251300937169,-175.768750002551,-174.770063922991,-173.771377843432,
-172.772691763872,-171.774005684312,-170.775319604752,-169.96811562999),
 .UNSPECIFIED.);
#610=B_SPLINE_CURVE_WITH_KNOTS('',3,(#43025,#43026,#43027,#43028,#43029,
#43030,#43031,#43032,#43033,#43034,#43035,#43036,#43037,#43038,#43039,#43040,
#43041,#43042,#43043,#43044,#43045,#43046),.UNSPECIFIED.,.F.,.F.,(4,3,3,
3,3,3,3,4),(166.998833916003,167.779261366072,168.777947445632,169.776633525192,
170.775319604752,171.774005684312,172.772691763872,173.282019223183),
 .UNSPECIFIED.);
#611=B_SPLINE_CURVE_WITH_KNOTS('',3,(#43051,#43052,#43053,#43054,#43055,
#43056,#43057,#43058,#43059,#43060,#43061,#43062,#43063,#43064,#43065,#43066,
#43067,#43068,#43069,#43070,#43071,#43072),.UNSPECIFIED.,.F.,.F.,(4,3,3,
3,3,3,3,4),(-182.534486244349,-181.760866479911,-180.762180400351,-179.763494320791,
-178.764808241231,-177.766122161671,-176.767436082111,-176.251300937169),
 .UNSPECIFIED.);
#612=B_SPLINE_CURVE_WITH_KNOTS('',3,(#43073,#43074,#43075,#43076,#43077,
#43078,#43079,#43080,#43081,#43082,#43083,#43084,#43085,#43086,#43087,#43088,
#43089,#43090,#43091,#43092,#43093,#43094),.UNSPECIFIED.,.F.,.F.,(4,3,3,
3,3,3,3,4),(173.282019223183,173.771377843432,174.770063922992,175.768750002551,
176.767436082111,177.766122161671,178.764808241231,179.565204530362),
 .UNSPECIFIED.);
#613=B_SPLINE_CURVE_WITH_KNOTS('',3,(#43099,#43100,#43101,#43102,#43103,
#43104,#43105,#43106,#43107,#43108,#43109,#43110,#43111,#43112,#43113,#43114,
#43115,#43116,#43117,#43118,#43119,#43120,#43121,#43122,#43123),
 .UNSPECIFIED.,.F.,.F.,(4,3,3,3,3,3,3,3,4),(-188.817671551528,-188.751669036831,
-187.752982957271,-186.754296877711,-185.755610798151,-184.756924718591,
-183.758238639031,-182.759552559471,-182.534486244349),.UNSPECIFIED.);
#614=B_SPLINE_CURVE_WITH_KNOTS('',3,(#43124,#43125,#43126,#43127,#43128,
#43129,#43130,#43131,#43132,#43133,#43134,#43135,#43136,#43137,#43138,#43139,
#43140,#43141,#43142,#43143,#43144,#43145,#43146,#43147,#43148),
 .UNSPECIFIED.,.F.,.F.,(4,3,3,3,3,3,3,3,4),(179.565204530362,179.763494320791,
180.762180400351,181.760866479911,182.759552559471,183.758238639031,184.756924718591,
185.755610798151,185.848389837542),.UNSPECIFIED.);
#615=B_SPLINE_CURVE_WITH_KNOTS('',3,(#43153,#43154,#43155,#43156,#43157,
#43158,#43159,#43160,#43161,#43162,#43163,#43164,#43165,#43166,#43167,#43168,
#43169,#43170,#43171,#43172,#43173,#43174),.UNSPECIFIED.,.F.,.F.,(4,3,3,
3,3,3,3,4),(-195.100856858708,-194.74378551419,-193.745099434631,-192.746413355071,
-191.747727275511,-190.749041195951,-189.750355116391,-188.817671551528),
 .UNSPECIFIED.);
#616=B_SPLINE_CURVE_WITH_KNOTS('',3,(#43175,#43176,#43177,#43178,#43179,
#43180,#43181,#43182,#43183,#43184,#43185,#43186,#43187,#43188,#43189,#43190,
#43191,#43192,#43193,#43194,#43195,#43196),.UNSPECIFIED.,.F.,.F.,(4,3,3,
3,3,3,3,4),(185.848389837542,186.754296877711,187.752982957271,188.751669036831,
189.750355116391,190.749041195951,191.747727275511,192.131575144721),
 .UNSPECIFIED.);
#617=B_SPLINE_CURVE_WITH_KNOTS('',3,(#43201,#43202,#43203,#43204,#43205,
#43206,#43207,#43208,#43209,#43210,#43211,#43212,#43213,#43214,#43215,#43216,
#43217,#43218,#43219,#43220,#43221,#43222),.UNSPECIFIED.,.F.,.F.,(4,3,3,
3,3,3,3,4),(-201.384042165887,-200.73590199155,-199.73721591199,-198.73852983243,
-197.73984375287,-196.74115767331,-195.74247159375,-195.100856858708),
 .UNSPECIFIED.);
#618=B_SPLINE_CURVE_WITH_KNOTS('',3,(#43223,#43224,#43225,#43226,#43227,
#43228,#43229,#43230,#43231,#43232,#43233,#43234,#43235,#43236,#43237,#43238,
#43239,#43240,#43241,#43242,#43243,#43244),.UNSPECIFIED.,.F.,.F.,(4,3,3,
3,3,3,3,4),(192.131575144721,192.746413355071,193.745099434631,194.743785514191,
195.74247159375,196.74115767331,197.73984375287,198.414760451901),
 .UNSPECIFIED.);
#619=B_SPLINE_CURVE_WITH_KNOTS('',3,(#43249,#43250,#43251,#43252,#43253,
#43254,#43255,#43256,#43257,#43258,#43259,#43260,#43261,#43262,#43263,#43264,
#43265,#43266,#43267,#43268,#43269,#43270),.UNSPECIFIED.,.F.,.F.,(4,3,3,
3,3,3,3,4),(-207.667227473067,-206.72801846891,-205.72933238935,-204.73064630979,
-203.73196023023,-202.73327415067,-201.73458807111,-201.384042165887),
 .UNSPECIFIED.);
#620=B_SPLINE_CURVE_WITH_KNOTS('',3,(#43271,#43272,#43273,#43274,#43275,
#43276,#43277,#43278,#43279,#43280,#43281,#43282,#43283,#43284,#43285,#43286,
#43287,#43288,#43289,#43290,#43291,#43292),.UNSPECIFIED.,.F.,.F.,(4,3,3,
3,3,3,3,4),(198.414760451901,198.73852983243,199.73721591199,200.73590199155,
201.73458807111,202.73327415067,203.73196023023,204.69794575908),
 .UNSPECIFIED.);
#621=B_SPLINE_CURVE_WITH_KNOTS('',3,(#43297,#43298,#43299,#43300,#43301,
#43302,#43303,#43304,#43305,#43306,#43307,#43308,#43309,#43310,#43311,#43312,
#43313,#43314,#43315,#43316,#43317,#43318,#43319,#43320,#43321),
 .UNSPECIFIED.,.F.,.F.,(4,3,3,3,3,3,3,3,4),(-213.950412780246,-213.71882102583,
-212.72013494627,-211.72144886671,-210.72276278715,-209.72407670759,-208.72539062803,
-207.72670454847,-207.667227473067),.UNSPECIFIED.);
#622=B_SPLINE_CURVE_WITH_KNOTS('',3,(#43322,#43323,#43324,#43325,#43326,
#43327,#43328,#43329,#43330,#43331,#43332,#43333,#43334,#43335,#43336,#43337,
#43338,#43339,#43340,#43341,#43342,#43343,#43344,#43345,#43346),
 .UNSPECIFIED.,.F.,.F.,(4,3,3,3,3,3,3,3,4),(204.69794575908,204.73064630979,
205.72933238935,206.72801846891,207.72670454847,208.72539062803,209.72407670759,
210.72276278715,210.98113106626),.UNSPECIFIED.);
#623=B_SPLINE_CURVE_WITH_KNOTS('',3,(#43351,#43352,#43353,#43354,#43355,
#43356,#43357,#43358,#43359,#43360,#43361,#43362,#43363,#43364,#43365,#43366,
#43367,#43368,#43369,#43370,#43371,#43372),.UNSPECIFIED.,.F.,.F.,(4,3,3,
3,3,3,3,4),(-220.233598087426,-219.710937503189,-218.712251423629,-217.713565344069,
-216.714879264509,-215.716193184949,-214.717507105389,-213.950412780246),
 .UNSPECIFIED.);
#624=B_SPLINE_CURVE_WITH_KNOTS('',3,(#43373,#43374,#43375,#43376,#43377,
#43378,#43379,#43380,#43381,#43382,#43383,#43384,#43385,#43386,#43387,#43388,
#43389,#43390,#43391,#43392,#43393,#43394),.UNSPECIFIED.,.F.,.F.,(4,3,3,
3,3,3,3,4),(210.98113106626,211.72144886671,212.72013494627,213.71882102583,
214.71750710539,215.71619318495,216.714879264509,217.26431637344),
 .UNSPECIFIED.);
#625=B_SPLINE_CURVE_WITH_KNOTS('',3,(#43399,#43400,#43401,#43402,#43403,
#43404,#43405,#43406,#43407,#43408,#43409,#43410,#43411,#43412,#43413,#43414,
#43415,#43416,#43417,#43418,#43419,#43420),.UNSPECIFIED.,.F.,.F.,(4,3,3,
3,3,3,3,4),(-226.516783394606,-225.703053980549,-224.704367900989,-223.705681821429,
-222.706995741869,-221.708309662309,-220.709623582749,-220.233598087426),
 .UNSPECIFIED.);
#626=B_SPLINE_CURVE_WITH_KNOTS('',3,(#43421,#43422,#43423,#43424,#43425,
#43426,#43427,#43428,#43429,#43430,#43431,#43432,#43433,#43434,#43435,#43436,
#43437,#43438,#43439,#43440,#43441,#43442),.UNSPECIFIED.,.F.,.F.,(4,3,3,
3,3,3,3,4),(217.26431637344,217.713565344069,218.712251423629,219.710937503189,
220.709623582749,221.708309662309,222.706995741869,223.547501680619),
 .UNSPECIFIED.);
#627=B_SPLINE_CURVE_WITH_KNOTS('',3,(#43447,#43448,#43449,#43450,#43451,
#43452,#43453,#43454,#43455,#43456,#43457,#43458,#43459,#43460,#43461,#43462,
#43463,#43464,#43465,#43466,#43467,#43468,#43469,#43470,#43471),
 .UNSPECIFIED.,.F.,.F.,(4,3,3,3,3,3,3,3,4),(-232.799968701785,-232.693856537469,
-231.695170457909,-230.696484378349,-229.697798298789,-228.699112219229,
-227.700426139669,-226.701740060109,-226.516783394606),.UNSPECIFIED.);
#628=B_SPLINE_CURVE_WITH_KNOTS('',3,(#43472,#43473,#43474,#43475,#43476,
#43477,#43478,#43479,#43480,#43481,#43482,#43483,#43484,#43485,#43486,#43487,
#43488,#43489,#43490,#43491,#43492,#43493,#43494,#43495,#43496),
 .UNSPECIFIED.,.F.,.F.,(4,3,3,3,3,3,3,3,4),(223.547501680619,223.705681821429,
224.704367900989,225.703053980549,226.701740060109,227.700426139669,228.699112219229,
229.697798298789,229.830686987799),.UNSPECIFIED.);
#629=B_SPLINE_CURVE_WITH_KNOTS('',3,(#43501,#43502,#43503,#43504,#43505,
#43506,#43507,#43508,#43509,#43510,#43511,#43512,#43513,#43514,#43515,#43516,
#43517,#43518,#43519,#43520,#43521,#43522),.UNSPECIFIED.,.F.,.F.,(4,3,3,
3,3,3,3,4),(-239.083154008965,-238.685973014828,-237.687286935268,-236.688600855708,
-235.689914776148,-234.691228696589,-233.692542617029,-232.799968701785),
 .UNSPECIFIED.);
#630=B_SPLINE_CURVE_WITH_KNOTS('',3,(#43523,#43524,#43525,#43526,#43527,
#43528,#43529,#43530,#43531,#43532,#43533,#43534,#43535,#43536,#43537,#43538,
#43539,#43540,#43541,#43542,#43543,#43544),.UNSPECIFIED.,.F.,.F.,(4,3,3,
3,3,3,3,4),(229.830686987799,230.696484378349,231.695170457909,232.693856537469,
233.692542617029,234.691228696589,235.689914776149,236.113872294978),
 .UNSPECIFIED.);
#631=B_SPLINE_CURVE_WITH_KNOTS('',3,(#43549,#43550,#43551,#43552,#43553,
#43554,#43555,#43556,#43557,#43558,#43559,#43560,#43561,#43562,#43563,#43564,
#43565,#43566,#43567,#43568,#43569,#43570),.UNSPECIFIED.,.F.,.F.,(4,3,3,
3,3,3,3,4),(-245.366339316144,-244.678089492188,-243.679403412628,-242.680717333068,
-241.682031253508,-240.683345173948,-239.684659094388,-239.083154008965),
 .UNSPECIFIED.);
#632=B_SPLINE_CURVE_WITH_KNOTS('',3,(#43571,#43572,#43573,#43574,#43575,
#43576,#43577,#43578,#43579,#43580,#43581,#43582,#43583,#43584,#43585,#43586,
#43587,#43588,#43589,#43590,#43591,#43592),.UNSPECIFIED.,.F.,.F.,(4,3,3,
3,3,3,3,4),(236.113872294978,236.688600855709,237.687286935268,238.685973014828,
239.684659094388,240.683345173948,241.682031253508,242.397057602158),
 .UNSPECIFIED.);
#633=B_SPLINE_CURVE_WITH_KNOTS('',3,(#43597,#43598,#43599,#43600,#43601,
#43602,#43603,#43604,#43605,#43606,#43607,#43608,#43609,#43610,#43611,#43612,
#43613,#43614,#43615,#43616,#43617,#43618),.UNSPECIFIED.,.F.,.F.,(4,3,3,
3,3,3,3,4),(-251.649524623324,-250.670205969548,-249.671519889988,-248.672833810428,
-247.674147730868,-246.675461651308,-245.676775571748,-245.366339316144),
 .UNSPECIFIED.);
#634=B_SPLINE_CURVE_WITH_KNOTS('',3,(#43619,#43620,#43621,#43622,#43623,
#43624,#43625,#43626,#43627,#43628,#43629,#43630,#43631,#43632,#43633,#43634,
#43635,#43636,#43637,#43638,#43639,#43640,#43641,#43642,#43643),
 .UNSPECIFIED.,.F.,.F.,(4,3,3,3,3,3,3,3,4),(242.397057602158,242.680717333068,
243.679403412628,244.678089492188,245.676775571748,246.675461651308,247.674147730868,
248.672833810428,248.680242909337),.UNSPECIFIED.);
#635=B_SPLINE_CURVE_WITH_KNOTS('',3,(#43648,#43649,#43650,#43651,#43652,
#43653,#43654,#43655,#43656,#43657,#43658,#43659,#43660,#43661,#43662,#43663,
#43664,#43665,#43666,#43667,#43668,#43669,#43670,#43671,#43672),
 .UNSPECIFIED.,.F.,.F.,(4,3,3,3,3,3,3,3,4),(-257.932709930503,-257.661008526467,
-256.662322446907,-255.663636367347,-254.664950287788,-253.666264208228,
-252.667578128668,-251.668892049108,-251.649524623324),.UNSPECIFIED.);
#636=B_SPLINE_CURVE_WITH_KNOTS('',3,(#43673,#43674,#43675,#43676,#43677,
#43678,#43679,#43680,#43681,#43682,#43683,#43684,#43685,#43686,#43687,#43688,
#43689,#43690,#43691,#43692,#43693,#43694),.UNSPECIFIED.,.F.,.F.,(4,3,3,
3,3,3,3,4),(248.680242909337,249.671519889988,250.670205969548,251.668892049108,
252.667578128668,253.666264208228,254.664950287788,254.963428216517),
 .UNSPECIFIED.);
#637=B_SPLINE_CURVE_WITH_KNOTS('',3,(#43699,#43700,#43701,#43702,#43703,
#43704,#43705,#43706,#43707,#43708,#43709,#43710,#43711,#43712,#43713,#43714,
#43715,#43716,#43717,#43718,#43719,#43720),.UNSPECIFIED.,.F.,.F.,(4,3,3,
3,3,3,3,4),(-264.215895237683,-263.653125003827,-262.654438924267,-261.655752844707,
-260.657066765147,-259.658380685587,-258.659694606027,-257.932709930503),
 .UNSPECIFIED.);
#638=B_SPLINE_CURVE_WITH_KNOTS('',3,(#43721,#43722,#43723,#43724,#43725,
#43726,#43727,#43728,#43729,#43730,#43731,#43732,#43733,#43734,#43735,#43736,
#43737,#43738,#43739,#43740,#43741,#43742),.UNSPECIFIED.,.F.,.F.,(4,3,3,
3,3,3,3,4),(254.963428216517,255.663636367348,256.662322446908,257.661008526468,
258.659694606027,259.658380685587,260.657066765147,261.246613523697),
 .UNSPECIFIED.);
#639=B_SPLINE_CURVE_WITH_KNOTS('',3,(#43747,#43748,#43749,#43750,#43751,
#43752,#43753,#43754,#43755,#43756,#43757,#43758,#43759,#43760,#43761,#43762,
#43763,#43764,#43765,#43766,#43767,#43768),.UNSPECIFIED.,.F.,.F.,(4,3,3,
3,3,3,3,4),(-270.499080544863,-269.645241481187,-268.646555401627,-267.647869322067,
-266.649183242507,-265.650497162947,-264.651811083387,-264.215895237683),
 .UNSPECIFIED.);
#640=B_SPLINE_CURVE_WITH_KNOTS('',3,(#43769,#43770,#43771,#43772,#43773,
#43774,#43775,#43776,#43777,#43778,#43779,#43780,#43781,#43782,#43783,#43784,
#43785,#43786,#43787,#43788,#43789,#43790),.UNSPECIFIED.,.F.,.F.,(4,3,3,
3,3,3,3,4),(261.246613523697,261.655752844707,262.654438924267,263.653125003827,
264.651811083387,265.650497162947,266.649183242507,267.529798830876),
 .UNSPECIFIED.);
#641=B_SPLINE_CURVE_WITH_KNOTS('',3,(#43795,#43796,#43797,#43798,#43799,
#43800,#43801,#43802,#43803,#43804,#43805,#43806,#43807,#43808,#43809,#43810,
#43811,#43812,#43813,#43814,#43815,#43816,#43817,#43818,#43819),
 .UNSPECIFIED.,.F.,.F.,(4,3,3,3,3,3,3,3,4),(-276.782265852042,-276.636044038106,
-275.637357958546,-274.638671878987,-273.639985799427,-272.641299719867,
-271.642613640307,-270.643927560747,-270.499080544863),.UNSPECIFIED.);
#642=B_SPLINE_CURVE_WITH_KNOTS('',3,(#43820,#43821,#43822,#43823,#43824,
#43825,#43826,#43827,#43828,#43829,#43830,#43831,#43832,#43833,#43834,#43835,
#43836,#43837,#43838,#43839,#43840,#43841,#43842,#43843,#43844),
 .UNSPECIFIED.,.F.,.F.,(4,3,3,3,3,3,3,3,4),(267.529798830876,267.647869322067,
268.646555401627,269.645241481187,270.643927560747,271.642613640307,272.641299719867,
273.639985799427,273.812984138056),.UNSPECIFIED.);
#643=B_SPLINE_CURVE_WITH_KNOTS('',3,(#43849,#43850,#43851,#43852,#43853,
#43854,#43855,#43856,#43857,#43858,#43859,#43860,#43861,#43862,#43863,#43864,
#43865,#43866,#43867,#43868,#43869,#43870),.UNSPECIFIED.,.F.,.F.,(4,3,3,
3,3,3,3,4),(-283.065451159222,-282.628160515466,-281.629474435906,-280.630788356346,
-279.632102276786,-278.633416197226,-277.634730117666,-276.782265852042),
 .UNSPECIFIED.);
#644=B_SPLINE_CURVE_WITH_KNOTS('',3,(#43871,#43872,#43873,#43874,#43875,
#43876,#43877,#43878,#43879,#43880,#43881,#43882,#43883,#43884,#43885,#43886,
#43887,#43888,#43889,#43890,#43891,#43892),.UNSPECIFIED.,.F.,.F.,(4,3,3,
3,3,3,3,4),(273.812984138056,274.638671878987,275.637357958547,276.636044038107,
277.634730117666,278.633416197226,279.632102276786,280.096169445235),
 .UNSPECIFIED.);
#645=B_SPLINE_CURVE_WITH_KNOTS('',3,(#43897,#43898,#43899,#43900,#43901,
#43902,#43903,#43904,#43905,#43906,#43907,#43908,#43909,#43910,#43911,#43912,
#43913,#43914,#43915,#43916,#43917,#43918),.UNSPECIFIED.,.F.,.F.,(4,3,3,
3,3,3,3,4),(-289.348636466401,-288.620276992826,-287.621590913266,-286.622904833706,
-285.624218754146,-284.625532674586,-283.626846595026,-283.065451159222),
 .UNSPECIFIED.);
#646=B_SPLINE_CURVE_WITH_KNOTS('',3,(#43919,#43920,#43921,#43922,#43923,
#43924,#43925,#43926,#43927,#43928,#43929,#43930,#43931,#43932,#43933,#43934,
#43935,#43936,#43937,#43938,#43939,#43940),.UNSPECIFIED.,.F.,.F.,(4,3,3,
3,3,3,3,4),(280.096169445235,280.630788356346,281.629474435906,282.628160515466,
283.626846595026,284.625532674586,285.624218754146,286.379354752415),
 .UNSPECIFIED.);
#647=B_SPLINE_CURVE_WITH_KNOTS('',3,(#43945,#43946,#43947,#43948,#43949,
#43950,#43951,#43952,#43953,#43954,#43955,#43956,#43957,#43958,#43959,#43960,
#43961,#43962,#43963,#43964,#43965,#43966,#43967,#43968,#43969),
 .UNSPECIFIED.,.F.,.F.,(4,3,3,3,3,3,3,3,4),(-295.631821773581,-295.611079549746,
-294.612393470186,-293.613707390626,-292.615021311066,-291.616335231506,
-290.617649151946,-289.618963072386,-289.348636466401),.UNSPECIFIED.);
#648=B_SPLINE_CURVE_WITH_KNOTS('',3,(#43970,#43971,#43972,#43973,#43974,
#43975,#43976,#43977,#43978,#43979,#43980,#43981,#43982,#43983,#43984,#43985,
#43986,#43987,#43988,#43989,#43990,#43991,#43992,#43993,#43994),
 .UNSPECIFIED.,.F.,.F.,(4,3,3,3,3,3,3,3,4),(286.379354752415,286.622904833706,
287.621590913266,288.620276992826,289.618963072386,290.617649151946,291.616335231506,
292.615021311066,292.662540059594),.UNSPECIFIED.);
#649=B_SPLINE_CURVE_WITH_KNOTS('',3,(#43999,#44000,#44001,#44002,#44003,
#44004,#44005,#44006,#44007,#44008,#44009,#44010,#44011,#44012,#44013,#44014,
#44015,#44016,#44017,#44018,#44019,#44020),.UNSPECIFIED.,.F.,.F.,(4,3,3,
3,3,3,3,4),(-301.91500708076,-301.603196027105,-300.604509947545,-299.605823867985,
-298.607137788425,-297.608451708865,-296.609765629305,-295.631821773581),
 .UNSPECIFIED.);
#650=B_SPLINE_CURVE_WITH_KNOTS('',3,(#44021,#44022,#44023,#44024,#44025,
#44026,#44027,#44028,#44029,#44030,#44031,#44032,#44033,#44034,#44035,#44036,
#44037,#44038,#44039,#44040,#44041,#44042),.UNSPECIFIED.,.F.,.F.,(4,3,3,
3,3,3,3,4),(292.662540059594,293.613707390626,294.612393470186,295.611079549746,
296.609765629306,297.608451708865,298.607137788425,298.945725366774),
 .UNSPECIFIED.);
#651=B_SPLINE_CURVE_WITH_KNOTS('',3,(#44047,#44048,#44049,#44050,#44051,
#44052,#44053,#44054,#44055,#44056,#44057,#44058,#44059,#44060,#44061,#44062,
#44063,#44064,#44065,#44066,#44067,#44068),.UNSPECIFIED.,.F.,.F.,(4,3,3,
3,3,3,3,4),(-308.19819238794,-307.595312504465,-306.596626424905,-305.597940345345,
-304.599254265785,-303.600568186225,-302.601882106665,-301.91500708076),
 .UNSPECIFIED.);
#652=B_SPLINE_CURVE_WITH_KNOTS('',3,(#44069,#44070,#44071,#44072,#44073,
#44074,#44075,#44076,#44077,#44078,#44079,#44080,#44081,#44082,#44083,#44084,
#44085,#44086,#44087,#44088,#44089,#44090),.UNSPECIFIED.,.F.,.F.,(4,3,3,
3,3,3,3,4),(298.945725366774,299.605823867985,300.604509947545,301.603196027105,
302.601882106665,303.600568186225,304.599254265785,305.228910673953),
 .UNSPECIFIED.);
#653=B_SPLINE_CURVE_WITH_KNOTS('',3,(#44095,#44096,#44097,#44098,#44099,
#44100,#44101,#44102,#44103,#44104,#44105,#44106,#44107,#44108,#44109,#44110,
#44111,#44112,#44113,#44114,#44115,#44116),.UNSPECIFIED.,.F.,.F.,(4,3,3,
3,3,3,3,4),(-314.481377695119,-313.587428981825,-312.588742902265,-311.590056822705,
-310.591370743145,-309.592684663585,-308.593998584025,-308.19819238794),
 .UNSPECIFIED.);
#654=B_SPLINE_CURVE_WITH_KNOTS('',3,(#44117,#44118,#44119,#44120,#44121,
#44122,#44123,#44124,#44125,#44126,#44127,#44128,#44129,#44130,#44131,#44132,
#44133,#44134,#44135,#44136,#44137,#44138),.UNSPECIFIED.,.F.,.F.,(4,3,3,
3,3,3,3,4),(305.228910673953,305.597940345345,306.596626424905,307.595312504465,
308.593998584025,309.592684663585,310.591370743145,311.512095981133),
 .UNSPECIFIED.);
#655=B_SPLINE_CURVE_WITH_KNOTS('',3,(#44143,#44144,#44145,#44146,#44147,
#44148,#44149,#44150,#44151,#44152,#44153,#44154,#44155,#44156,#44157,#44158,
#44159,#44160,#44161,#44162,#44163,#44164,#44165,#44166,#44167),
 .UNSPECIFIED.,.F.,.F.,(4,3,3,3,3,3,3,3,4),(-320.764563002299,-320.578231538744,
-319.579545459184,-318.580859379624,-317.582173300064,-316.583487220505,
-315.584801140945,-314.586115061385,-314.481377695119),.UNSPECIFIED.);
#656=B_SPLINE_CURVE_WITH_KNOTS('',3,(#44168,#44169,#44170,#44171,#44172,
#44173,#44174,#44175,#44176,#44177,#44178,#44179,#44180,#44181,#44182,#44183,
#44184,#44185,#44186,#44187,#44188,#44189,#44190,#44191,#44192),
 .UNSPECIFIED.,.F.,.F.,(4,3,3,3,3,3,3,3,4),(311.512095981133,311.590056822705,
312.588742902265,313.587428981825,314.586115061385,315.584801140945,316.583487220505,
317.582173300065,317.795281288313),.UNSPECIFIED.);
#657=B_SPLINE_CURVE_WITH_KNOTS('',3,(#44197,#44198,#44199,#44200,#44201,
#44202,#44203,#44204,#44205,#44206,#44207,#44208,#44209,#44210,#44211,#44212,
#44213,#44214,#44215,#44216,#44217,#44218),.UNSPECIFIED.,.F.,.F.,(4,3,3,
3,3,3,3,4),(-327.047748309479,-326.570348016104,-325.571661936544,-324.572975856984,
-323.574289777424,-322.575603697864,-321.576917618304,-320.764563002299),
 .UNSPECIFIED.);
#658=B_SPLINE_CURVE_WITH_KNOTS('',3,(#44219,#44220,#44221,#44222,#44223,
#44224,#44225,#44226,#44227,#44228,#44229,#44230,#44231,#44232,#44233,#44234,
#44235,#44236,#44237,#44238,#44239,#44240),.UNSPECIFIED.,.F.,.F.,(4,3,3,
3,3,3,3,4),(317.795281288313,318.580859379625,319.579545459185,320.578231538744,
321.576917618304,322.575603697864,323.574289777424,324.078466595492),
 .UNSPECIFIED.);
#659=B_SPLINE_CURVE_WITH_KNOTS('',3,(#44245,#44246,#44247,#44248,#44249,
#44250,#44251,#44252,#44253,#44254,#44255,#44256,#44257,#44258,#44259,#44260,
#44261,#44262,#44263,#44264,#44265,#44266),.UNSPECIFIED.,.F.,.F.,(4,3,3,
3,3,3,3,4),(-333.330933616658,-332.562464493464,-331.563778413904,-330.565092334344,
-329.566406254784,-328.567720175224,-327.569034095664,-327.047748309479),
 .UNSPECIFIED.);
#660=B_SPLINE_CURVE_WITH_KNOTS('',3,(#44267,#44268,#44269,#44270,#44271,
#44272,#44273,#44274,#44275,#44276,#44277,#44278,#44279,#44280,#44281,#44282,
#44283,#44284,#44285,#44286,#44287,#44288),.UNSPECIFIED.,.F.,.F.,(4,3,3,
3,3,3,3,4),(324.078466595492,324.572975856984,325.571661936544,326.570348016104,
327.569034095664,328.567720175224,329.566406254784,330.361651902672),
 .UNSPECIFIED.);
#661=B_SPLINE_CURVE_WITH_KNOTS('',3,(#44293,#44294,#44295,#44296,#44297,
#44298,#44299,#44300,#44301,#44302,#44303,#44304,#44305,#44306,#44307,#44308,
#44309,#44310,#44311,#44312,#44313,#44314,#44315,#44316,#44317),
 .UNSPECIFIED.,.F.,.F.,(4,3,3,3,3,3,3,3,4),(-339.614118923838,-339.553267050383,
-338.554580970823,-337.555894891264,-336.557208811704,-335.558522732144,
-334.559836652584,-333.561150573024,-333.330933616658),.UNSPECIFIED.);
#662=B_SPLINE_CURVE_WITH_KNOTS('',3,(#44318,#44319,#44320,#44321,#44322,
#44323,#44324,#44325,#44326,#44327,#44328,#44329,#44330,#44331,#44332,#44333,
#44334,#44335,#44336,#44337,#44338,#44339,#44340,#44341,#44342),
 .UNSPECIFIED.,.F.,.F.,(4,3,3,3,3,3,3,3,4),(330.361651902672,330.565092334344,
331.563778413904,332.562464493464,333.561150573024,334.559836652584,335.558522732144,
336.557208811704,336.644837209851),.UNSPECIFIED.);
#663=B_SPLINE_CURVE_WITH_KNOTS('',3,(#44347,#44348,#44349,#44350,#44351,
#44352,#44353,#44354,#44355,#44356,#44357,#44358,#44359,#44360,#44361,#44362,
#44363,#44364,#44365,#44366,#44367,#44368),.UNSPECIFIED.,.F.,.F.,(4,3,3,
3,3,3,3,4),(-345.897304231017,-345.545383527743,-344.546697448183,-343.548011368623,
-342.549325289063,-341.550639209503,-340.551953129943,-339.614118923838),
 .UNSPECIFIED.);
#664=B_SPLINE_CURVE_WITH_KNOTS('',3,(#44369,#44370,#44371,#44372,#44373,
#44374,#44375,#44376,#44377,#44378,#44379,#44380,#44381,#44382,#44383,#44384,
#44385,#44386,#44387,#44388,#44389,#44390),.UNSPECIFIED.,.F.,.F.,(4,3,3,
3,3,3,3,4),(336.644837209851,337.555894891264,338.554580970824,339.553267050384,
340.551953129944,341.550639209503,342.549325289063,342.928022517031),
 .UNSPECIFIED.);
#665=B_SPLINE_CURVE_WITH_KNOTS('',3,(#44395,#44396,#44397,#44398,#44399,
#44400,#44401,#44402,#44403,#44404,#44405,#44406,#44407,#44408,#44409,#44410,
#44411,#44412,#44413,#44414,#44415,#44416),.UNSPECIFIED.,.F.,.F.,(4,3,3,
3,3,3,3,4),(-352.180489538197,-351.537500005103,-350.538813925543,-349.540127845983,
-348.541441766423,-347.542755686863,-346.544069607303,-345.897304231017),
 .UNSPECIFIED.);
#666=B_SPLINE_CURVE_WITH_KNOTS('',3,(#44417,#44418,#44419,#44420,#44421,
#44422,#44423,#44424,#44425,#44426,#44427,#44428,#44429,#44430,#44431,#44432,
#44433,#44434,#44435,#44436,#44437,#44438),.UNSPECIFIED.,.F.,.F.,(4,3,3,
3,3,3,3,4),(342.928022517031,343.548011368623,344.546697448183,345.545383527743,
346.544069607303,347.542755686863,348.541441766423,349.21120782421),
 .UNSPECIFIED.);
#667=B_SPLINE_CURVE_WITH_KNOTS('',3,(#44443,#44444,#44445,#44446,#44447,
#44448,#44449,#44450,#44451,#44452,#44453,#44454,#44455,#44456,#44457,#44458,
#44459,#44460,#44461,#44462,#44463,#44464),.UNSPECIFIED.,.F.,.F.,(4,3,3,
3,3,3,3,4),(-358.463674845376,-357.529616482463,-356.530930402903,-355.532244323343,
-354.533558243783,-353.534872164223,-352.536186084663,-352.180489538197),
 .UNSPECIFIED.);
#668=B_SPLINE_CURVE_WITH_KNOTS('',3,(#44465,#44466,#44467,#44468,#44469,
#44470,#44471,#44472,#44473,#44474,#44475,#44476,#44477,#44478,#44479,#44480,
#44481,#44482,#44483,#44484,#44485,#44486),.UNSPECIFIED.,.F.,.F.,(4,3,3,
3,3,3,3,4),(349.21120782421,349.540127845983,350.538813925543,351.537500005103,
352.536186084663,353.534872164223,354.533558243783,355.49439313139),
 .UNSPECIFIED.);
#669=B_SPLINE_CURVE_WITH_KNOTS('',3,(#44491,#44492,#44493,#44494,#44495,
#44496,#44497,#44498,#44499,#44500,#44501,#44502,#44503,#44504,#44505,#44506,
#44507,#44508,#44509,#44510,#44511,#44512,#44513,#44514,#44515),
 .UNSPECIFIED.,.F.,.F.,(4,3,3,3,3,3,3,3,4),(-364.746860152556,-364.520419039382,
-363.521732959822,-362.523046880262,-361.524360800702,-360.525674721142,
-359.526988641582,-358.528302562022,-358.463674845376),.UNSPECIFIED.);
#670=B_SPLINE_CURVE_WITH_KNOTS('',3,(#44516,#44517,#44518,#44519,#44520,
#44521,#44522,#44523,#44524,#44525,#44526,#44527,#44528,#44529,#44530,#44531,
#44532,#44533,#44534,#44535,#44536,#44537,#44538,#44539,#44540),
 .UNSPECIFIED.,.F.,.F.,(4,3,3,3,3,3,3,3,4),(355.49439313139,355.532244323343,
356.530930402903,357.529616482463,358.528302562023,359.526988641583,360.525674721143,
361.524360800702,361.77757843857),.UNSPECIFIED.);
#671=B_SPLINE_CURVE_WITH_KNOTS('',3,(#44546,#44547,#44548,#44549,#44550,
#44551),.UNSPECIFIED.,.F.,.F.,(4,1,1,4),(380.132711084365,380.904956050751,
381.903642130311,382.826527695671),.UNSPECIFIED.);
#672=B_SPLINE_CURVE_WITH_KNOTS('',3,(#44554,#44555,#44556,#44557,#44558),
 .UNSPECIFIED.,.F.,.F.,(4,1,4),(380.132711084365,380.587110696239,381.585796775799),
 .UNSPECIFIED.);
#673=B_SPLINE_CURVE_WITH_KNOTS('',3,(#44563,#44564,#44565,#44566,#44567,
#44568,#44569,#44570,#44571,#44572,#44573),.UNSPECIFIED.,.F.,.F.,(4,1,1,
1,1,1,1,1,4),(373.849525777185,373.914153493831,374.912839573391,375.911525652951,
376.910211732511,377.908897812071,378.907583891631,379.906269971191,380.132711084365),
 .UNSPECIFIED.);
#674=B_SPLINE_CURVE_WITH_KNOTS('',3,(#44574,#44575,#44576,#44577,#44578,
#44579,#44580,#44581,#44582,#44583),.UNSPECIFIED.,.F.,.F.,(4,1,1,1,1,1,
1,4),(373.849525777185,374.594994218879,375.593680298439,376.592366377999,
377.591052457559,378.589738537119,379.588424616679,380.132711084365),
 .UNSPECIFIED.);
#675=B_SPLINE_CURVE_WITH_KNOTS('',3,(#44588,#44589,#44590,#44591,#44592,
#44593,#44594,#44595,#44596,#44597),.UNSPECIFIED.,.F.,.F.,(4,1,1,1,1,1,
1,4),(367.566340470006,367.922037016472,368.920723096032,369.919409175592,
370.918095255152,371.916781334712,372.915467414271,373.849525777185),
 .UNSPECIFIED.);
#676=B_SPLINE_CURVE_WITH_KNOTS('',3,(#44598,#44599,#44600,#44601,#44602,
#44603,#44604,#44605,#44606,#44607,#44608),.UNSPECIFIED.,.F.,.F.,(4,1,1,
1,1,1,1,1,4),(367.566340470006,367.60419166196,368.602877741519,369.601563821079,
370.600249900639,371.598935980199,372.597622059759,373.596308139319,373.849525777185),
 .UNSPECIFIED.);
#677=B_SPLINE_CURVE_WITH_KNOTS('',3,(#44613,#44614,#44615,#44616,#44617,
#44618,#44619,#44620,#44621,#44622),.UNSPECIFIED.,.F.,.F.,(4,1,1,1,1,1,
1,4),(361.283155162826,361.929920539112,362.928606618672,363.927292698232,
364.925978777792,365.924664857352,366.923350936912,367.566340470006),
 .UNSPECIFIED.);
#678=B_SPLINE_CURVE_WITH_KNOTS('',3,(#44623,#44624,#44625,#44626,#44627,
#44628,#44629,#44630,#44631,#44632),.UNSPECIFIED.,.F.,.F.,(4,1,1,1,1,1,
1,4),(361.283155162826,361.6120751846,362.61076126416,363.60944734372,364.60813342328,
365.60681950284,366.6055055824,367.566340470006),.UNSPECIFIED.);
#679=B_SPLINE_CURVE_WITH_KNOTS('',3,(#44637,#44638,#44639,#44640,#44641,
#44642,#44643,#44644,#44645,#44646),.UNSPECIFIED.,.F.,.F.,(4,1,1,1,1,1,
1,4),(354.999969855647,355.937804061752,356.936490141312,357.935176220872,
358.933862300432,359.932548379992,360.931234459552,361.283155162826),
 .UNSPECIFIED.);
#680=B_SPLINE_CURVE_WITH_KNOTS('',3,(#44647,#44648,#44649,#44650,#44651,
#44652,#44653,#44654,#44655,#44656),.UNSPECIFIED.,.F.,.F.,(4,1,1,1,1,1,
1,4),(354.999969855647,355.61995870724,356.6186447868,357.61733086636,358.61601694592,
359.61470302548,360.61338910504,361.283155162826),.UNSPECIFIED.);
#681=B_SPLINE_CURVE_WITH_KNOTS('',3,(#44661,#44662,#44663,#44664,#44665,
#44666,#44667,#44668,#44669,#44670,#44671),.UNSPECIFIED.,.F.,.F.,(4,1,1,
1,1,1,1,1,4),(348.716784548467,348.947001504833,349.945687584393,350.944373663953,
351.943059743512,352.941745823072,353.940431902632,354.939117982192,354.999969855647),
 .UNSPECIFIED.);
#682=B_SPLINE_CURVE_WITH_KNOTS('',3,(#44672,#44673,#44674,#44675,#44676,
#44677,#44678,#44679,#44680,#44681),.UNSPECIFIED.,.F.,.F.,(4,1,1,1,1,1,
1,4),(348.716784548467,349.62784222988,350.62652830944,351.625214389,352.62390046856,
353.62258654812,354.62127262768,354.999969855647),.UNSPECIFIED.);
#683=B_SPLINE_CURVE_WITH_KNOTS('',3,(#44686,#44687,#44688,#44689,#44690,
#44691,#44692,#44693,#44694,#44695),.UNSPECIFIED.,.F.,.F.,(4,1,1,1,1,1,
1,4),(342.433599241287,342.954885027473,343.953571107033,344.952257186593,
345.950943266153,346.949629345713,347.948315425273,348.716784548467),
 .UNSPECIFIED.);
#684=B_SPLINE_CURVE_WITH_KNOTS('',3,(#44696,#44697,#44698,#44699,#44700,
#44701,#44702,#44703,#44704,#44705,#44706),.UNSPECIFIED.,.F.,.F.,(4,1,1,
1,1,1,1,1,4),(342.433599241288,342.637039672961,343.635725752521,344.634411832081,
345.633097911641,346.631783991201,347.63047007076,348.62915615032,348.716784548467),
 .UNSPECIFIED.);
#685=B_SPLINE_CURVE_WITH_KNOTS('',3,(#44711,#44712,#44713,#44714,#44715,
#44716,#44717,#44718,#44719,#44720),.UNSPECIFIED.,.F.,.F.,(4,1,1,1,1,1,
1,4),(336.150413934108,336.962768550113,337.961454629673,338.960140709233,
339.958826788793,340.957512868353,341.956198947913,342.433599241287),
 .UNSPECIFIED.);
#686=B_SPLINE_CURVE_WITH_KNOTS('',3,(#44721,#44722,#44723,#44724,#44725,
#44726,#44727,#44728,#44729,#44730),.UNSPECIFIED.,.F.,.F.,(4,1,1,1,1,1,
1,4),(336.150413934108,336.644923195601,337.643609275161,338.642295354721,
339.640981434281,340.639667513841,341.638353593401,342.433599241288),
 .UNSPECIFIED.);
#687=B_SPLINE_CURVE_WITH_KNOTS('',3,(#44735,#44736,#44737,#44738,#44739,
#44740,#44741,#44742,#44743,#44744,#44745),.UNSPECIFIED.,.F.,.F.,(4,1,1,
1,1,1,1,1,4),(329.867228626928,329.971965993194,330.970652072754,331.969338152313,
332.968024231873,333.966710311433,334.965396390993,335.964082470553,336.150413934108),
 .UNSPECIFIED.);
#688=B_SPLINE_CURVE_WITH_KNOTS('',3,(#44746,#44747,#44748,#44749,#44750,
#44751,#44752,#44753,#44754,#44755),.UNSPECIFIED.,.F.,.F.,(4,1,1,1,1,1,
1,4),(329.867228626928,330.652806718241,331.651492797801,332.650178877361,
333.648864956921,334.647551036481,335.646237116041,336.150413934108),
 .UNSPECIFIED.);
#689=B_SPLINE_CURVE_WITH_KNOTS('',3,(#44760,#44761,#44762,#44763,#44764,
#44765,#44766,#44767,#44768,#44769),.UNSPECIFIED.,.F.,.F.,(4,1,1,1,1,1,
1,4),(323.584043319749,323.979849515834,324.978535595394,325.977221674954,
326.975907754514,327.974593834074,328.973279913634,329.867228626928),
 .UNSPECIFIED.);
#690=B_SPLINE_CURVE_WITH_KNOTS('',3,(#44770,#44771,#44772,#44773,#44774,
#44775,#44776,#44777,#44778,#44779,#44780),.UNSPECIFIED.,.F.,.F.,(4,1,1,
1,1,1,1,1,4),(323.584043319749,323.662004161322,324.660690240882,325.659376320442,
326.658062400001,327.656748479561,328.655434559121,329.654120638681,329.867228626928),
 .UNSPECIFIED.);
#691=B_SPLINE_CURVE_WITH_KNOTS('',3,(#44785,#44786,#44787,#44788,#44789,
#44790,#44791,#44792,#44793,#44794),.UNSPECIFIED.,.F.,.F.,(4,1,1,1,1,1,
1,4),(317.300858012569,317.987733038474,318.986419118034,319.985105197594,
320.983791277154,321.982477356714,322.981163436274,323.584043319749),
 .UNSPECIFIED.);
#692=B_SPLINE_CURVE_WITH_KNOTS('',3,(#44795,#44796,#44797,#44798,#44799,
#44800,#44801,#44802,#44803,#44804),.UNSPECIFIED.,.F.,.F.,(4,1,1,1,1,1,
1,4),(317.300858012569,317.669887683962,318.668573763522,319.667259843082,
320.665945922642,321.664632002202,322.663318081762,323.584043319749),
 .UNSPECIFIED.);
#693=B_SPLINE_CURVE_WITH_KNOTS('',3,(#44809,#44810,#44811,#44812,#44813,
#44814,#44815,#44816,#44817,#44818),.UNSPECIFIED.,.F.,.F.,(4,1,1,1,1,1,
1,4),(311.01767270539,311.995616561114,312.994302640674,313.992988720234,
314.991674799794,315.990360879354,316.989046958914,317.300858012569),
 .UNSPECIFIED.);
#694=B_SPLINE_CURVE_WITH_KNOTS('',3,(#44819,#44820,#44821,#44822,#44823,
#44824,#44825,#44826,#44827,#44828),.UNSPECIFIED.,.F.,.F.,(4,1,1,1,1,1,
1,4),(311.01767270539,311.677771206602,312.676457286162,313.675143365722,
314.673829445282,315.672515524842,316.671201604402,317.300858012569),
 .UNSPECIFIED.);
#695=B_SPLINE_CURVE_WITH_KNOTS('',3,(#44833,#44834,#44835,#44836,#44837,
#44838,#44839,#44840,#44841,#44842,#44843),.UNSPECIFIED.,.F.,.F.,(4,1,1,
1,1,1,1,1,4),(304.73448739821,305.004814004195,306.003500083755,307.002186163315,
308.000872242875,308.999558322435,309.998244401995,310.996930481555,311.01767270539),
 .UNSPECIFIED.);
#696=B_SPLINE_CURVE_WITH_KNOTS('',3,(#44844,#44845,#44846,#44847,#44848,
#44849,#44850,#44851,#44852,#44853),.UNSPECIFIED.,.F.,.F.,(4,1,1,1,1,1,
1,4),(304.73448739821,305.685654729243,306.684340808802,307.683026888362,
308.681712967922,309.680399047482,310.679085127042,311.01767270539),
 .UNSPECIFIED.);
#697=B_SPLINE_CURVE_WITH_KNOTS('',3,(#44858,#44859,#44860,#44861,#44862,
#44863,#44864,#44865,#44866,#44867),.UNSPECIFIED.,.F.,.F.,(4,1,1,1,1,1,
1,4),(298.45130209103,299.012697526835,300.011383606395,301.010069685955,
302.008755765515,303.007441845075,304.006127924635,304.73448739821),
 .UNSPECIFIED.);
#698=B_SPLINE_CURVE_WITH_KNOTS('',3,(#44868,#44869,#44870,#44871,#44872,
#44873,#44874,#44875,#44876,#44877,#44878),.UNSPECIFIED.,.F.,.F.,(4,1,1,
1,1,1,1,1,4),(298.451302091031,298.694852172323,299.693538251883,300.692224331443,
301.690910411003,302.689596490563,303.688282570123,304.686968649683,304.73448739821),
 .UNSPECIFIED.);
#699=B_SPLINE_CURVE_WITH_KNOTS('',3,(#44883,#44884,#44885,#44886,#44887,
#44888,#44889,#44890,#44891,#44892),.UNSPECIFIED.,.F.,.F.,(4,1,1,1,1,1,
1,4),(292.168116783851,293.020581049475,294.019267129035,295.017953208595,
296.016639288155,297.015325367715,298.014011447275,298.45130209103),
 .UNSPECIFIED.);
#700=B_SPLINE_CURVE_WITH_KNOTS('',3,(#44893,#44894,#44895,#44896,#44897,
#44898,#44899,#44900,#44901,#44902),.UNSPECIFIED.,.F.,.F.,(4,1,1,1,1,1,
1,4),(292.168116783851,292.702735694963,293.701421774523,294.700107854083,
295.698793933643,296.697480013203,297.696166092763,298.451302091031),
 .UNSPECIFIED.);
#701=B_SPLINE_CURVE_WITH_KNOTS('',3,(#44907,#44908,#44909,#44910,#44911,
#44912,#44913,#44914,#44915,#44916,#44917),.UNSPECIFIED.,.F.,.F.,(4,1,1,
1,1,1,1,1,4),(285.884931476671,286.029778492556,287.028464572116,288.027150651676,
289.025836731236,290.024522810796,291.023208890355,292.021894969915,292.168116783851),
 .UNSPECIFIED.);
#702=B_SPLINE_CURVE_WITH_KNOTS('',3,(#44918,#44919,#44920,#44921,#44922,
#44923,#44924,#44925,#44926,#44927),.UNSPECIFIED.,.F.,.F.,(4,1,1,1,1,1,
1,4),(285.884931476671,286.710619217603,287.709305297163,288.707991376723,
289.706677456283,290.705363535843,291.704049615403,292.168116783851),
 .UNSPECIFIED.);
#703=B_SPLINE_CURVE_WITH_KNOTS('',3,(#44932,#44933,#44934,#44935,#44936,
#44937,#44938,#44939,#44940,#44941),.UNSPECIFIED.,.F.,.F.,(4,1,1,1,1,1,
1,4),(279.601746169492,280.037662015196,281.036348094756,282.035034174316,
283.033720253876,284.032406333436,285.031092412996,285.884931476671),
 .UNSPECIFIED.);
#704=B_SPLINE_CURVE_WITH_KNOTS('',3,(#44942,#44943,#44944,#44945,#44946,
#44947,#44948,#44949,#44950,#44951,#44952),.UNSPECIFIED.,.F.,.F.,(4,1,1,
1,1,1,1,1,4),(279.601746169492,279.719816660684,280.718502740244,281.717188819804,
282.715874899364,283.714560978924,284.713247058484,285.711933138043,285.884931476671),
 .UNSPECIFIED.);
#705=B_SPLINE_CURVE_WITH_KNOTS('',3,(#44957,#44958,#44959,#44960,#44961,
#44962,#44963,#44964,#44965,#44966),.UNSPECIFIED.,.F.,.F.,(4,1,1,1,1,1,
1,4),(273.318560862312,274.045545537836,275.044231617396,276.042917696956,
277.041603776516,278.040289856076,279.038975935636,279.601746169492),
 .UNSPECIFIED.);
#706=B_SPLINE_CURVE_WITH_KNOTS('',3,(#44967,#44968,#44969,#44970,#44971,
#44972,#44973,#44974,#44975,#44976),.UNSPECIFIED.,.F.,.F.,(4,1,1,1,1,1,
1,4),(273.318560862312,273.727700183324,274.726386262884,275.725072342444,
276.723758422004,277.722444501564,278.721130581124,279.601746169492),
 .UNSPECIFIED.);
#707=B_SPLINE_CURVE_WITH_KNOTS('',3,(#44981,#44982,#44983,#44984,#44985,
#44986,#44987,#44988,#44989,#44990,#44991),.UNSPECIFIED.,.F.,.F.,(4,1,1,
1,1,1,1,1,4),(267.035375555133,267.054742980917,268.053429060477,269.052115140037,
270.050801219597,271.049487299156,272.048173378716,273.046859458276,273.318560862312),
 .UNSPECIFIED.);
#708=B_SPLINE_CURVE_WITH_KNOTS('',3,(#44992,#44993,#44994,#44995,#44996,
#44997,#44998,#44999,#45000,#45001),.UNSPECIFIED.,.F.,.F.,(4,1,1,1,1,1,
1,4),(267.035375555133,267.735583705964,268.734269785524,269.732955865084,
270.731641944644,271.730328024204,272.729014103764,273.318560862312),
 .UNSPECIFIED.);
#709=B_SPLINE_CURVE_WITH_KNOTS('',3,(#45006,#45007,#45008,#45009,#45010,
#45011,#45012,#45013,#45014,#45015),.UNSPECIFIED.,.F.,.F.,(4,1,1,1,1,1,
1,4),(260.752190247953,261.062626503557,262.061312583117,263.059998662677,
264.058684742237,265.057370821797,266.056056901357,267.035375555133),
 .UNSPECIFIED.);
#710=B_SPLINE_CURVE_WITH_KNOTS('',3,(#45016,#45017,#45018,#45019,#45020,
#45021,#45022,#45023,#45024,#45025),.UNSPECIFIED.,.F.,.F.,(4,1,1,1,1,1,
1,4),(260.752190247953,261.743467228605,262.742153308165,263.740839387725,
264.739525467284,265.738211546844,266.736897626404,267.035375555133),
 .UNSPECIFIED.);
#711=B_SPLINE_CURVE_WITH_KNOTS('',3,(#45030,#45031,#45032,#45033,#45034,
#45035,#45036,#45037,#45038,#45039),.UNSPECIFIED.,.F.,.F.,(4,1,1,1,1,1,
1,4),(254.469004940773,255.070510026197,256.069196105757,257.067882185317,
258.066568264877,259.065254344437,260.063940423997,260.752190247953),
 .UNSPECIFIED.);
#712=B_SPLINE_CURVE_WITH_KNOTS('',3,(#45040,#45041,#45042,#45043,#45044,
#45045,#45046,#45047,#45048,#45049,#45050),.UNSPECIFIED.,.F.,.F.,(4,1,1,
1,1,1,1,1,4),(254.469004940774,254.752664671685,255.751350751245,256.750036830805,
257.748722910365,258.747408989925,259.746095069485,260.744781149045,260.752190247953),
 .UNSPECIFIED.);
#713=B_SPLINE_CURVE_WITH_KNOTS('',3,(#45055,#45056,#45057,#45058,#45059,
#45060,#45061,#45062,#45063,#45064),.UNSPECIFIED.,.F.,.F.,(4,1,1,1,1,1,
1,4),(248.185819633594,249.078393548838,250.077079628397,251.075765707957,
252.074451787517,253.073137867077,254.071823946637,254.469004940773),
 .UNSPECIFIED.);
#714=B_SPLINE_CURVE_WITH_KNOTS('',3,(#45065,#45066,#45067,#45068,#45069,
#45070,#45071,#45072,#45073,#45074),.UNSPECIFIED.,.F.,.F.,(4,1,1,1,1,1,
1,4),(248.185819633594,248.760548194325,249.759234273885,250.757920353445,
251.756606433005,252.755292512565,253.753978592125,254.469004940774),
 .UNSPECIFIED.);
#715=B_SPLINE_CURVE_WITH_KNOTS('',3,(#45079,#45080,#45081,#45082,#45083,
#45084,#45085,#45086,#45087,#45088,#45089),.UNSPECIFIED.,.F.,.F.,(4,1,1,
1,1,1,1,1,4),(241.902634326414,242.087590991918,243.086277071478,244.084963151038,
245.083649230598,246.082335310158,247.081021389718,248.079707469278,248.185819633594),
 .UNSPECIFIED.);
#716=B_SPLINE_CURVE_WITH_KNOTS('',3,(#45090,#45091,#45092,#45093,#45094,
#45095,#45096,#45097,#45098,#45099),.UNSPECIFIED.,.F.,.F.,(4,1,1,1,1,1,
1,4),(241.902634326415,242.768431716966,243.767117796525,244.765803876085,
245.764489955645,246.763176035205,247.761862114765,248.185819633594),
 .UNSPECIFIED.);
#717=B_SPLINE_CURVE_WITH_KNOTS('',3,(#45104,#45105,#45106,#45107,#45108,
#45109,#45110,#45111,#45112,#45113),.UNSPECIFIED.,.F.,.F.,(4,1,1,1,1,1,
1,4),(235.619449019235,236.095474514558,237.094160594118,238.092846673678,
239.091532753238,240.090218832798,241.088904912358,241.902634326414),
 .UNSPECIFIED.);
#718=B_SPLINE_CURVE_WITH_KNOTS('',3,(#45114,#45115,#45116,#45117,#45118,
#45119,#45120,#45121,#45122,#45123,#45124),.UNSPECIFIED.,.F.,.F.,(4,1,1,
1,1,1,1,1,4),(235.619449019235,235.777629160046,236.776315239606,237.775001319166,
238.773687398726,239.772373478286,240.771059557846,241.769745637406,241.902634326415),
 .UNSPECIFIED.);
#719=B_SPLINE_CURVE_WITH_KNOTS('',3,(#45129,#45130,#45131,#45132,#45133,
#45134,#45135,#45136,#45137,#45138),.UNSPECIFIED.,.F.,.F.,(4,1,1,1,1,1,
1,4),(229.336263712055,230.103358037198,231.102044116758,232.100730196318,
233.099416275878,234.098102355438,235.096788434998,235.619449019235),
 .UNSPECIFIED.);
#720=B_SPLINE_CURVE_WITH_KNOTS('',3,(#45139,#45140,#45141,#45142,#45143,
#45144,#45145,#45146,#45147,#45148),.UNSPECIFIED.,.F.,.F.,(4,1,1,1,1,1,
1,4),(229.336263712055,229.785512682686,230.784198762246,231.782884841806,
232.781570921366,233.780257000926,234.778943080486,235.619449019235),
 .UNSPECIFIED.);
#721=B_SPLINE_CURVE_WITH_KNOTS('',3,(#45153,#45154,#45155,#45156,#45157,
#45158,#45159,#45160,#45161,#45162,#45163),.UNSPECIFIED.,.F.,.F.,(4,1,1,
1,1,1,1,1,4),(223.053078404876,223.112555480279,224.111241559839,225.109927639399,
226.108613718959,227.107299798519,228.105985878079,229.104671957639,229.336263712055),
 .UNSPECIFIED.);
#722=B_SPLINE_CURVE_WITH_KNOTS('',3,(#45164,#45165,#45166,#45167,#45168,
#45169,#45170,#45171,#45172,#45173),.UNSPECIFIED.,.F.,.F.,(4,1,1,1,1,1,
1,4),(223.053078404876,223.793396205326,224.792082284886,225.790768364446,
226.789454444006,227.788140523566,228.786826603126,229.336263712055),
 .UNSPECIFIED.);
#723=B_SPLINE_CURVE_WITH_KNOTS('',3,(#45178,#45179,#45180,#45181,#45182,
#45183,#45184,#45185,#45186,#45187),.UNSPECIFIED.,.F.,.F.,(4,1,1,1,1,1,
1,4),(216.769893097696,217.120439002919,218.119125082479,219.117811162039,
220.116497241599,221.115183321159,222.113869400719,223.053078404876),
 .UNSPECIFIED.);
#724=B_SPLINE_CURVE_WITH_KNOTS('',3,(#45188,#45189,#45190,#45191,#45192,
#45193,#45194,#45195,#45196,#45197,#45198),.UNSPECIFIED.,.F.,.F.,(4,1,1,
1,1,1,1,1,4),(216.769893097696,216.802593648407,217.801279727967,218.799965807527,
219.798651887087,220.797337966647,221.796024046207,222.794710125767,223.053078404876),
 .UNSPECIFIED.);
#725=B_SPLINE_CURVE_WITH_KNOTS('',3,(#45203,#45204,#45205,#45206,#45207,
#45208,#45209,#45210,#45211,#45212),.UNSPECIFIED.,.F.,.F.,(4,1,1,1,1,1,
1,4),(210.486707790517,211.128322525559,212.127008605119,213.125694684679,
214.124380764239,215.123066843799,216.121752923359,216.769893097696),
 .UNSPECIFIED.);
#726=B_SPLINE_CURVE_WITH_KNOTS('',3,(#45213,#45214,#45215,#45216,#45217,
#45218,#45219,#45220,#45221,#45222),.UNSPECIFIED.,.F.,.F.,(4,1,1,1,1,1,
1,4),(210.486707790517,210.810477171047,211.809163250607,212.807849330167,
213.806535409727,214.805221489287,215.803907568847,216.769893097696),
 .UNSPECIFIED.);
#727=B_SPLINE_CURVE_WITH_KNOTS('',3,(#45227,#45228,#45229,#45230,#45231,
#45232,#45233,#45234,#45235,#45236),.UNSPECIFIED.,.F.,.F.,(4,1,1,1,1,1,
1,4),(204.203522483337,205.1362060482,206.13489212776,207.13357820732,208.13226428688,
209.130950366439,210.129636445999,210.486707790517),.UNSPECIFIED.);
#728=B_SPLINE_CURVE_WITH_KNOTS('',3,(#45237,#45238,#45239,#45240,#45241,
#45242,#45243,#45244,#45245,#45246),.UNSPECIFIED.,.F.,.F.,(4,1,1,1,1,1,
1,4),(204.203522483337,204.818360693687,205.817046773247,206.815732852807,
207.814418932367,208.813105011927,209.811791091487,210.486707790517),
 .UNSPECIFIED.);
#729=B_SPLINE_CURVE_WITH_KNOTS('',3,(#45251,#45252,#45253,#45254,#45255,
#45256,#45257,#45258,#45259,#45260,#45261),.UNSPECIFIED.,.F.,.F.,(4,1,1,
1,1,1,1,1,4),(197.920337176157,198.14540349128,199.14408957084,200.1427756504,
201.14146172996,202.14014780952,203.13883388908,204.13751996864,204.203522483337),
 .UNSPECIFIED.);
#730=B_SPLINE_CURVE_WITH_KNOTS('',3,(#45262,#45263,#45264,#45265,#45266,
#45267,#45268,#45269,#45270,#45271),.UNSPECIFIED.,.F.,.F.,(4,1,1,1,1,1,
1,4),(197.920337176158,198.826244216328,199.824930295888,200.823616375448,
201.822302455008,202.820988534567,203.819674614127,204.203522483337),
 .UNSPECIFIED.);
#731=B_SPLINE_CURVE_WITH_KNOTS('',3,(#45276,#45277,#45278,#45279,#45280,
#45281,#45282,#45283,#45284,#45285),.UNSPECIFIED.,.F.,.F.,(4,1,1,1,1,1,
1,4),(191.637151868978,192.15328701392,193.15197309348,194.15065917304,
195.1493452526,196.14803133216,197.14671741172,197.920337176157),
 .UNSPECIFIED.);
#732=B_SPLINE_CURVE_WITH_KNOTS('',3,(#45286,#45287,#45288,#45289,#45290,
#45291,#45292,#45293,#45294,#45295,#45296),.UNSPECIFIED.,.F.,.F.,(4,1,1,
1,1,1,1,1,4),(191.637151868978,191.835441659408,192.834127738968,193.832813818528,
194.831499898088,195.830185977648,196.828872057208,197.827558136768,197.920337176158),
 .UNSPECIFIED.);
#733=B_SPLINE_CURVE_WITH_KNOTS('',3,(#45301,#45302,#45303,#45304,#45305,
#45306,#45307,#45308,#45309,#45310),.UNSPECIFIED.,.F.,.F.,(4,1,1,1,1,1,
1,4),(185.353966561798,186.161170536561,187.159856616121,188.158542695681,
189.15722877524,190.1559148548,191.15460093436,191.637151868978),
 .UNSPECIFIED.);
#734=B_SPLINE_CURVE_WITH_KNOTS('',3,(#45311,#45312,#45313,#45314,#45315,
#45316,#45317,#45318,#45319,#45320),.UNSPECIFIED.,.F.,.F.,(4,1,1,1,1,1,
1,4),(185.353966561798,185.843325182048,186.842011261608,187.840697341168,
188.839383420728,189.838069500288,190.836755579848,191.637151868978),
 .UNSPECIFIED.);
#735=B_SPLINE_CURVE_WITH_KNOTS('',3,(#45325,#45326,#45327,#45328,#45329,
#45330,#45331,#45332,#45333,#45334,#45335),.UNSPECIFIED.,.F.,.F.,(4,1,1,
1,1,1,1,1,4),(179.070781254619,179.170367979641,180.169054059201,181.167740138761,
182.166426218321,183.165112297881,184.163798377441,185.162484457001,185.353966561798),
 .UNSPECIFIED.);
#736=B_SPLINE_CURVE_WITH_KNOTS('',3,(#45336,#45337,#45338,#45339,#45340,
#45341,#45342,#45343,#45344,#45345),.UNSPECIFIED.,.F.,.F.,(4,1,1,1,1,1,
1,4),(179.070781254619,179.851208704689,180.849894784249,181.848580863809,
182.847266943368,183.845953022928,184.844639102488,185.353966561798),
 .UNSPECIFIED.);
#737=B_SPLINE_CURVE_WITH_KNOTS('',3,(#45350,#45351,#45352,#45353,#45354,
#45355,#45356,#45357,#45358,#45359),.UNSPECIFIED.,.F.,.F.,(4,1,1,1,1,1,
1,4),(172.787595947439,173.178251502281,174.176937581841,175.175623661401,
176.174309740961,177.172995820521,178.171681900081,179.070781254619),
 .UNSPECIFIED.);
#738=B_SPLINE_CURVE_WITH_KNOTS('',3,(#45360,#45361,#45362,#45363,#45364,
#45365,#45366,#45367,#45368,#45369,#45370),.UNSPECIFIED.,.F.,.F.,(4,1,1,
1,1,1,1,1,4),(172.787595947439,172.860406147769,173.859092227329,174.857778306889,
175.856464386449,176.855150466009,177.853836545569,178.852522625129,179.070781254619),
 .UNSPECIFIED.);
#739=B_SPLINE_CURVE_WITH_KNOTS('',3,(#45375,#45376,#45377,#45378,#45379,
#45380,#45381,#45382,#45383,#45384),.UNSPECIFIED.,.F.,.F.,(4,1,1,1,1,1,
1,4),(166.50441064026,167.186135024922,168.184821104482,169.183507184041,
170.182193263601,171.180879343161,172.179565422721,172.787595947439),
 .UNSPECIFIED.);
#740=B_SPLINE_CURVE_WITH_KNOTS('',3,(#45385,#45386,#45387,#45388,#45389,
#45390,#45391,#45392,#45393,#45394),.UNSPECIFIED.,.F.,.F.,(4,1,1,1,1,1,
1,4),(166.50441064026,166.868289670409,167.866975749969,168.865661829529,
169.864347909089,170.863033988649,171.861720068209,172.787595947439),
 .UNSPECIFIED.);
#741=B_SPLINE_CURVE_WITH_KNOTS('',3,(#45399,#45400,#45401,#45402,#45403,
#45404,#45405,#45406,#45407,#45408),.UNSPECIFIED.,.F.,.F.,(4,1,1,1,1,1,
1,4),(160.22122533308,161.194018547562,162.192704627122,163.191390706682,
164.190076786242,165.188762865802,166.187448945362,166.50441064026),
 .UNSPECIFIED.);
#742=B_SPLINE_CURVE_WITH_KNOTS('',3,(#45409,#45410,#45411,#45412,#45413,
#45414,#45415,#45416,#45417,#45418),.UNSPECIFIED.,.F.,.F.,(4,1,1,1,1,1,
1,4),(160.22122533308,160.87617319305,161.874859272609,162.873545352169,
163.872231431729,164.870917511289,165.869603590849,166.50441064026),
 .UNSPECIFIED.);
#743=B_SPLINE_CURVE_WITH_KNOTS('',3,(#45423,#45424,#45425,#45426,#45427,
#45428,#45429,#45430,#45431,#45432,#45433),.UNSPECIFIED.,.F.,.F.,(4,1,1,
1,1,1,1,1,4),(153.9380400259,154.203215990642,155.201902070202,156.200588149762,
157.199274229322,158.197960308882,159.196646388442,160.195332468002,160.22122533308),
 .UNSPECIFIED.);
#744=B_SPLINE_CURVE_WITH_KNOTS('',3,(#45434,#45435,#45436,#45437,#45438,
#45439,#45440,#45441,#45442,#45443),.UNSPECIFIED.,.F.,.F.,(4,1,1,1,1,1,
1,4),(153.938040025901,154.88405671569,155.88274279525,156.88142887481,
157.88011495437,158.87880103393,159.87748711349,160.22122533308),
 .UNSPECIFIED.);
#745=B_SPLINE_CURVE_WITH_KNOTS('',3,(#45448,#45449,#45450,#45451,#45452,
#45453,#45454,#45455,#45456,#45457),.UNSPECIFIED.,.F.,.F.,(4,1,1,1,1,1,
1,4),(147.654854718721,148.211099513282,149.209785592842,150.208471672402,
151.207157751962,152.205843831522,153.204529911082,153.9380400259),
 .UNSPECIFIED.);
#746=B_SPLINE_CURVE_WITH_KNOTS('',3,(#45458,#45459,#45460,#45461,#45462,
#45463,#45464,#45465,#45466,#45467,#45468),.UNSPECIFIED.,.F.,.F.,(4,1,1,
1,1,1,1,1,4),(147.654854718721,147.89325415877,148.89194023833,149.89062631789,
150.88931239745,151.88799847701,152.88668455657,153.88537063613,153.938040025901),
 .UNSPECIFIED.);
#747=B_SPLINE_CURVE_WITH_KNOTS('',3,(#45473,#45474,#45475,#45476,#45477,
#45478,#45479,#45480,#45481,#45482),.UNSPECIFIED.,.F.,.F.,(4,1,1,1,1,1,
1,4),(141.371669411541,142.218983035923,143.217669115483,144.216355195043,
145.215041274603,146.213727354163,147.212413433723,147.654854718721),
 .UNSPECIFIED.);
#748=B_SPLINE_CURVE_WITH_KNOTS('',3,(#45483,#45484,#45485,#45486,#45487,
#45488,#45489,#45490,#45491,#45492),.UNSPECIFIED.,.F.,.F.,(4,1,1,1,1,1,
1,4),(141.371669411542,141.90113768141,142.89982376097,143.89850984053,
144.89719592009,145.89588199965,146.89456807921,147.654854718721),
 .UNSPECIFIED.);
#749=B_SPLINE_CURVE_WITH_KNOTS('',3,(#45497,#45498,#45499,#45500,#45501,
#45502,#45503,#45504,#45505,#45506,#45507),.UNSPECIFIED.,.F.,.F.,(4,1,1,
1,1,1,1,1,4),(135.088484104362,135.228180479003,136.226866558563,137.225552638123,
138.224238717683,139.222924797243,140.221610876803,141.220296956363,141.371669411541),
 .UNSPECIFIED.);
#750=B_SPLINE_CURVE_WITH_KNOTS('',3,(#45508,#45509,#45510,#45511,#45512,
#45513,#45514,#45515,#45516,#45517),.UNSPECIFIED.,.F.,.F.,(4,1,1,1,1,1,
1,4),(135.088484104362,135.909021204051,136.907707283611,137.906393363171,
138.905079442731,139.903765522291,140.90245160185,141.371669411542),
 .UNSPECIFIED.);
#751=B_SPLINE_CURVE_WITH_KNOTS('',3,(#45522,#45523,#45524,#45525,#45526,
#45527,#45528,#45529,#45530,#45531),.UNSPECIFIED.,.F.,.F.,(4,1,1,1,1,1,
1,4),(128.805298797182,129.236064001643,130.234750081203,131.233436160763,
132.232122240323,133.230808319883,134.229494399443,135.088484104362),
 .UNSPECIFIED.);
#752=B_SPLINE_CURVE_WITH_KNOTS('',3,(#45532,#45533,#45534,#45535,#45536,
#45537,#45538,#45539,#45540,#45541,#45542),.UNSPECIFIED.,.F.,.F.,(4,1,1,
1,1,1,1,1,4),(128.805298797182,128.918218647131,129.916904726691,130.915590806251,
131.914276885811,132.912962965371,133.911649044931,134.910335124491,135.088484104362),
 .UNSPECIFIED.);
#753=B_SPLINE_CURVE_WITH_KNOTS('',3,(#45547,#45548,#45549,#45550,#45551,
#45552,#45553,#45554,#45555,#45556),.UNSPECIFIED.,.F.,.F.,(4,1,1,1,1,1,
1,4),(122.522113490003,123.243947524284,124.242633603844,125.241319683404,
126.240005762964,127.238691842524,128.237377922083,128.805298797182),
 .UNSPECIFIED.);
#754=B_SPLINE_CURVE_WITH_KNOTS('',3,(#45557,#45558,#45559,#45560,#45561,
#45562,#45563,#45564,#45565,#45566),.UNSPECIFIED.,.F.,.F.,(4,1,1,1,1,1,
1,4),(122.522113490003,122.926102169771,123.924788249331,124.923474328891,
125.922160408451,126.920846488011,127.919532567571,128.805298797182),
 .UNSPECIFIED.);
#755=B_SPLINE_CURVE_WITH_KNOTS('',3,(#45571,#45572,#45573,#45574,#45575,
#45576,#45577,#45578,#45579,#45580,#45581),.UNSPECIFIED.,.F.,.F.,(4,1,1,
1,1,1,1,1,4),(116.238928182823,116.253144967364,117.251831046924,118.250517126484,
119.249203206044,120.247889285604,121.246575365164,122.245261444724,122.522113490003),
 .UNSPECIFIED.);
#756=B_SPLINE_CURVE_WITH_KNOTS('',3,(#45582,#45583,#45584,#45585,#45586,
#45587,#45588,#45589,#45590,#45591),.UNSPECIFIED.,.F.,.F.,(4,1,1,1,1,1,
1,4),(116.238928182823,116.933985692412,117.932671771972,118.931357851532,
119.930043931092,120.928730010651,121.927416090211,122.522113490003),
 .UNSPECIFIED.);
#757=B_SPLINE_CURVE_WITH_KNOTS('',3,(#45596,#45597,#45598,#45599,#45600,
#45601,#45602,#45603,#45604,#45605),.UNSPECIFIED.,.F.,.F.,(4,1,1,1,1,1,
1,4),(109.955742875643,110.261028490004,111.259714569564,112.258400649124,
113.257086728684,114.255772808244,115.254458887804,116.238928182823),
 .UNSPECIFIED.);
#758=B_SPLINE_CURVE_WITH_KNOTS('',3,(#45606,#45607,#45608,#45609,#45610,
#45611,#45612,#45613,#45614,#45615),.UNSPECIFIED.,.F.,.F.,(4,1,1,1,1,1,
1,4),(109.955742875644,110.941869215052,111.940555294612,112.939241374172,
113.937927453732,114.936613533292,115.935299612852,116.238928182823),
 .UNSPECIFIED.);
#759=B_SPLINE_CURVE_WITH_KNOTS('',3,(#45620,#45621,#45622,#45623,#45624,
#45625,#45626,#45627,#45628,#45629),.UNSPECIFIED.,.F.,.F.,(4,1,1,1,1,1,
1,4),(103.672557568464,104.268912012645,105.267598092205,106.266284171765,
107.264970251324,108.263656330884,109.262342410444,109.955742875643),
 .UNSPECIFIED.);
#760=B_SPLINE_CURVE_WITH_KNOTS('',3,(#45630,#45631,#45632,#45633,#45634,
#45635,#45636,#45637,#45638,#45639,#45640),.UNSPECIFIED.,.F.,.F.,(4,1,1,
1,1,1,1,1,4),(103.672557568464,103.951066658132,104.949752737692,105.948438817252,
106.947124896812,107.945810976372,108.944497055932,109.943183135492,109.955742875644),
 .UNSPECIFIED.);
#761=B_SPLINE_CURVE_WITH_KNOTS('',3,(#45645,#45646,#45647,#45648,#45649,
#45650,#45651,#45652,#45653,#45654),.UNSPECIFIED.,.F.,.F.,(4,1,1,1,1,1,
1,4),(97.3893722612842,98.2767955352849,99.2754816148449,100.274167694405,
101.272853773965,102.271539853525,103.270225933085,103.672557568464),
 .UNSPECIFIED.);
#762=B_SPLINE_CURVE_WITH_KNOTS('',3,(#45655,#45656,#45657,#45658,#45659,
#45660,#45661,#45662,#45663,#45664),.UNSPECIFIED.,.F.,.F.,(4,1,1,1,1,1,
1,4),(97.3893722612844,97.9589501807726,98.9576362603325,99.9563223398925,
100.955008419452,101.953694499012,102.952380578572,103.672557568464),
 .UNSPECIFIED.);
#763=B_SPLINE_CURVE_WITH_KNOTS('',3,(#45669,#45670,#45671,#45672,#45673,
#45674,#45675,#45676,#45677,#45678,#45679),.UNSPECIFIED.,.F.,.F.,(4,1,1,
1,1,1,1,1,4),(91.1061869541046,91.2859929783653,92.2846790579252,93.2833651374852,
94.2820512170451,95.2807372966051,96.279423376165,97.278109455725,97.3893722612842),
 .UNSPECIFIED.);
#764=B_SPLINE_CURVE_WITH_KNOTS('',3,(#45680,#45681,#45682,#45683,#45684,
#45685,#45686,#45687,#45688,#45689),.UNSPECIFIED.,.F.,.F.,(4,1,1,1,1,1,
1,4),(91.1061869541048,91.9668337034129,92.9655197829728,93.9642058625328,
94.9628919420927,95.9615780216527,96.9602641012126,97.3893722612844),
 .UNSPECIFIED.);
#765=B_SPLINE_CURVE_WITH_KNOTS('',3,(#45694,#45695,#45696,#45697,#45698,
#45699,#45700,#45701,#45702,#45703),.UNSPECIFIED.,.F.,.F.,(4,1,1,1,1,1,
1,4),(84.8230016469251,85.2938765010056,86.2925625805655,87.2912486601255,
88.2899347396854,89.2886208192454,90.2873068988053,91.1061869541046),
 .UNSPECIFIED.);
#766=B_SPLINE_CURVE_WITH_KNOTS('',3,(#45704,#45705,#45706,#45707,#45708,
#45709,#45710,#45711,#45712,#45713,#45714),.UNSPECIFIED.,.F.,.F.,(4,1,1,
1,1,1,1,1,4),(84.8230016469252,84.9760311464932,85.9747172260532,86.9734033056131,
87.9720893851731,88.970775464733,89.969461544293,90.9681476238529,91.1061869541048),
 .UNSPECIFIED.);
#767=B_SPLINE_CURVE_WITH_KNOTS('',3,(#45719,#45720,#45721,#45722,#45723,
#45724,#45725,#45726,#45727,#45728),.UNSPECIFIED.,.F.,.F.,(4,1,1,1,1,1,
1,4),(78.5398163397455,79.3017600236459,80.3004461032058,81.2991321827658,
82.2978182623257,83.2965043418857,84.2951904214456,84.8230016469251),
 .UNSPECIFIED.);
#768=B_SPLINE_CURVE_WITH_KNOTS('',3,(#45729,#45730,#45731,#45732,#45733,
#45734,#45735,#45736,#45737,#45738),.UNSPECIFIED.,.F.,.F.,(4,1,1,1,1,1,
1,4),(78.5398163397457,78.9839146691335,79.9826007486935,80.9812868282534,
81.9799729078134,82.9786589873733,83.9773450669333,84.8230016469252),
 .UNSPECIFIED.);
#769=B_SPLINE_CURVE_WITH_KNOTS('',3,(#45743,#45744,#45745,#45746,#45747,
#45748,#45749,#45750,#45751,#45752,#45753),.UNSPECIFIED.,.F.,.F.,(4,1,1,
1,1,1,1,1,4),(72.2566310325659,72.3109574667262,73.3096435462861,74.3083296258461,
75.307015705406,76.305701784966,77.3043878645259,78.3030739440859,78.5398163397455),
 .UNSPECIFIED.);
#770=B_SPLINE_CURVE_WITH_KNOTS('',3,(#45754,#45755,#45756,#45757,#45758,
#45759,#45760,#45761,#45762,#45763),.UNSPECIFIED.,.F.,.F.,(4,1,1,1,1,1,
1,4),(72.256631032566,72.9917981917738,73.9904842713337,74.9891703508937,
75.9878564304536,76.9865425100136,77.9852285895736,78.5398163397457),
 .UNSPECIFIED.);
#771=B_SPLINE_CURVE_WITH_KNOTS('',3,(#45768,#45769,#45770,#45771,#45772,
#45773,#45774,#45775,#45776,#45777),.UNSPECIFIED.,.F.,.F.,(4,1,1,1,1,1,
1,4),(65.9734457253862,66.3188409893665,67.3175270689264,68.3162131484864,
69.3148992280463,70.3135853076063,71.3122713871662,72.2566310325659),
 .UNSPECIFIED.);
#772=B_SPLINE_CURVE_WITH_KNOTS('',3,(#45778,#45779,#45780,#45781,#45782,
#45783,#45784,#45785,#45786,#45787,#45788),.UNSPECIFIED.,.F.,.F.,(4,1,1,
1,1,1,1,1,4),(65.9734457253864,66.0009956348541,66.9996817144141,67.998367793974,
68.997053873534,69.9957399530939,70.9944260326539,71.9931121122139,72.256631032566),
 .UNSPECIFIED.);
#773=B_SPLINE_CURVE_WITH_KNOTS('',3,(#45793,#45794,#45795,#45796,#45797,
#45798,#45799,#45800,#45801,#45802),.UNSPECIFIED.,.F.,.F.,(4,1,1,1,1,1,
1,4),(59.6902604182067,60.3267245120068,61.3254105915667,62.3240966711267,
63.3227827506866,64.3214688302466,65.3201549098065,65.9734457253862),
 .UNSPECIFIED.);
#774=B_SPLINE_CURVE_WITH_KNOTS('',3,(#45803,#45804,#45805,#45806,#45807,
#45808,#45809,#45810,#45811,#45812),.UNSPECIFIED.,.F.,.F.,(4,1,1,1,1,1,
1,4),(59.6902604182069,60.0088791574944,61.0075652370544,62.0062513166143,
63.0049373961743,64.0036234757342,65.0023095552942,65.9734457253864),
 .UNSPECIFIED.);
#775=B_SPLINE_CURVE_WITH_KNOTS('',3,(#45817,#45818,#45819,#45820,#45821,
#45822,#45823,#45824,#45825,#45826),.UNSPECIFIED.,.F.,.F.,(4,1,1,1,1,1,
1,4),(53.4070751110271,54.3346080346471,55.333294114207,56.331980193767,
57.3306662733269,58.3293523528869,59.3280384324468,59.6902604182067),
 .UNSPECIFIED.);
#776=B_SPLINE_CURVE_WITH_KNOTS('',3,(#45827,#45828,#45829,#45830,#45831,
#45832,#45833,#45834,#45835,#45836),.UNSPECIFIED.,.F.,.F.,(4,1,1,1,1,1,
1,4),(53.4070751110273,54.0167626801347,55.0154487596947,56.0141348392546,
57.0128209188146,58.0115069983745,59.0101930779345,59.6902604182069),
 .UNSPECIFIED.);
#777=B_SPLINE_CURVE_WITH_KNOTS('',3,(#45841,#45842,#45843,#45844,#45845,
#45846,#45847,#45848,#45849,#45850,#45851),.UNSPECIFIED.,.F.,.F.,(4,1,1,
1,1,1,1,1,4),(47.1238898038475,47.3438054777274,48.3424915572874,49.3411776368473,
50.3398637164073,51.3385497959672,52.3372358755272,53.3359219550871,53.4070751110271),
 .UNSPECIFIED.);
#778=B_SPLINE_CURVE_WITH_KNOTS('',3,(#45852,#45853,#45854,#45855,#45856,
#45857,#45858,#45859,#45860,#45861),.UNSPECIFIED.,.F.,.F.,(4,1,1,1,1,1,
1,4),(47.1238898038477,48.024646202775,49.023332282335,50.0220183618949,
51.0207044414549,52.0193905210148,53.0180766005748,53.4070751110273),
 .UNSPECIFIED.);
#779=B_SPLINE_CURVE_WITH_KNOTS('',3,(#45866,#45867,#45868,#45869,#45870,
#45871,#45872,#45873,#45874,#45875),.UNSPECIFIED.,.F.,.F.,(4,1,1,1,1,1,
1,4),(40.8407044966679,41.3516890003677,42.3503750799277,43.3490611594876,
44.3477472390476,45.3464333186075,46.3451193981675,47.1238898038475),
 .UNSPECIFIED.);
#780=B_SPLINE_CURVE_WITH_KNOTS('',3,(#45876,#45877,#45878,#45879,#45880,
#45881,#45882,#45883,#45884,#45885,#45886),.UNSPECIFIED.,.F.,.F.,(4,1,1,
1,1,1,1,1,4),(40.8407044966681,41.0338436458553,42.0325297254153,43.0312158049753,
44.0299018845352,45.0285879640952,46.0272740436551,47.0259601232151,47.1238898038477),
 .UNSPECIFIED.);
#781=B_SPLINE_CURVE_WITH_KNOTS('',3,(#45891,#45892,#45893,#45894,#45895,
#45896,#45897,#45898,#45899,#45900),.UNSPECIFIED.,.F.,.F.,(4,1,1,1,1,1,
1,4),(34.5575191894883,35.359572523008,36.358258602568,37.3569446821279,
38.3556307616879,39.3543168412478,40.3530029208078,40.8407044966679),
 .UNSPECIFIED.);
#782=B_SPLINE_CURVE_WITH_KNOTS('',3,(#45901,#45902,#45903,#45904,#45905,
#45906,#45907,#45908,#45909,#45910),.UNSPECIFIED.,.F.,.F.,(4,1,1,1,1,1,
1,4),(34.5575191894885,35.0417271684956,36.0404132480556,37.0390993276155,
38.0377854071755,39.0364714867355,40.0351575662954,40.8407044966681),
 .UNSPECIFIED.);
#783=B_SPLINE_CURVE_WITH_KNOTS('',3,(#45915,#45916,#45917,#45918,#45919,
#45920,#45921,#45922,#45923,#45924,#45925),.UNSPECIFIED.,.F.,.F.,(4,1,1,
1,1,1,1,1,4),(28.2743338823087,28.3687699660883,29.3674560456483,30.3661421252082,
31.3648282047682,32.3635142843282,33.3622003638881,34.3608864434481,34.5575191894883),
 .UNSPECIFIED.);
#784=B_SPLINE_CURVE_WITH_KNOTS('',3,(#45926,#45927,#45928,#45929,#45930,
#45931,#45932,#45933,#45934,#45935),.UNSPECIFIED.,.F.,.F.,(4,1,1,1,1,1,
1,4),(28.2743338823089,29.0496106911359,30.0482967706959,31.0469828502558,
32.0456689298158,33.0443550093757,34.0430410889357,34.5575191894885),
 .UNSPECIFIED.);
#785=B_SPLINE_CURVE_WITH_KNOTS('',3,(#45940,#45941,#45942,#45943,#45944,
#45945,#45946,#45947,#45948,#45949),.UNSPECIFIED.,.F.,.F.,(4,1,1,1,1,1,
1,4),(21.9911485751291,22.3766534887286,23.3753395682886,24.3740256478485,
25.3727117274085,26.3713978069684,27.3700838865284,28.2743338823087),
 .UNSPECIFIED.);
#786=B_SPLINE_CURVE_WITH_KNOTS('',3,(#45950,#45951,#45952,#45953,#45954,
#45955,#45956,#45957,#45958,#45959,#45960),.UNSPECIFIED.,.F.,.F.,(4,1,1,
1,1,1,1,1,4),(21.9911485751293,22.0588081342163,23.0574942137762,24.0561802933362,
25.0548663728961,26.0535524524561,27.052238532016,28.050924611576,28.2743338823089),
 .UNSPECIFIED.);
#787=B_SPLINE_CURVE_WITH_KNOTS('',3,(#45965,#45966,#45967,#45968,#45969,
#45970,#45971,#45972,#45973,#45974),.UNSPECIFIED.,.F.,.F.,(4,1,1,1,1,1,
1,4),(15.7079632679496,16.3845370113689,17.3832230909289,18.3819091704888,
19.3805952500488,20.3792813296087,21.3779674091687,21.9911485751291),
 .UNSPECIFIED.);
#788=B_SPLINE_CURVE_WITH_KNOTS('',3,(#45975,#45976,#45977,#45978,#45979,
#45980,#45981,#45982,#45983,#45984),.UNSPECIFIED.,.F.,.F.,(4,1,1,1,1,1,
1,4),(15.7079632679497,16.0666916568566,17.0653777364165,18.0640638159765,
19.0627498955364,20.0614359750964,21.0601220546563,21.9911485751293),
 .UNSPECIFIED.);
#789=B_SPLINE_CURVE_WITH_KNOTS('',3,(#45987,#45988,#45989,#45990,#45991,
#45992,#45993,#45994,#45995,#45996,#45997,#45998,#45999,#46000,#46001,#46002,
#46003,#46004,#46005,#46006,#46007,#46008,#46009,#46010,#46011,#46012,#46013,
#46014,#46015,#46016,#46017,#46018,#46019,#46020,#46021,#46022,#46023,#46024,
#46025,#46026,#46027,#46028,#46029,#46030,#46031,#46032,#46033,#46034,#46035,
#46036,#46037,#46038),.UNSPECIFIED.,.F.,.F.,(4,3,3,3,3,3,3,3,3,3,3,3,3,
3,3,3,3,4),(-0.276631791712715,-0.26755901985898,-0.245786814899969,-0.233874251841385,
-0.212417712774227,-0.201844136596455,-0.173306013186041,-0.162876402370629,
-0.153623752254054,-0.140564570666302,-0.120812346575674,-0.110858182676873,
-0.10074618282354,-0.0755596371176548,-0.0588540251780687,-0.0493417440450129,
-0.0183248504906759,0.),.UNSPECIFIED.);
#790=B_SPLINE_CURVE_WITH_KNOTS('',3,(#46043,#46044,#46045,#46046,#46047,
#46048,#46049,#46050,#46051,#46052,#46053,#46054,#46055,#46056,#46057,#46058,
#46059,#46060,#46061,#46062,#46063,#46064,#46065,#46066,#46067,#46068,#46069,
#46070,#46071,#46072,#46073,#46074,#46075,#46076,#46077,#46078,#46079,#46080,
#46081,#46082,#46083,#46084,#46085,#46086,#46087,#46088,#46089,#46090,#46091,
#46092,#46093,#46094),.UNSPECIFIED.,.F.,.F.,(4,3,3,3,3,3,3,3,3,3,3,3,3,
3,3,3,3,4),(-0.275362278356787,-0.264292581061059,-0.242714596523907,-0.228543028021742,
-0.209227773008753,-0.199395258896952,-0.189100003351452,-0.159713559956535,
-0.147814894797435,-0.139076691589832,-0.125504176784125,-0.103148327528027,
-0.0941264284167034,-0.0661327433935608,-0.0498049250752028,-0.0407969165022222,
-0.0145455879908767,0.),.UNSPECIFIED.);
#791=B_SPLINE_CURVE_WITH_KNOTS('',3,(#47587,#47588,#47589,#47590,#47591,
#47592,#47593,#47594,#47595,#47596,#47597,#47598,#47599,#47600,#47601,#47602,
#47603,#47604,#47605),.UNSPECIFIED.,.F.,.F.,(4,3,3,3,3,3,4),(361.77757843857,
362.523046880262,363.521732959822,364.520419039382,365.519105118942,366.517791198502,
367.440676763862),.UNSPECIFIED.);
#792=B_SPLINE_CURVE_WITH_KNOTS('',3,(#47607,#47608,#47609,#47610,#47611,
#47612,#47613,#47614,#47615,#47616,#47617,#47618,#47619,#47620,#47621,#47622,
#47623,#47624,#47625,#47626,#47627,#47628,#47629,#47630,#47631,#47632,#47633,
#47634,#47635,#47636,#47637,#47638,#47639,#47640,#47641,#47642,#47643,#47644,
#47645,#47646,#47647,#47648,#47649,#47650,#47651,#47652,#47653,#47654,#47655,
#47656,#47657,#47658),.UNSPECIFIED.,.F.,.F.,(4,3,3,3,3,3,3,3,3,3,3,3,3,
3,3,3,3,4),(-0.276631791712692,-0.267559019858928,-0.245786815023485,-0.233874252356153,
-0.21241770641256,-0.201844136492789,-0.173306013103481,-0.162876405863916,
-0.153623758375204,-0.140564570666252,-0.12081234527961,-0.110858177928118,
-0.100746182189666,-0.0755596366422492,-0.058854022142393,-0.04934174195364,
-0.018324847486917,0.),.UNSPECIFIED.);
#793=B_SPLINE_CURVE_WITH_KNOTS('',3,(#47659,#47660,#47661,#47662,#47663),
 .UNSPECIFIED.,.F.,.F.,(4,1,4),(14.1451200119366,15.0680055772966,15.7079632679497),
 .UNSPECIFIED.);
#794=B_SPLINE_CURVE_WITH_KNOTS('',3,(#47666,#47667,#47668,#47669,#47670,
#47671,#47672,#47673,#47674,#47675,#47676,#47677,#47678,#47679,#47680,#47681,
#47682,#47683,#47684,#47685,#47686,#47687,#47688,#47689,#47690,#47691,#47692,
#47693,#47694,#47695,#47696,#47697,#47698,#47699,#47700,#47701,#47702,#47703,
#47704,#47705,#47706,#47707,#47708,#47709,#47710,#47711,#47712,#47713,#47714,
#47715,#47716,#47717),.UNSPECIFIED.,.F.,.F.,(4,3,3,3,3,3,3,3,3,3,3,3,3,
3,3,3,3,4),(-0.275362278356907,-0.264292581061165,-0.242714595883773,-0.22854302749595,
-0.209227769645797,-0.199395250917095,-0.189100000879922,-0.159713556370167,
-0.147814883828647,-0.139076671830681,-0.125504176784174,-0.103148391122983,
-0.0941264875184657,-0.0661328024083947,-0.0498050734898823,-0.0407969659451433,
-0.0145456388647011,0.),.UNSPECIFIED.);
#795=B_SPLINE_CURVE_WITH_KNOTS('',3,(#47720,#47721,#47722,#47723),
 .UNSPECIFIED.,.F.,.F.,(4,4),(15.385850931809,15.7079632679496),
 .UNSPECIFIED.);
#796=B_SPLINE_CURVE_WITH_KNOTS('',3,(#49216,#49217,#49218,#49219,#49220,
#49221,#49222,#49223,#49224,#49225,#49226,#49227,#49228,#49229,#49230,#49231),
 .UNSPECIFIED.,.F.,.F.,(4,3,3,3,3,4),(-369.513849437182,-368.515163357622,
-367.516477278062,-366.517791198502,-365.519105118942,-364.746860152556),
 .UNSPECIFIED.);
#797=B_SPLINE_CURVE_WITH_KNOTS('',3,(#50095,#50096,#50097,#50098,#50099,
#50100,#50101,#50102,#50103,#50104,#50105,#50106,#50107,#50108,#50109,#50110,
#50111,#50112,#50113,#50114,#50115,#50116),.UNSPECIFIED.,.F.,.F.,(4,3,3,
3,3,3,3,4),(-8.01856088759472,-7.99175481068278,-6.99278545934743,-5.99381610801208,
-4.99484675667673,-3.99587740534139,-2.99690805400604,-2.06659765062437),
 .UNSPECIFIED.);
#798=B_SPLINE_CURVE_WITH_KNOTS('',3,(#50124,#50125,#50126,#50127,#50128,
#50129,#50130,#50131,#50132,#50133,#50134,#50135,#50136,#50137,#50138,#50139,
#50140,#50141,#50142),.UNSPECIFIED.,.F.,.F.,(4,3,3,3,3,3,4),(0.,0.99896935133533,
1.99793870267068,2.99690805400603,3.99587740534138,4.99484675667673,5.04361105059381),
 .UNSPECIFIED.);
#799=B_SPLINE_CURVE_WITH_KNOTS('',3,(#50147,#50148,#50149,#50150,#50151,
#50152,#50153,#50154,#50155,#50156,#50157,#50158,#50159,#50160,#50161,#50162,
#50163,#50164,#50165,#50166,#50167,#50168),.UNSPECIFIED.,.F.,.F.,(4,3,3,
3,3,3,3,4),(-14.3017461947743,-13.9855709186949,-12.9866015673595,-11.9876322160242,
-10.9886628646888,-9.98969351335347,-8.99072416201812,-8.01856088759472),
 .UNSPECIFIED.);
#800=B_SPLINE_CURVE_WITH_KNOTS('',3,(#50169,#50170,#50171,#50172,#50173,
#50174,#50175,#50176,#50177,#50178,#50179,#50180,#50181,#50182,#50183,#50184,
#50185,#50186,#50187,#50188,#50189,#50190),.UNSPECIFIED.,.F.,.F.,(4,3,3,
3,3,3,3,4),(5.04361105059381,5.99381610801208,6.99278545934743,7.99175481068277,
8.99072416201812,9.98969351335347,10.9886628646888,11.3267963577734),
 .UNSPECIFIED.);
#801=B_SPLINE_CURVE_WITH_KNOTS('',3,(#50195,#50196,#50197,#50198,#50199,
#50200,#50201,#50202,#50203,#50204,#50205,#50206,#50207,#50208,#50209,#50210,
#50211,#50212,#50213,#50214,#50215,#50216),.UNSPECIFIED.,.F.,.F.,(4,3,3,
3,3,3,3,4),(-20.5849315019539,-19.9793870267069,-18.9804176753716,-17.9814483240362,
-16.9824789727009,-15.9835096213656,-14.9845402700302,-14.3017461947743),
 .UNSPECIFIED.);
#802=B_SPLINE_CURVE_WITH_KNOTS('',3,(#50217,#50218,#50219,#50220,#50221,
#50222,#50223,#50224,#50225,#50226,#50227,#50228,#50229,#50230,#50231,#50232,
#50233,#50234,#50235,#50236,#50237,#50238),.UNSPECIFIED.,.F.,.F.,(4,3,3,
3,3,3,3,4),(11.3267963577734,11.9876322160242,12.9866015673595,13.9855709186949,
14.9845402700302,15.9835096213656,16.9824789727009,17.609981664953),
 .UNSPECIFIED.);
#803=B_SPLINE_CURVE_WITH_KNOTS('',3,(#50243,#50244,#50245,#50246,#50247,
#50248,#50249,#50250,#50251,#50252,#50253,#50254,#50255,#50256,#50257,#50258,
#50259,#50260,#50261,#50262,#50263,#50264),.UNSPECIFIED.,.F.,.F.,(4,3,3,
3,3,3,3,4),(-26.8681168091335,-25.973203134719,-24.9742337833837,-23.9752644320483,
-22.976295080713,-21.9773257293776,-20.9783563780423,-20.5849315019539),
 .UNSPECIFIED.);
#804=B_SPLINE_CURVE_WITH_KNOTS('',3,(#50265,#50266,#50267,#50268,#50269,
#50270,#50271,#50272,#50273,#50274,#50275,#50276,#50277,#50278,#50279,#50280,
#50281,#50282,#50283,#50284,#50285,#50286),.UNSPECIFIED.,.F.,.F.,(4,3,3,
3,3,3,3,4),(17.609981664953,17.9814483240363,18.9804176753716,19.9793870267069,
20.9783563780423,21.9773257293776,22.976295080713,23.8931669721326),
 .UNSPECIFIED.);
#805=B_SPLINE_CURVE_WITH_KNOTS('',3,(#50291,#50292,#50293,#50294,#50295,
#50296,#50297,#50298,#50299,#50300,#50301,#50302,#50303,#50304,#50305,#50306,
#50307,#50308,#50309,#50310,#50311,#50312,#50313,#50314,#50315),
 .UNSPECIFIED.,.F.,.F.,(4,3,3,3,3,3,3,3,4),(-33.1513021163131,-32.9659885940664,
-31.9670192427311,-30.9680498913958,-29.9690805400604,-28.9701111887251,
-27.9711418373897,-26.9721724860544,-26.8681168091335),.UNSPECIFIED.);
#806=B_SPLINE_CURVE_WITH_KNOTS('',3,(#50316,#50317,#50318,#50319,#50320,
#50321,#50322,#50323,#50324,#50325,#50326,#50327,#50328,#50329,#50330,#50331,
#50332,#50333,#50334,#50335,#50336,#50337,#50338,#50339,#50340),
 .UNSPECIFIED.,.F.,.F.,(4,3,3,3,3,3,3,3,4),(23.8931669721326,23.9752644320483,
24.9742337833837,25.973203134719,26.9721724860544,27.9711418373897,28.970111188725,
29.9690805400604,30.1763522793122),.UNSPECIFIED.);
#807=B_SPLINE_CURVE_WITH_KNOTS('',3,(#50345,#50346,#50347,#50348,#50349,
#50350,#50351,#50352,#50353,#50354,#50355,#50356,#50357,#50358,#50359,#50360,
#50361,#50362,#50363,#50364,#50365,#50366),.UNSPECIFIED.,.F.,.F.,(4,3,3,
3,3,3,3,4),(-39.4344874234927,-38.9598047020785,-37.9608353507432,-36.9618659994078,
-35.9628966480725,-34.9639272967371,-33.9649579454018,-33.1513021163131),
 .UNSPECIFIED.);
#808=B_SPLINE_CURVE_WITH_KNOTS('',3,(#50367,#50368,#50369,#50370,#50371,
#50372,#50373,#50374,#50375,#50376,#50377,#50378,#50379,#50380,#50381,#50382,
#50383,#50384,#50385,#50386,#50387,#50388),.UNSPECIFIED.,.F.,.F.,(4,3,3,
3,3,3,3,4),(30.1763522793122,30.9680498913957,31.9670192427311,32.9659885940664,
33.9649579454018,34.9639272967371,35.9628966480725,36.4595375864917),
 .UNSPECIFIED.);
#809=B_SPLINE_CURVE_WITH_KNOTS('',3,(#50393,#50394,#50395,#50396,#50397,
#50398,#50399,#50400,#50401,#50402,#50403,#50404,#50405,#50406,#50407,#50408,
#50409,#50410,#50411,#50412,#50413,#50414),.UNSPECIFIED.,.F.,.F.,(4,3,3,
3,3,3,3,4),(-45.7176727306722,-44.9536208100906,-43.9546514587553,-42.9556821074199,
-41.9567127560846,-40.9577434047492,-39.9587740534139,-39.4344874234927),
 .UNSPECIFIED.);
#810=B_SPLINE_CURVE_WITH_KNOTS('',3,(#50415,#50416,#50417,#50418,#50419,
#50420,#50421,#50422,#50423,#50424,#50425,#50426,#50427,#50428,#50429,#50430,
#50431,#50432,#50433,#50434,#50435,#50436),.UNSPECIFIED.,.F.,.F.,(4,3,3,
3,3,3,3,4),(36.4595375864917,36.9618659994078,37.9608353507432,38.9598047020785,
39.9587740534139,40.9577434047492,41.9567127560846,42.7427228936713),
 .UNSPECIFIED.);
#811=B_SPLINE_CURVE_WITH_KNOTS('',3,(#50441,#50442,#50443,#50444,#50445,
#50446,#50447,#50448,#50449,#50450,#50451,#50452,#50453,#50454,#50455,#50456,
#50457,#50458,#50459,#50460,#50461,#50462,#50463,#50464,#50465),
 .UNSPECIFIED.,.F.,.F.,(4,3,3,3,3,3,3,3,4),(-52.0008580378518,-51.946406269438,
-50.9474369181027,-49.9484675667673,-48.949498215432,-47.9505288640967,
-46.9515595127613,-45.952590161426,-45.7176727306722),.UNSPECIFIED.);
#812=B_SPLINE_CURVE_WITH_KNOTS('',3,(#50466,#50467,#50468,#50469,#50470,
#50471,#50472,#50473,#50474,#50475,#50476,#50477,#50478,#50479,#50480,#50481,
#50482,#50483,#50484,#50485,#50486,#50487,#50488,#50489,#50490),
 .UNSPECIFIED.,.F.,.F.,(4,3,3,3,3,3,3,3,4),(42.7427228936713,42.9556821074199,
43.9546514587553,44.9536208100906,45.9525901614259,46.9515595127613,47.9505288640966,
48.949498215432,49.0259082008509),.UNSPECIFIED.);
#813=B_SPLINE_CURVE_WITH_KNOTS('',3,(#50495,#50496,#50497,#50498,#50499,
#50500,#50501,#50502,#50503,#50504,#50505,#50506,#50507,#50508,#50509,#50510,
#50511,#50512,#50513,#50514,#50515,#50516),.UNSPECIFIED.,.F.,.F.,(4,3,3,
3,3,3,3,4),(-58.2840433450314,-57.9402223774501,-56.9412530261148,-55.9422836747794,
-54.9433143234441,-53.9443449721087,-52.9453756207734,-52.0008580378518),
 .UNSPECIFIED.);
#814=B_SPLINE_CURVE_WITH_KNOTS('',3,(#50517,#50518,#50519,#50520,#50521,
#50522,#50523,#50524,#50525,#50526,#50527,#50528,#50529,#50530,#50531,#50532,
#50533,#50534,#50535,#50536,#50537,#50538),.UNSPECIFIED.,.F.,.F.,(4,3,3,
3,3,3,3,4),(49.0259082008509,49.9484675667673,50.9474369181027,51.946406269438,
52.9453756207734,53.9443449721087,54.9433143234441,55.3090935080305),
 .UNSPECIFIED.);
#815=B_SPLINE_CURVE_WITH_KNOTS('',3,(#50543,#50544,#50545,#50546,#50547,
#50548,#50549,#50550,#50551,#50552,#50553,#50554,#50555,#50556,#50557,#50558,
#50559,#50560,#50561,#50562,#50563,#50564),.UNSPECIFIED.,.F.,.F.,(4,3,3,
3,3,3,3,4),(-64.567228652211,-63.9340384854622,-62.9350691341269,-61.9360997827915,
-60.9371304314562,-59.9381610801208,-58.9391917287855,-58.2840433450314),
 .UNSPECIFIED.);
#816=B_SPLINE_CURVE_WITH_KNOTS('',3,(#50565,#50566,#50567,#50568,#50569,
#50570,#50571,#50572,#50573,#50574,#50575,#50576,#50577,#50578,#50579,#50580,
#50581,#50582,#50583,#50584,#50585,#50586),.UNSPECIFIED.,.F.,.F.,(4,3,3,
3,3,3,3,4),(55.3090935080305,55.9422836747794,56.9412530261148,57.9402223774501,
58.9391917287854,59.9381610801208,60.9371304314561,61.5922788152101),
 .UNSPECIFIED.);
#817=B_SPLINE_CURVE_WITH_KNOTS('',3,(#50591,#50592,#50593,#50594,#50595,
#50596,#50597,#50598,#50599,#50600,#50601,#50602,#50603,#50604,#50605,#50606,
#50607,#50608,#50609,#50610,#50611,#50612),.UNSPECIFIED.,.F.,.F.,(4,3,3,
3,3,3,3,4),(-70.8504139593906,-69.9278545934743,-68.9288852421389,-67.9299158908036,
-66.9309465394682,-65.9319771881329,-64.9330078367975,-64.567228652211),
 .UNSPECIFIED.);
#818=B_SPLINE_CURVE_WITH_KNOTS('',3,(#50613,#50614,#50615,#50616,#50617,
#50618,#50619,#50620,#50621,#50622,#50623,#50624,#50625,#50626,#50627,#50628,
#50629,#50630,#50631,#50632,#50633,#50634),.UNSPECIFIED.,.F.,.F.,(4,3,3,
3,3,3,3,4),(61.5922788152101,61.9360997827915,62.9350691341268,63.9340384854622,
64.9330078367975,65.9319771881329,66.9309465394682,67.8754641223897),
 .UNSPECIFIED.);
#819=B_SPLINE_CURVE_WITH_KNOTS('',3,(#50639,#50640,#50641,#50642,#50643,
#50644,#50645,#50646,#50647,#50648,#50649,#50650,#50651,#50652,#50653,#50654,
#50655,#50656,#50657,#50658,#50659,#50660,#50661,#50662,#50663),
 .UNSPECIFIED.,.F.,.F.,(4,3,3,3,3,3,3,3,4),(-77.1335992665702,-76.9206400528217,
-75.9216707014863,-74.922701350151,-73.9237319988157,-72.9247626474803,
-71.925793296145,-70.9268239448096,-70.8504139593906),.UNSPECIFIED.);
#820=B_SPLINE_CURVE_WITH_KNOTS('',3,(#50664,#50665,#50666,#50667,#50668,
#50669,#50670,#50671,#50672,#50673,#50674,#50675,#50676,#50677,#50678,#50679,
#50680,#50681,#50682,#50683,#50684,#50685,#50686,#50687,#50688),
 .UNSPECIFIED.,.F.,.F.,(4,3,3,3,3,3,3,3,4),(67.8754641223897,67.9299158908036,
68.9288852421389,69.9278545934743,70.9268239448096,71.9257932961449,72.9247626474803,
73.9237319988156,74.1586494295693),.UNSPECIFIED.);
#821=B_SPLINE_CURVE_WITH_KNOTS('',3,(#50693,#50694,#50695,#50696,#50697,
#50698,#50699,#50700,#50701,#50702,#50703,#50704,#50705,#50706,#50707,#50708,
#50709,#50710,#50711,#50712,#50713,#50714),.UNSPECIFIED.,.F.,.F.,(4,3,3,
3,3,3,3,4),(-83.4167845737498,-82.9144561608338,-81.9154868094984,-80.9165174581631,
-79.9175481068278,-78.9185787554924,-77.9196094041571,-77.1335992665702),
 .UNSPECIFIED.);
#822=B_SPLINE_CURVE_WITH_KNOTS('',3,(#50715,#50716,#50717,#50718,#50719,
#50720,#50721,#50722,#50723,#50724,#50725,#50726,#50727,#50728,#50729,#50730,
#50731,#50732,#50733,#50734,#50735,#50736),.UNSPECIFIED.,.F.,.F.,(4,3,3,
3,3,3,3,4),(74.1586494295693,74.922701350151,75.9216707014863,76.9206400528217,
77.919609404157,78.9185787554924,79.9175481068277,80.4418347367489),
 .UNSPECIFIED.);
#823=B_SPLINE_CURVE_WITH_KNOTS('',3,(#50741,#50742,#50743,#50744,#50745,
#50746,#50747,#50748,#50749,#50750,#50751,#50752,#50753,#50754,#50755,#50756,
#50757,#50758,#50759,#50760,#50761,#50762),.UNSPECIFIED.,.F.,.F.,(4,3,3,
3,3,3,3,4),(-89.6999698809294,-88.9082722688459,-87.9093029175105,-86.9103335661752,
-85.9113642148398,-84.9123948635045,-83.9134255121691,-83.4167845737498),
 .UNSPECIFIED.);
#824=B_SPLINE_CURVE_WITH_KNOTS('',3,(#50763,#50764,#50765,#50766,#50767,
#50768,#50769,#50770,#50771,#50772,#50773,#50774,#50775,#50776,#50777,#50778,
#50779,#50780,#50781,#50782,#50783,#50784),.UNSPECIFIED.,.F.,.F.,(4,3,3,
3,3,3,3,4),(80.4418347367489,80.9165174581631,81.9154868094984,82.9144561608338,
83.9134255121691,84.9123948635045,85.9113642148398,86.7250200439285),
 .UNSPECIFIED.);
#825=B_SPLINE_CURVE_WITH_KNOTS('',3,(#50789,#50790,#50791,#50792,#50793,
#50794,#50795,#50796,#50797,#50798,#50799,#50800,#50801,#50802,#50803,#50804,
#50805,#50806,#50807,#50808,#50809,#50810,#50811,#50812,#50813),
 .UNSPECIFIED.,.F.,.F.,(4,3,3,3,3,3,3,3,4),(-95.983155188109,-95.9010577281933,
-94.902088376858,-93.9031190255226,-92.9041496741873,-91.9051803228519,
-90.9062109715166,-89.9072416201812,-89.6999698809294),.UNSPECIFIED.);
#826=B_SPLINE_CURVE_WITH_KNOTS('',3,(#50814,#50815,#50816,#50817,#50818,
#50819,#50820,#50821,#50822,#50823,#50824,#50825,#50826,#50827,#50828,#50829,
#50830,#50831,#50832,#50833,#50834,#50835,#50836,#50837,#50838),
 .UNSPECIFIED.,.F.,.F.,(4,3,3,3,3,3,3,3,4),(86.7250200439285,86.9103335661752,
87.9093029175105,88.9082722688459,89.9072416201812,90.9062109715166,91.9051803228519,
92.9041496741873,93.0082053511081),.UNSPECIFIED.);
#827=B_SPLINE_CURVE_WITH_KNOTS('',3,(#50843,#50844,#50845,#50846,#50847,
#50848,#50849,#50850,#50851,#50852,#50853,#50854,#50855,#50856,#50857,#50858,
#50859,#50860,#50861,#50862,#50863,#50864),.UNSPECIFIED.,.F.,.F.,(4,3,3,
3,3,3,3,4),(-102.266340495289,-101.894873836205,-100.89590448487,-99.8969351335347,
-98.8979657821993,-97.898996430864,-96.9000270795287,-95.983155188109),
 .UNSPECIFIED.);
#828=B_SPLINE_CURVE_WITH_KNOTS('',3,(#50865,#50866,#50867,#50868,#50869,
#50870,#50871,#50872,#50873,#50874,#50875,#50876,#50877,#50878,#50879,#50880,
#50881,#50882,#50883,#50884,#50885,#50886),.UNSPECIFIED.,.F.,.F.,(4,3,3,
3,3,3,3,4),(93.0082053511081,93.9031190255226,94.9020883768579,95.9010577281933,
96.9000270795286,97.8989964308639,98.8979657821993,99.2913906582877),
 .UNSPECIFIED.);
#829=B_SPLINE_CURVE_WITH_KNOTS('',3,(#50891,#50892,#50893,#50894,#50895,
#50896,#50897,#50898,#50899,#50900,#50901,#50902,#50903,#50904,#50905,#50906,
#50907,#50908,#50909,#50910,#50911,#50912),.UNSPECIFIED.,.F.,.F.,(4,3,3,
3,3,3,3,4),(-108.549525802468,-107.888689944217,-106.889720592882,-105.890751241547,
-104.891781890211,-103.892812538876,-102.893843187541,-102.266340495289),
 .UNSPECIFIED.);
#830=B_SPLINE_CURVE_WITH_KNOTS('',3,(#50913,#50914,#50915,#50916,#50917,
#50918,#50919,#50920,#50921,#50922,#50923,#50924,#50925,#50926,#50927,#50928,
#50929,#50930,#50931,#50932,#50933,#50934),.UNSPECIFIED.,.F.,.F.,(4,3,3,
3,3,3,3,4),(99.2913906582877,99.8969351335346,100.89590448487,101.894873836205,
102.893843187541,103.892812538876,104.891781890211,105.574575965467),
 .UNSPECIFIED.);
#831=B_SPLINE_CURVE_WITH_KNOTS('',3,(#50939,#50940,#50941,#50942,#50943,
#50944,#50945,#50946,#50947,#50948,#50949,#50950,#50951,#50952,#50953,#50954,
#50955,#50956,#50957,#50958,#50959,#50960),.UNSPECIFIED.,.F.,.F.,(4,3,3,
3,3,3,3,4),(-114.832711109648,-113.88250605223,-112.883536700894,-111.884567349559,
-110.885597998224,-109.886628646888,-108.887659295553,-108.549525802468),
 .UNSPECIFIED.);
#832=B_SPLINE_CURVE_WITH_KNOTS('',3,(#50961,#50962,#50963,#50964,#50965,
#50966,#50967,#50968,#50969,#50970,#50971,#50972,#50973,#50974,#50975,#50976,
#50977,#50978,#50979,#50980,#50981,#50982),.UNSPECIFIED.,.F.,.F.,(4,3,3,
3,3,3,3,4),(105.574575965467,105.890751241547,106.889720592882,107.888689944217,
108.887659295553,109.886628646888,110.885597998223,111.857761272647),
 .UNSPECIFIED.);
#833=B_SPLINE_CURVE_WITH_KNOTS('',3,(#50988,#50989,#50990,#50991,#50992,
#50993,#50994),.UNSPECIFIED.,.F.,.F.,(4,1,1,1,4),(128.805298797182,128.854063091099,
129.853032442434,130.852001793769,131.782312197151),.UNSPECIFIED.);
#834=B_SPLINE_CURVE_WITH_KNOTS('',3,(#50997,#50998,#50999,#51000,#51001),
 .UNSPECIFIED.,.F.,.F.,(4,1,4),(128.805298797182,129.541705026261,130.540674377597),
 .UNSPECIFIED.);
#835=B_SPLINE_CURVE_WITH_KNOTS('',3,(#51006,#51007,#51008,#51009,#51010,
#51011,#51012,#51013,#51014,#51015),.UNSPECIFIED.,.F.,.F.,(4,1,1,1,1,1,
1,4),(122.522113490002,122.860246983087,123.859216334422,124.858185685757,
125.857155037093,126.856124388428,127.855093739763,128.805298797182),
 .UNSPECIFIED.);
#836=B_SPLINE_CURVE_WITH_KNOTS('',3,(#51016,#51017,#51018,#51019,#51020,
#51021,#51022,#51023,#51024,#51025,#51026),.UNSPECIFIED.,.F.,.F.,(4,1,1,
1,1,1,1,1,4),(122.522113490002,122.548919566914,123.547888918249,124.546858269584,
125.54582762092,126.544796972255,127.54376632359,128.542735674926,128.805298797182),
 .UNSPECIFIED.);
#837=B_SPLINE_CURVE_WITH_KNOTS('',3,(#51031,#51032,#51033,#51034,#51035,
#51036,#51037,#51038,#51039,#51040),.UNSPECIFIED.,.F.,.F.,(4,1,1,1,1,1,
1,4),(116.238928182822,116.866430875074,117.86540022641,118.864369577745,
119.863338929081,120.862308280416,121.861277631751,122.522113490002),
 .UNSPECIFIED.);
#838=B_SPLINE_CURVE_WITH_KNOTS('',3,(#51041,#51042,#51043,#51044,#51045,
#51046,#51047,#51048,#51049,#51050),.UNSPECIFIED.,.F.,.F.,(4,1,1,1,1,1,
1,4),(116.238928182822,116.555103458902,117.554072810237,118.553042161572,
119.552011512908,120.550980864243,121.549950215578,122.522113490002),
 .UNSPECIFIED.);
#839=B_SPLINE_CURVE_WITH_KNOTS('',3,(#51055,#51056,#51057,#51058,#51059,
#51060,#51061,#51062,#51063,#51064),.UNSPECIFIED.,.F.,.F.,(4,1,1,1,1,1,
1,4),(109.955742875643,110.872614767062,111.871584118398,112.870553469733,
113.869522821068,114.868492172404,115.867461523739,116.238928182822),
 .UNSPECIFIED.);
#840=B_SPLINE_CURVE_WITH_KNOTS('',3,(#51065,#51066,#51067,#51068,#51069,
#51070,#51071,#51072,#51073,#51074),.UNSPECIFIED.,.F.,.F.,(4,1,1,1,1,1,
1,4),(109.955742875643,110.56128735089,111.560256702225,112.55922605356,
113.558195404896,114.557164756231,115.556134107566,116.238928182822),
 .UNSPECIFIED.);
#841=B_SPLINE_CURVE_WITH_KNOTS('',3,(#51079,#51080,#51081,#51082,#51083,
#51084,#51085,#51086,#51087,#51088,#51089),.UNSPECIFIED.,.F.,.F.,(4,1,1,
1,1,1,1,1,4),(103.672557568463,103.879829307715,104.87879865905,105.877768010386,
106.876737361721,107.875706713056,108.874676064392,109.873645415727,109.955742875643),
 .UNSPECIFIED.);
#842=B_SPLINE_CURVE_WITH_KNOTS('',3,(#51090,#51091,#51092,#51093,#51094,
#51095,#51096,#51097,#51098,#51099),.UNSPECIFIED.,.F.,.F.,(4,1,1,1,1,1,
1,4),(103.672557568463,104.567471242878,105.566440594213,106.565409945548,
107.564379296884,108.563348648219,109.562317999554,109.955742875643),
 .UNSPECIFIED.);
#843=B_SPLINE_CURVE_WITH_KNOTS('',3,(#51104,#51105,#51106,#51107,#51108,
#51109,#51110,#51111,#51112,#51113),.UNSPECIFIED.,.F.,.F.,(4,1,1,1,1,1,
1,4),(97.3893722612835,97.8860131997029,98.8849825510382,99.8839519023736,
100.882921253709,101.881890605044,102.88085995638,103.672557568463),
 .UNSPECIFIED.);
#844=B_SPLINE_CURVE_WITH_KNOTS('',3,(#51114,#51115,#51116,#51117,#51118,
#51119,#51120,#51121,#51122,#51123,#51124),.UNSPECIFIED.,.F.,.F.,(4,1,1,
1,1,1,1,1,4),(97.3893722612835,97.5746857835301,98.5736551348654,99.5726244862008,
100.571593837536,101.570563188871,102.569532540207,103.568501891542,103.672557568463),
 .UNSPECIFIED.);
#845=B_SPLINE_CURVE_WITH_KNOTS('',3,(#51129,#51130,#51131,#51132,#51133,
#51134,#51135,#51136,#51137,#51138),.UNSPECIFIED.,.F.,.F.,(4,1,1,1,1,1,
1,4),(91.106186954104,91.8921970916908,92.8911664430261,93.8901357943615,
94.8891051456968,95.8880744970322,96.8870438483675,97.3893722612835),
 .UNSPECIFIED.);
#846=B_SPLINE_CURVE_WITH_KNOTS('',3,(#51139,#51140,#51141,#51142,#51143,
#51144,#51145,#51146,#51147,#51148),.UNSPECIFIED.,.F.,.F.,(4,1,1,1,1,1,
1,4),(91.1061869541039,91.580869675518,92.5798390268534,93.5788083781887,
94.5777777295241,95.5767470808594,96.5757164321948,97.3893722612835),
 .UNSPECIFIED.);
#847=B_SPLINE_CURVE_WITH_KNOTS('',3,(#51153,#51154,#51155,#51156,#51157,
#51158,#51159,#51160,#51161,#51162,#51163),.UNSPECIFIED.,.F.,.F.,(4,1,1,
1,1,1,1,1,4),(84.8230016469244,84.8994116323434,85.8983809836787,86.8973503350141,
87.8963196863494,88.8952890376847,89.8942583890201,90.8932277403554,91.106186954104),
 .UNSPECIFIED.);
#848=B_SPLINE_CURVE_WITH_KNOTS('',3,(#51164,#51165,#51166,#51167,#51168,
#51169,#51170,#51171,#51172,#51173),.UNSPECIFIED.,.F.,.F.,(4,1,1,1,1,1,
1,4),(84.8230016469243,85.5870535675059,86.5860229188413,87.5849922701766,
88.583961621512,89.5829309728473,90.5819003241827,91.1061869541039),
 .UNSPECIFIED.);
#849=B_SPLINE_CURVE_WITH_KNOTS('',3,(#51178,#51179,#51180,#51181,#51182,
#51183,#51184,#51185,#51186,#51187),.UNSPECIFIED.,.F.,.F.,(4,1,1,1,1,1,
1,4),(78.5398163397448,78.9055955243313,79.9045648756666,80.903534227002,
81.9025035783373,82.9014729296727,83.900442281008,84.8230016469244),
 .UNSPECIFIED.);
#850=B_SPLINE_CURVE_WITH_KNOTS('',3,(#51188,#51189,#51190,#51191,#51192,
#51193,#51194,#51195,#51196,#51197,#51198),.UNSPECIFIED.,.F.,.F.,(4,1,1,
1,1,1,1,1,4),(78.5398163397448,78.5942681081585,79.5932374594938,80.5922068108292,
81.5911761621645,82.5901455134999,83.5891148648352,84.5880842161706,84.8230016469243),
 .UNSPECIFIED.);
#851=B_SPLINE_CURVE_WITH_KNOTS('',3,(#51203,#51204,#51205,#51206,#51207,
#51208,#51209,#51210,#51211,#51212),.UNSPECIFIED.,.F.,.F.,(4,1,1,1,1,1,
1,4),(72.2566310325652,72.9117794163192,73.9107487676546,74.9097181189899,
75.9086874703252,76.9076568216606,77.9066261729959,78.5398163397448),
 .UNSPECIFIED.);
#852=B_SPLINE_CURVE_WITH_KNOTS('',3,(#51213,#51214,#51215,#51216,#51217,
#51218,#51219,#51220,#51221,#51222),.UNSPECIFIED.,.F.,.F.,(4,1,1,1,1,1,
1,4),(72.2566310325652,72.6004520001464,73.5994213514818,74.5983907028171,
75.5973600541525,76.5963294054878,77.5952987568232,78.5398163397448),
 .UNSPECIFIED.);
#853=B_SPLINE_CURVE_WITH_KNOTS('',3,(#51227,#51228,#51229,#51230,#51231,
#51232,#51233,#51234,#51235,#51236),.UNSPECIFIED.,.F.,.F.,(4,1,1,1,1,1,
1,4),(65.9734457253856,66.9179633083071,67.9169326596425,68.9159020109778,
69.9148713623132,70.9138407136485,71.9128100649839,72.2566310325652),
 .UNSPECIFIED.);
#854=B_SPLINE_CURVE_WITH_KNOTS('',3,(#51237,#51238,#51239,#51240,#51241,
#51242,#51243,#51244,#51245,#51246),.UNSPECIFIED.,.F.,.F.,(4,1,1,1,1,1,
1,4),(65.9734457253856,66.6066358921343,67.6056052434697,68.604574594805,
69.6035439461404,70.6025132974757,71.6014826488111,72.2566310325652),
 .UNSPECIFIED.);
#855=B_SPLINE_CURVE_WITH_KNOTS('',3,(#51251,#51252,#51253,#51254,#51255,
#51256,#51257,#51258,#51259,#51260,#51261),.UNSPECIFIED.,.F.,.F.,(4,1,1,
1,1,1,1,1,4),(59.690260418206,59.9251778489597,60.924147200295,61.9231165516304,
62.9220859029657,63.9210552543011,64.9200246056364,65.9189939569718,65.9734457253856),
 .UNSPECIFIED.);
#856=B_SPLINE_CURVE_WITH_KNOTS('',3,(#51262,#51263,#51264,#51265,#51266,
#51267,#51268,#51269,#51270,#51271),.UNSPECIFIED.,.F.,.F.,(4,1,1,1,1,1,
1,4),(59.690260418206,60.6128197841223,61.6117891354576,62.610758486793,
63.6097278381283,64.6086971894637,65.607666540799,65.9734457253856),
 .UNSPECIFIED.);
#857=B_SPLINE_CURVE_WITH_KNOTS('',3,(#51276,#51277,#51278,#51279,#51280,
#51281,#51282,#51283,#51284,#51285),.UNSPECIFIED.,.F.,.F.,(4,1,1,1,1,1,
1,4),(53.4070751110264,53.9313617409476,54.930331092283,55.9293004436183,
56.9282697949536,57.927239146289,58.9262084976243,59.690260418206),
 .UNSPECIFIED.);
#858=B_SPLINE_CURVE_WITH_KNOTS('',3,(#51286,#51287,#51288,#51289,#51290,
#51291,#51292,#51293,#51294,#51295,#51296),.UNSPECIFIED.,.F.,.F.,(4,1,1,
1,1,1,1,1,4),(53.4070751110264,53.6200343247748,54.6190036761102,55.6179730274455,
56.6169423787809,57.6159117301162,58.6148810814516,59.6138504327869,59.690260418206),
 .UNSPECIFIED.);
#859=B_SPLINE_CURVE_WITH_KNOTS('',3,(#51301,#51302,#51303,#51304,#51305,
#51306,#51307,#51308,#51309,#51310),.UNSPECIFIED.,.F.,.F.,(4,1,1,1,1,1,
1,4),(47.1238898038468,47.9375456329355,48.9365149842709,49.9354843356062,
50.9344536869416,51.9334230382769,52.9323923896123,53.4070751110264),
 .UNSPECIFIED.);
#860=B_SPLINE_CURVE_WITH_KNOTS('',3,(#51311,#51312,#51313,#51314,#51315,
#51316,#51317,#51318,#51319,#51320),.UNSPECIFIED.,.F.,.F.,(4,1,1,1,1,1,
1,4),(47.1238898038468,47.6262182167628,48.6251875680981,49.6241569194335,
50.6231262707688,51.6220956221041,52.6210649734395,53.4070751110264),
 .UNSPECIFIED.);
#861=B_SPLINE_CURVE_WITH_KNOTS('',3,(#51325,#51326,#51327,#51328,#51329,
#51330,#51331,#51332,#51333,#51334,#51335),.UNSPECIFIED.,.F.,.F.,(4,1,1,
1,1,1,1,1,4),(40.8407044966672,40.9447601735881,41.9437295249234,42.9426988762588,
43.9416682275941,44.9406375789295,45.9396069302648,46.9385762816002,47.1238898038468),
 .UNSPECIFIED.);
#862=B_SPLINE_CURVE_WITH_KNOTS('',3,(#51336,#51337,#51338,#51339,#51340,
#51341,#51342,#51343,#51344,#51345),.UNSPECIFIED.,.F.,.F.,(4,1,1,1,1,1,
1,4),(40.8407044966672,41.6324021087507,42.631371460086,43.6303408114214,
44.6293101627567,45.6282795140921,46.6272488654274,47.1238898038468),
 .UNSPECIFIED.);
#863=B_SPLINE_CURVE_WITH_KNOTS('',3,(#51350,#51351,#51352,#51353,#51354,
#51355,#51356,#51357,#51358,#51359),.UNSPECIFIED.,.F.,.F.,(4,1,1,1,1,1,
1,4),(34.5575191894876,34.950944065576,35.9499134169114,36.9488827682467,
37.9478521195821,38.9468214709174,39.9457908222528,40.8407044966672),
 .UNSPECIFIED.);
#864=B_SPLINE_CURVE_WITH_KNOTS('',3,(#51360,#51361,#51362,#51363,#51364,
#51365,#51366,#51367,#51368,#51369,#51370),.UNSPECIFIED.,.F.,.F.,(4,1,1,
1,1,1,1,1,4),(34.5575191894876,34.6396166494033,35.6385860007386,36.6375553520739,
37.6365247034093,38.6354940547446,39.63446340608,40.6334327574153,40.8407044966672),
 .UNSPECIFIED.);
#865=B_SPLINE_CURVE_WITH_KNOTS('',3,(#51375,#51376,#51377,#51378,#51379,
#51380,#51381,#51382,#51383,#51384),.UNSPECIFIED.,.F.,.F.,(4,1,1,1,1,1,
1,4),(28.2743338823081,28.9571279575639,29.9560973088993,30.9550666602346,
31.95403601157,32.9530053629053,33.9519747142407,34.5575191894876),
 .UNSPECIFIED.);
#866=B_SPLINE_CURVE_WITH_KNOTS('',3,(#51385,#51386,#51387,#51388,#51389,
#51390,#51391,#51392,#51393,#51394),.UNSPECIFIED.,.F.,.F.,(4,1,1,1,1,1,
1,4),(28.274333882308,28.6458005413912,29.6447698927265,30.6437392440619,
31.6427085953972,32.6416779467326,33.6406472980679,34.5575191894876),
 .UNSPECIFIED.);
#867=B_SPLINE_CURVE_WITH_KNOTS('',3,(#51399,#51400,#51401,#51402,#51403,
#51404,#51405,#51406,#51407,#51408),.UNSPECIFIED.,.F.,.F.,(4,1,1,1,1,1,
1,4),(21.9911485751285,22.9633118495519,23.9622812008872,24.9612505522226,
25.9602199035579,26.9591892548932,27.9581586062286,28.2743338823081),
 .UNSPECIFIED.);
#868=B_SPLINE_CURVE_WITH_KNOTS('',3,(#51409,#51410,#51411,#51412,#51413,
#51414,#51415,#51416,#51417,#51418),.UNSPECIFIED.,.F.,.F.,(4,1,1,1,1,1,
1,4),(21.9911485751284,22.6519844333791,23.6509537847144,24.6499231360498,
25.6488924873851,26.6478618387205,27.6468311900558,28.274333882308),
 .UNSPECIFIED.);
#869=B_SPLINE_CURVE_WITH_KNOTS('',3,(#51423,#51424,#51425,#51426,#51427,
#51428,#51429,#51430,#51431,#51432,#51433),.UNSPECIFIED.,.F.,.F.,(4,1,1,
1,1,1,1,1,4),(15.7079632679489,15.9705263902044,16.9694957415398,17.9684650928751,
18.9674344442105,19.9664037955458,20.9653731468812,21.9643424982165,21.9911485751285),
 .UNSPECIFIED.);
#870=B_SPLINE_CURVE_WITH_KNOTS('',3,(#51434,#51435,#51436,#51437,#51438,
#51439,#51440,#51441,#51442,#51443),.UNSPECIFIED.,.F.,.F.,(4,1,1,1,1,1,
1,4),(15.7079632679489,16.658168325367,17.6571376767024,18.6561070280377,
19.6550763793731,20.6540457307084,21.6530150820438,21.9911485751284),
 .UNSPECIFIED.);
#871=B_SPLINE_CURVE_WITH_KNOTS('',3,(#51446,#51447,#51448,#51449,#51450,
#51451,#51452,#51453,#51454,#51455,#51456,#51457,#51458,#51459,#51460,#51461,
#51462,#51463,#51464,#51465,#51466,#51467,#51468,#51469,#51470,#51471,#51472,
#51473,#51474,#51475,#51476,#51477,#51478,#51479,#51480,#51481,#51482,#51483,
#51484,#51485,#51486,#51487,#51488,#51489,#51490,#51491,#51492,#51493,#51494,
#51495,#51496,#51497,#51498,#51499,#51500,#51501,#51502,#51503),
 .UNSPECIFIED.,.F.,.F.,(4,3,3,3,3,3,3,3,3,3,3,3,3,3,3,3,3,3,3,4),(-0.463803050843755,
-0.449907398794694,-0.418031857702381,-0.400337768208314,-0.372896888686324,
-0.358221213465045,-0.345421670140428,-0.303252356142987,-0.273478234693713,
-0.262474993370258,-0.235827691279064,-0.206349229869181,-0.190332836617136,
-0.175380554584644,-0.131535415938483,-0.108450622298565,-0.0944456675460115,
-0.0816634290814505,-0.0359771892759535,0.),.UNSPECIFIED.);
#872=B_SPLINE_CURVE_WITH_KNOTS('',3,(#51508,#51509,#51510,#51511,#51512,
#51513,#51514,#51515,#51516,#51517,#51518,#51519,#51520,#51521,#51522,#51523,
#51524,#51525,#51526,#51527,#51528,#51529,#51530,#51531,#51532,#51533,#51534,
#51535,#51536,#51537,#51538,#51539,#51540,#51541,#51542,#51543,#51544,#51545,
#51546,#51547,#51548,#51549,#51550,#51551,#51552,#51553,#51554,#51555,#51556,
#51557,#51558,#51559,#51560,#51561,#51562,#51563,#51564,#51565),
 .UNSPECIFIED.,.F.,.F.,(4,3,3,3,3,3,3,3,3,3,3,3,3,3,3,3,3,3,3,4),(-0.461788964899843,
-0.444996338453757,-0.413305262598462,-0.398720954647667,-0.383442254293799,
-0.356179300230217,-0.336984284953546,-0.32270401518387,-0.279139696516272,
-0.260144406012141,-0.247531499300344,-0.235347705780398,-0.211863769192623,
-0.169080986415294,-0.153240163194338,-0.114930122395753,-0.0804234717365801,
-0.0679412143129863,-0.0289558983189821,0.),.UNSPECIFIED.);
#873=B_SPLINE_CURVE_WITH_KNOTS('',3,(#52058,#52059,#52060,#52061,#52062,
#52063,#52064,#52065,#52066,#52067,#52068,#52069,#52070,#52071,#52072,#52073,
#52074,#52075,#52076,#52077,#52078,#52079),.UNSPECIFIED.,.F.,.F.,(4,3,3,
3,3,3,3,4),(111.857761272647,111.884567349559,112.883536700894,113.88250605223,
114.881475403565,115.8804447549,116.879414106236,117.809724509617),
 .UNSPECIFIED.);
#874=B_SPLINE_CURVE_WITH_KNOTS('',3,(#52081,#52082,#52083,#52084,#52085,
#52086,#52087,#52088,#52089,#52090,#52091,#52092,#52093,#52094,#52095,#52096,
#52097,#52098,#52099,#52100,#52101,#52102,#52103,#52104,#52105,#52106,#52107,
#52108,#52109,#52110,#52111,#52112,#52113,#52114,#52115,#52116,#52117,#52118,
#52119,#52120,#52121,#52122,#52123,#52124,#52125,#52126,#52127,#52128,#52129,
#52130,#52131,#52132,#52133,#52134,#52135,#52136,#52137,#52138),
 .UNSPECIFIED.,.F.,.F.,(4,3,3,3,3,3,3,3,3,3,3,3,3,3,3,3,3,3,3,4),(-0.46380305084371,
-0.449907398794639,-0.418031858716818,-0.400337770850382,-0.372897098979116,
-0.358225636990301,-0.345427365771652,-0.303258135833885,-0.273481221790439,
-0.262481185322834,-0.235827691279055,-0.206349229869174,-0.190332831578201,
-0.175380551365677,-0.131535413524257,-0.108450616220395,-0.09444564303348,
-0.0816634226200209,-0.0359771748293766,0.),.UNSPECIFIED.);
#875=B_SPLINE_CURVE_WITH_KNOTS('',3,(#52139,#52140,#52141,#52142,#52143,
#52144,#52145),.UNSPECIFIED.,.F.,.F.,(4,1,1,1,4),(12.7309498679793,13.661260271361,
14.6602296226963,15.6591989740317,15.7079632679489),.UNSPECIFIED.);
#876=B_SPLINE_CURVE_WITH_KNOTS('',3,(#52148,#52149,#52150,#52151,#52152,
#52153,#52154,#52155,#52156,#52157,#52158,#52159,#52160,#52161,#52162,#52163,
#52164,#52165,#52166,#52167,#52168,#52169,#52170,#52171,#52172,#52173,#52174,
#52175,#52176,#52177,#52178,#52179,#52180,#52181,#52182,#52183,#52184,#52185,
#52186,#52187,#52188,#52189,#52190,#52191,#52192,#52193,#52194,#52195,#52196,
#52197,#52198,#52199,#52200,#52201,#52202,#52203,#52204,#52205),
 .UNSPECIFIED.,.F.,.F.,(4,3,3,3,3,3,3,3,3,3,3,3,3,3,3,3,3,3,3,4),(-0.461788964899765,
-0.444996338453673,-0.413305257846947,-0.398720941271075,-0.38344224790616,
-0.356179268364253,-0.33698399566128,-0.32270394349123,-0.279139618915834,
-0.260144344795765,-0.247531524843875,-0.235347708885629,-0.211863769192592,
-0.16908098381302,-0.153240164163327,-0.114930123122496,-0.08042347380898,
-0.0679412157174702,-0.028955921834972,0.),.UNSPECIFIED.);
#877=B_SPLINE_CURVE_WITH_KNOTS('',3,(#52208,#52209,#52210,#52211,#52212),
 .UNSPECIFIED.,.F.,.F.,(4,1,4),(13.9725876875337,14.9715570388691,15.7079632679489),
 .UNSPECIFIED.);
#878=B_SPLINE_CURVE_WITH_KNOTS('',3,(#52705,#52706,#52707,#52708,#52709,
#52710,#52711,#52712,#52713,#52714,#52715,#52716,#52717,#52718,#52719,#52720,
#52721,#52722,#52723),.UNSPECIFIED.,.F.,.F.,(4,3,3,3,3,3,4),(-119.876322160242,
-118.877352808906,-117.878383457571,-116.879414106236,-115.8804447549,-114.881475403565,
-114.832711109648),.UNSPECIFIED.);
#879=SHAPE_REPRESENTATION_RELATIONSHIP('SRR','None',#53724,#895);
#880=SHAPE_REPRESENTATION_RELATIONSHIP('SRR','None',#53725,#896);
#881=SHAPE_REPRESENTATION_RELATIONSHIP('SRR','None',#53726,#897);
#882=SHAPE_REPRESENTATION_RELATIONSHIP('SRR','None',#53727,#898);
#883=SHAPE_REPRESENTATION_RELATIONSHIP('SRR','None',#53728,#899);
#884=SHAPE_REPRESENTATION_RELATIONSHIP('SRR','None',#53729,#900);
#885=SHAPE_REPRESENTATION_RELATIONSHIP('SRR','None',#53730,#901);
#886=SHAPE_REPRESENTATION_RELATIONSHIP('SRR','None',#53731,#902);
#887=SHAPE_REPRESENTATION_RELATIONSHIP('SRR','None',#53732,#903);
#888=SHAPE_REPRESENTATION_RELATIONSHIP('SRR','None',#53733,#904);
#889=SHAPE_REPRESENTATION_RELATIONSHIP('SRR','None',#53734,#905);
#890=SHAPE_REPRESENTATION_RELATIONSHIP('SRR','None',#53735,#906);
#891=SHAPE_REPRESENTATION_RELATIONSHIP('SRR','None',#53736,#907);
#892=SHAPE_REPRESENTATION_RELATIONSHIP('SRR','None',#53737,#908);
#893=SHAPE_REPRESENTATION_RELATIONSHIP('SRR','None',#53738,#909);
#894=SHAPE_REPRESENTATION_RELATIONSHIP('SRR','None',#53739,#910);
#895=ADVANCED_BREP_SHAPE_REPRESENTATION('',(#927),#53634);
#896=ADVANCED_BREP_SHAPE_REPRESENTATION('',(#928),#53635);
#897=ADVANCED_BREP_SHAPE_REPRESENTATION('',(#929),#53636);
#898=ADVANCED_BREP_SHAPE_REPRESENTATION('',(#930),#53637);
#899=ADVANCED_BREP_SHAPE_REPRESENTATION('',(#931),#53638);
#900=ADVANCED_BREP_SHAPE_REPRESENTATION('',(#932),#53639);
#901=ADVANCED_BREP_SHAPE_REPRESENTATION('',(#933),#53640);
#902=ADVANCED_BREP_SHAPE_REPRESENTATION('',(#934),#53641);
#903=ADVANCED_BREP_SHAPE_REPRESENTATION('',(#935),#53642);
#904=ADVANCED_BREP_SHAPE_REPRESENTATION('',(#936),#53643);
#905=ADVANCED_BREP_SHAPE_REPRESENTATION('',(#937),#53644);
#906=ADVANCED_BREP_SHAPE_REPRESENTATION('',(#938),#53645);
#907=ADVANCED_BREP_SHAPE_REPRESENTATION('',(#939),#53646);
#908=ADVANCED_BREP_SHAPE_REPRESENTATION('',(#940),#53647);
#909=ADVANCED_BREP_SHAPE_REPRESENTATION('',(#941),#53648);
#910=ADVANCED_BREP_SHAPE_REPRESENTATION('',(#942),#53649);
#911=STYLED_ITEM('',(#53937),#927);
#912=STYLED_ITEM('',(#53944),#928);
#913=STYLED_ITEM('',(#53937),#929);
#914=STYLED_ITEM('',(#53972),#930);
#915=STYLED_ITEM('',(#53944),#931);
#916=STYLED_ITEM('',(#53972),#932);
#917=STYLED_ITEM('',(#53944),#933);
#918=STYLED_ITEM('',(#53951),#934);
#919=STYLED_ITEM('',(#53944),#935);
#920=STYLED_ITEM('',(#53965),#936);
#921=STYLED_ITEM('',(#53951),#937);
#922=STYLED_ITEM('',(#53958),#938);
#923=STYLED_ITEM('',(#53944),#939);
#924=STYLED_ITEM('',(#53965),#940);
#925=STYLED_ITEM('',(#53965),#941);
#926=STYLED_ITEM('',(#53965),#942);
#927=MANIFOLD_SOLID_BREP('Base Flange',#23303);
#928=MANIFOLD_SOLID_BREP('Rear Mirror Cell Plate',#23304);
#929=MANIFOLD_SOLID_BREP('Front Cell Alignment Frame',#23305);
#930=MANIFOLD_SOLID_BREP('Invar Spacing Ring',#23306);
#931=MANIFOLD_SOLID_BREP('Retaining Ring',#23307);
#932=MANIFOLD_SOLID_BREP('SHV Plug',#23308);
#933=MANIFOLD_SOLID_BREP('Mirror Substrate',#23309);
#934=MANIFOLD_SOLID_BREP('PZT Tube',#23310);
#935=MANIFOLD_SOLID_BREP('Gap Sensor',#23311);
#936=MANIFOLD_SOLID_BREP('Gasket',#23312);
#937=MANIFOLD_SOLID_BREP('Clip',#23313);
#938=MANIFOLD_SOLID_BREP('Disc Spring',#23314);
#939=MANIFOLD_SOLID_BREP('Thumb Knob',#23315);
#940=MANIFOLD_SOLID_BREP('ISO_4762_M3x8_A2',#23316);
#941=MANIFOLD_SOLID_BREP('ISO_4762_M3x30_A2',#23317);
#942=MANIFOLD_SOLID_BREP('ISO_4762_M5x16_A2',#23318);
#943=CYLINDRICAL_SURFACE('',#23543,0.6);
#944=CYLINDRICAL_SURFACE('',#23546,0.6);
#945=CYLINDRICAL_SURFACE('',#23599,0.55);
#946=CYLINDRICAL_SURFACE('',#23604,0.55);
#947=CYLINDRICAL_SURFACE('',#23609,0.55);
#948=CYLINDRICAL_SURFACE('',#23614,0.55);
#949=CYLINDRICAL_SURFACE('',#23619,0.5);
#950=CYLINDRICAL_SURFACE('',#23624,0.5);
#951=CYLINDRICAL_SURFACE('',#23629,0.5);
#952=CYLINDRICAL_SURFACE('',#23633,0.275);
#953=CYLINDRICAL_SURFACE('',#23640,0.275);
#954=CYLINDRICAL_SURFACE('',#23647,0.275);
#955=CYLINDRICAL_SURFACE('',#23654,0.33);
#956=CYLINDRICAL_SURFACE('',#23661,0.33);
#957=CYLINDRICAL_SURFACE('',#23668,0.33);
#958=CYLINDRICAL_SURFACE('',#23675,0.33);
#959=CYLINDRICAL_SURFACE('',#23683,0.6);
#960=CYLINDRICAL_SURFACE('',#23684,0.6);
#961=CYLINDRICAL_SURFACE('',#23742,0.6);
#962=CYLINDRICAL_SURFACE('',#23768,3.3);
#963=CYLINDRICAL_SURFACE('',#23773,3.775);
#964=CYLINDRICAL_SURFACE('',#23781,0.17);
#965=CYLINDRICAL_SURFACE('',#23787,0.17);
#966=CYLINDRICAL_SURFACE('',#23793,0.17);
#967=CYLINDRICAL_SURFACE('',#23798,0.405);
#968=CYLINDRICAL_SURFACE('',#23802,0.404999999999999);
#969=CYLINDRICAL_SURFACE('',#23806,0.405);
#970=CYLINDRICAL_SURFACE('',#23818,0.405);
#971=CYLINDRICAL_SURFACE('',#23823,0.255);
#972=CYLINDRICAL_SURFACE('',#23828,0.255);
#973=CYLINDRICAL_SURFACE('',#23833,0.255);
#974=CYLINDRICAL_SURFACE('',#23841,0.155);
#975=CYLINDRICAL_SURFACE('',#23846,0.155);
#976=CYLINDRICAL_SURFACE('',#23851,0.155);
#977=CYLINDRICAL_SURFACE('',#23855,0.6);
#978=CYLINDRICAL_SURFACE('',#23898,0.6);
#979=CYLINDRICAL_SURFACE('',#23901,0.6);
#980=CYLINDRICAL_SURFACE('',#23929,3.775);
#981=CYLINDRICAL_SURFACE('',#23953,3.3);
#982=CYLINDRICAL_SURFACE('',#23963,0.205);
#983=CYLINDRICAL_SURFACE('',#23968,0.205);
#984=CYLINDRICAL_SURFACE('',#23973,0.205);
#985=CYLINDRICAL_SURFACE('',#23980,0.6);
#986=CYLINDRICAL_SURFACE('',#23982,0.6);
#987=CYLINDRICAL_SURFACE('',#23988,4.);
#988=CYLINDRICAL_SURFACE('',#24015,4.8);
#989=CYLINDRICAL_SURFACE('',#24025,0.155);
#990=CYLINDRICAL_SURFACE('',#24030,0.154999999999999);
#991=CYLINDRICAL_SURFACE('',#24035,0.155);
#992=CYLINDRICAL_SURFACE('',#24043,0.17);
#993=CYLINDRICAL_SURFACE('',#24066,0.17);
#994=CYLINDRICAL_SURFACE('',#24072,0.17);
#995=CYLINDRICAL_SURFACE('',#24078,0.170000000000001);
#996=CYLINDRICAL_SURFACE('',#24084,0.17);
#997=CYLINDRICAL_SURFACE('',#24090,0.17);
#998=CYLINDRICAL_SURFACE('',#24096,4.7);
#999=CYLINDRICAL_SURFACE('',#24103,3.3);
#1000=CYLINDRICAL_SURFACE('',#24108,0.3954);
#1001=CYLINDRICAL_SURFACE('',#24111,0.3954);
#1002=CYLINDRICAL_SURFACE('',#24112,0.3954);
#1003=CYLINDRICAL_SURFACE('',#24113,0.3954);
#1004=CYLINDRICAL_SURFACE('',#24114,0.3954);
#1005=CYLINDRICAL_SURFACE('',#24115,0.3954);
#1006=CYLINDRICAL_SURFACE('',#24116,0.3954);
#1007=CYLINDRICAL_SURFACE('',#24117,0.3954);
#1008=CYLINDRICAL_SURFACE('',#24118,0.3954);
#1009=CYLINDRICAL_SURFACE('',#24119,0.3954);
#1010=CYLINDRICAL_SURFACE('',#24120,0.352375);
#1011=CYLINDRICAL_SURFACE('',#24122,0.352375);
#1012=CYLINDRICAL_SURFACE('',#24123,0.352375);
#1013=CYLINDRICAL_SURFACE('',#24124,0.352375);
#1014=CYLINDRICAL_SURFACE('',#24125,0.352375);
#1015=CYLINDRICAL_SURFACE('',#24126,0.352375);
#1016=CYLINDRICAL_SURFACE('',#24127,0.352375);
#1017=CYLINDRICAL_SURFACE('',#24128,0.352375);
#1018=CYLINDRICAL_SURFACE('',#24129,0.352375);
#1019=CYLINDRICAL_SURFACE('',#24130,0.352375);
#1020=CYLINDRICAL_SURFACE('',#24131,0.352375);
#1021=CYLINDRICAL_SURFACE('',#24134,0.352375);
#1022=CYLINDRICAL_SURFACE('',#24135,0.08);
#1023=CYLINDRICAL_SURFACE('',#24138,0.08);
#1024=CYLINDRICAL_SURFACE('',#24141,0.08);
#1025=CYLINDRICAL_SURFACE('',#24144,0.08);
#1026=CYLINDRICAL_SURFACE('',#24293,0.06);
#1027=CYLINDRICAL_SURFACE('',#24301,0.25);
#1028=CYLINDRICAL_SURFACE('',#24303,0.5);
#1029=CYLINDRICAL_SURFACE('',#24308,0.52);
#1030=CYLINDRICAL_SURFACE('',#24330,0.3954);
#1031=CYLINDRICAL_SURFACE('',#24336,3.75);
#1032=CYLINDRICAL_SURFACE('',#24344,0.385);
#1033=CYLINDRICAL_SURFACE('',#24351,0.4);
#1034=CYLINDRICAL_SURFACE('',#24354,0.385);
#1035=CYLINDRICAL_SURFACE('',#24361,0.4);
#1036=CYLINDRICAL_SURFACE('',#24364,0.4);
#1037=CYLINDRICAL_SURFACE('',#24373,0.25);
#1038=CYLINDRICAL_SURFACE('',#24380,0.6);
#1039=CYLINDRICAL_SURFACE('',#24499,0.24);
#1040=CYLINDRICAL_SURFACE('',#24502,0.28);
#1041=CYLINDRICAL_SURFACE('',#24511,0.4);
#1042=CYLINDRICAL_SURFACE('',#24514,0.3);
#1043=CYLINDRICAL_SURFACE('',#24518,0.18);
#1044=CYLINDRICAL_SURFACE('',#24522,3.35);
#1045=CYLINDRICAL_SURFACE('',#24527,3.75);
#1046=CYLINDRICAL_SURFACE('',#24534,0.225000000000001);
#1047=CYLINDRICAL_SURFACE('',#24564,0.2);
#1048=CYLINDRICAL_SURFACE('',#24581,0.2);
#1049=CYLINDRICAL_SURFACE('',#24583,0.35);
#1050=CYLINDRICAL_SURFACE('',#24585,0.35);
#1051=CYLINDRICAL_SURFACE('',#24587,0.21);
#1052=CYLINDRICAL_SURFACE('',#24592,0.4);
#1053=CYLINDRICAL_SURFACE('',#24596,0.1954);
#1054=CYLINDRICAL_SURFACE('',#24600,0.1954);
#1055=CYLINDRICAL_SURFACE('',#24601,0.1954);
#1056=CYLINDRICAL_SURFACE('',#24602,0.1954);
#1057=CYLINDRICAL_SURFACE('',#24603,0.1954);
#1058=CYLINDRICAL_SURFACE('',#24604,0.1954);
#1059=CYLINDRICAL_SURFACE('',#24605,0.1954);
#1060=CYLINDRICAL_SURFACE('',#24606,0.1954);
#1061=CYLINDRICAL_SURFACE('',#24607,0.1954);
#1062=CYLINDRICAL_SURFACE('',#24608,0.1954);
#1063=CYLINDRICAL_SURFACE('',#24609,0.1954);
#1064=CYLINDRICAL_SURFACE('',#24610,0.1954);
#1065=CYLINDRICAL_SURFACE('',#24611,0.1954);
#1066=CYLINDRICAL_SURFACE('',#24612,0.1954);
#1067=CYLINDRICAL_SURFACE('',#24613,0.15555);
#1068=CYLINDRICAL_SURFACE('',#24615,0.15555);
#1069=CYLINDRICAL_SURFACE('',#24616,0.15555);
#1070=CYLINDRICAL_SURFACE('',#24617,0.15555);
#1071=CYLINDRICAL_SURFACE('',#24618,0.15555);
#1072=CYLINDRICAL_SURFACE('',#24619,0.15555);
#1073=CYLINDRICAL_SURFACE('',#24620,0.15555);
#1074=CYLINDRICAL_SURFACE('',#24621,0.15555);
#1075=CYLINDRICAL_SURFACE('',#24622,0.15555);
#1076=CYLINDRICAL_SURFACE('',#24623,0.15555);
#1077=CYLINDRICAL_SURFACE('',#24624,0.15555);
#1078=CYLINDRICAL_SURFACE('',#24625,0.15555);
#1079=CYLINDRICAL_SURFACE('',#24626,0.15555);
#1080=CYLINDRICAL_SURFACE('',#24627,0.15555);
#1081=CYLINDRICAL_SURFACE('',#24628,0.15555);
#1082=CYLINDRICAL_SURFACE('',#24632,0.15555);
#1083=CYLINDRICAL_SURFACE('',#24633,0.1954);
#1084=CYLINDRICAL_SURFACE('',#24790,0.6);
#1085=CYLINDRICAL_SURFACE('',#24796,0.14635);
#1086=CYLINDRICAL_SURFACE('',#24800,0.14635);
#1087=CYLINDRICAL_SURFACE('',#24801,0.14635);
#1088=CYLINDRICAL_SURFACE('',#24802,0.14635);
#1089=CYLINDRICAL_SURFACE('',#24803,0.14635);
#1090=CYLINDRICAL_SURFACE('',#24804,0.14635);
#1091=CYLINDRICAL_SURFACE('',#24805,0.14635);
#1092=CYLINDRICAL_SURFACE('',#24806,0.14635);
#1093=CYLINDRICAL_SURFACE('',#24807,0.14635);
#1094=CYLINDRICAL_SURFACE('',#24808,0.14635);
#1095=CYLINDRICAL_SURFACE('',#24809,0.14635);
#1096=CYLINDRICAL_SURFACE('',#24810,0.14635);
#1097=CYLINDRICAL_SURFACE('',#24811,0.14635);
#1098=CYLINDRICAL_SURFACE('',#24812,0.14635);
#1099=CYLINDRICAL_SURFACE('',#24813,0.117775);
#1100=CYLINDRICAL_SURFACE('',#24815,0.117775);
#1101=CYLINDRICAL_SURFACE('',#24816,0.117775);
#1102=CYLINDRICAL_SURFACE('',#24817,0.117775);
#1103=CYLINDRICAL_SURFACE('',#24818,0.117775);
#1104=CYLINDRICAL_SURFACE('',#24819,0.117775);
#1105=CYLINDRICAL_SURFACE('',#24820,0.117775);
#1106=CYLINDRICAL_SURFACE('',#24821,0.117775);
#1107=CYLINDRICAL_SURFACE('',#24822,0.117775);
#1108=CYLINDRICAL_SURFACE('',#24823,0.117775);
#1109=CYLINDRICAL_SURFACE('',#24824,0.117775);
#1110=CYLINDRICAL_SURFACE('',#24825,0.117775);
#1111=CYLINDRICAL_SURFACE('',#24826,0.117775);
#1112=CYLINDRICAL_SURFACE('',#24827,0.117775);
#1113=CYLINDRICAL_SURFACE('',#24828,0.117775);
#1114=CYLINDRICAL_SURFACE('',#24834,0.117775);
#1115=CYLINDRICAL_SURFACE('',#24976,0.275);
#1116=CYLINDRICAL_SURFACE('',#25032,0.14635);
#1117=CYLINDRICAL_SURFACE('',#25039,0.14635);
#1118=CYLINDRICAL_SURFACE('',#25043,0.14635);
#1119=CYLINDRICAL_SURFACE('',#25044,0.14635);
#1120=CYLINDRICAL_SURFACE('',#25045,0.14635);
#1121=CYLINDRICAL_SURFACE('',#25046,0.14635);
#1122=CYLINDRICAL_SURFACE('',#25047,0.14635);
#1123=CYLINDRICAL_SURFACE('',#25048,0.14635);
#1124=CYLINDRICAL_SURFACE('',#25049,0.14635);
#1125=CYLINDRICAL_SURFACE('',#25050,0.14635);
#1126=CYLINDRICAL_SURFACE('',#25051,0.14635);
#1127=CYLINDRICAL_SURFACE('',#25052,0.14635);
#1128=CYLINDRICAL_SURFACE('',#25053,0.14635);
#1129=CYLINDRICAL_SURFACE('',#25054,0.14635);
#1130=CYLINDRICAL_SURFACE('',#25055,0.14635);
#1131=CYLINDRICAL_SURFACE('',#25056,0.14635);
#1132=CYLINDRICAL_SURFACE('',#25057,0.14635);
#1133=CYLINDRICAL_SURFACE('',#25058,0.14635);
#1134=CYLINDRICAL_SURFACE('',#25059,0.14635);
#1135=CYLINDRICAL_SURFACE('',#25060,0.14635);
#1136=CYLINDRICAL_SURFACE('',#25061,0.14635);
#1137=CYLINDRICAL_SURFACE('',#25062,0.14635);
#1138=CYLINDRICAL_SURFACE('',#25063,0.14635);
#1139=CYLINDRICAL_SURFACE('',#25064,0.14635);
#1140=CYLINDRICAL_SURFACE('',#25065,0.14635);
#1141=CYLINDRICAL_SURFACE('',#25066,0.14635);
#1142=CYLINDRICAL_SURFACE('',#25067,0.14635);
#1143=CYLINDRICAL_SURFACE('',#25068,0.14635);
#1144=CYLINDRICAL_SURFACE('',#25069,0.14635);
#1145=CYLINDRICAL_SURFACE('',#25070,0.14635);
#1146=CYLINDRICAL_SURFACE('',#25071,0.14635);
#1147=CYLINDRICAL_SURFACE('',#25072,0.14635);
#1148=CYLINDRICAL_SURFACE('',#25073,0.14635);
#1149=CYLINDRICAL_SURFACE('',#25074,0.14635);
#1150=CYLINDRICAL_SURFACE('',#25075,0.14635);
#1151=CYLINDRICAL_SURFACE('',#25076,0.14635);
#1152=CYLINDRICAL_SURFACE('',#25077,0.14635);
#1153=CYLINDRICAL_SURFACE('',#25078,0.14635);
#1154=CYLINDRICAL_SURFACE('',#25079,0.14635);
#1155=CYLINDRICAL_SURFACE('',#25080,0.14635);
#1156=CYLINDRICAL_SURFACE('',#25081,0.14635);
#1157=CYLINDRICAL_SURFACE('',#25082,0.14635);
#1158=CYLINDRICAL_SURFACE('',#25083,0.14635);
#1159=CYLINDRICAL_SURFACE('',#25084,0.14635);
#1160=CYLINDRICAL_SURFACE('',#25085,0.14635);
#1161=CYLINDRICAL_SURFACE('',#25086,0.14635);
#1162=CYLINDRICAL_SURFACE('',#25087,0.14635);
#1163=CYLINDRICAL_SURFACE('',#25088,0.14635);
#1164=CYLINDRICAL_SURFACE('',#25089,0.14635);
#1165=CYLINDRICAL_SURFACE('',#25090,0.14635);
#1166=CYLINDRICAL_SURFACE('',#25091,0.14635);
#1167=CYLINDRICAL_SURFACE('',#25092,0.14635);
#1168=CYLINDRICAL_SURFACE('',#25093,0.14635);
#1169=CYLINDRICAL_SURFACE('',#25094,0.14635);
#1170=CYLINDRICAL_SURFACE('',#25095,0.14635);
#1171=CYLINDRICAL_SURFACE('',#25096,0.14635);
#1172=CYLINDRICAL_SURFACE('',#25097,0.14635);
#1173=CYLINDRICAL_SURFACE('',#25098,0.14635);
#1174=CYLINDRICAL_SURFACE('',#25099,0.14635);
#1175=CYLINDRICAL_SURFACE('',#25100,0.117775);
#1176=CYLINDRICAL_SURFACE('',#25102,0.117775);
#1177=CYLINDRICAL_SURFACE('',#25103,0.117775);
#1178=CYLINDRICAL_SURFACE('',#25104,0.117775);
#1179=CYLINDRICAL_SURFACE('',#25105,0.117775);
#1180=CYLINDRICAL_SURFACE('',#25106,0.117775);
#1181=CYLINDRICAL_SURFACE('',#25107,0.117775);
#1182=CYLINDRICAL_SURFACE('',#25108,0.117775);
#1183=CYLINDRICAL_SURFACE('',#25109,0.117775);
#1184=CYLINDRICAL_SURFACE('',#25110,0.117775);
#1185=CYLINDRICAL_SURFACE('',#25111,0.117775);
#1186=CYLINDRICAL_SURFACE('',#25112,0.117775);
#1187=CYLINDRICAL_SURFACE('',#25113,0.117775);
#1188=CYLINDRICAL_SURFACE('',#25114,0.117775);
#1189=CYLINDRICAL_SURFACE('',#25115,0.117775);
#1190=CYLINDRICAL_SURFACE('',#25116,0.117775);
#1191=CYLINDRICAL_SURFACE('',#25117,0.117775);
#1192=CYLINDRICAL_SURFACE('',#25118,0.117775);
#1193=CYLINDRICAL_SURFACE('',#25119,0.117775);
#1194=CYLINDRICAL_SURFACE('',#25120,0.117775);
#1195=CYLINDRICAL_SURFACE('',#25121,0.117775);
#1196=CYLINDRICAL_SURFACE('',#25122,0.117775);
#1197=CYLINDRICAL_SURFACE('',#25123,0.117775);
#1198=CYLINDRICAL_SURFACE('',#25124,0.117775);
#1199=CYLINDRICAL_SURFACE('',#25125,0.117775);
#1200=CYLINDRICAL_SURFACE('',#25126,0.117775);
#1201=CYLINDRICAL_SURFACE('',#25127,0.117775);
#1202=CYLINDRICAL_SURFACE('',#25128,0.117775);
#1203=CYLINDRICAL_SURFACE('',#25129,0.117775);
#1204=CYLINDRICAL_SURFACE('',#25130,0.117775);
#1205=CYLINDRICAL_SURFACE('',#25131,0.117775);
#1206=CYLINDRICAL_SURFACE('',#25132,0.117775);
#1207=CYLINDRICAL_SURFACE('',#25133,0.117775);
#1208=CYLINDRICAL_SURFACE('',#25134,0.117775);
#1209=CYLINDRICAL_SURFACE('',#25135,0.117775);
#1210=CYLINDRICAL_SURFACE('',#25136,0.117775);
#1211=CYLINDRICAL_SURFACE('',#25137,0.117775);
#1212=CYLINDRICAL_SURFACE('',#25138,0.117775);
#1213=CYLINDRICAL_SURFACE('',#25139,0.117775);
#1214=CYLINDRICAL_SURFACE('',#25140,0.117775);
#1215=CYLINDRICAL_SURFACE('',#25141,0.117775);
#1216=CYLINDRICAL_SURFACE('',#25142,0.117775);
#1217=CYLINDRICAL_SURFACE('',#25143,0.117775);
#1218=CYLINDRICAL_SURFACE('',#25144,0.117775);
#1219=CYLINDRICAL_SURFACE('',#25145,0.117775);
#1220=CYLINDRICAL_SURFACE('',#25146,0.117775);
#1221=CYLINDRICAL_SURFACE('',#25147,0.117775);
#1222=CYLINDRICAL_SURFACE('',#25148,0.117775);
#1223=CYLINDRICAL_SURFACE('',#25149,0.117775);
#1224=CYLINDRICAL_SURFACE('',#25150,0.117775);
#1225=CYLINDRICAL_SURFACE('',#25151,0.117775);
#1226=CYLINDRICAL_SURFACE('',#25152,0.117775);
#1227=CYLINDRICAL_SURFACE('',#25153,0.117775);
#1228=CYLINDRICAL_SURFACE('',#25154,0.117775);
#1229=CYLINDRICAL_SURFACE('',#25155,0.117775);
#1230=CYLINDRICAL_SURFACE('',#25156,0.117775);
#1231=CYLINDRICAL_SURFACE('',#25157,0.117775);
#1232=CYLINDRICAL_SURFACE('',#25158,0.117775);
#1233=CYLINDRICAL_SURFACE('',#25159,0.117775);
#1234=CYLINDRICAL_SURFACE('',#25165,0.117775);
#1235=CYLINDRICAL_SURFACE('',#25307,0.275);
#1236=CYLINDRICAL_SURFACE('',#25363,0.14635);
#1237=CYLINDRICAL_SURFACE('',#25370,0.24505);
#1238=CYLINDRICAL_SURFACE('',#25374,0.24505);
#1239=CYLINDRICAL_SURFACE('',#25375,0.24505);
#1240=CYLINDRICAL_SURFACE('',#25376,0.24505);
#1241=CYLINDRICAL_SURFACE('',#25377,0.24505);
#1242=CYLINDRICAL_SURFACE('',#25378,0.24505);
#1243=CYLINDRICAL_SURFACE('',#25379,0.24505);
#1244=CYLINDRICAL_SURFACE('',#25380,0.24505);
#1245=CYLINDRICAL_SURFACE('',#25381,0.24505);
#1246=CYLINDRICAL_SURFACE('',#25382,0.24505);
#1247=CYLINDRICAL_SURFACE('',#25383,0.24505);
#1248=CYLINDRICAL_SURFACE('',#25384,0.24505);
#1249=CYLINDRICAL_SURFACE('',#25385,0.24505);
#1250=CYLINDRICAL_SURFACE('',#25386,0.24505);
#1251=CYLINDRICAL_SURFACE('',#25387,0.24505);
#1252=CYLINDRICAL_SURFACE('',#25388,0.24505);
#1253=CYLINDRICAL_SURFACE('',#25389,0.24505);
#1254=CYLINDRICAL_SURFACE('',#25390,0.24505);
#1255=CYLINDRICAL_SURFACE('',#25391,0.199475);
#1256=CYLINDRICAL_SURFACE('',#25393,0.199475);
#1257=CYLINDRICAL_SURFACE('',#25394,0.199475);
#1258=CYLINDRICAL_SURFACE('',#25395,0.199475);
#1259=CYLINDRICAL_SURFACE('',#25396,0.199475);
#1260=CYLINDRICAL_SURFACE('',#25397,0.199475);
#1261=CYLINDRICAL_SURFACE('',#25398,0.199475);
#1262=CYLINDRICAL_SURFACE('',#25399,0.199475);
#1263=CYLINDRICAL_SURFACE('',#25400,0.199475);
#1264=CYLINDRICAL_SURFACE('',#25401,0.199475);
#1265=CYLINDRICAL_SURFACE('',#25402,0.199475);
#1266=CYLINDRICAL_SURFACE('',#25403,0.199475);
#1267=CYLINDRICAL_SURFACE('',#25404,0.199475);
#1268=CYLINDRICAL_SURFACE('',#25405,0.199475);
#1269=CYLINDRICAL_SURFACE('',#25406,0.199475);
#1270=CYLINDRICAL_SURFACE('',#25407,0.199475);
#1271=CYLINDRICAL_SURFACE('',#25408,0.199475);
#1272=CYLINDRICAL_SURFACE('',#25409,0.199475);
#1273=CYLINDRICAL_SURFACE('',#25410,0.199475);
#1274=CYLINDRICAL_SURFACE('',#25416,0.199475);
#1275=CYLINDRICAL_SURFACE('',#25558,0.425);
#1276=CYLINDRICAL_SURFACE('',#25614,0.24505);
#1277=FACE_BOUND('',#3577,.T.);
#1278=FACE_BOUND('',#3578,.T.);
#1279=FACE_BOUND('',#3579,.T.);
#1280=FACE_BOUND('',#3580,.T.);
#1281=FACE_BOUND('',#3581,.T.);
#1282=FACE_BOUND('',#3582,.T.);
#1283=FACE_BOUND('',#3583,.T.);
#1284=FACE_BOUND('',#3612,.T.);
#1285=FACE_BOUND('',#3613,.T.);
#1286=FACE_BOUND('',#3614,.T.);
#1287=FACE_BOUND('',#3615,.T.);
#1288=FACE_BOUND('',#3616,.T.);
#1289=FACE_BOUND('',#3617,.T.);
#1290=FACE_BOUND('',#3618,.T.);
#1291=FACE_BOUND('',#3648,.T.);
#1292=FACE_BOUND('',#3653,.T.);
#1293=FACE_BOUND('',#3658,.T.);
#1294=FACE_BOUND('',#3663,.T.);
#1295=FACE_BOUND('',#3668,.T.);
#1296=FACE_BOUND('',#3673,.T.);
#1297=FACE_BOUND('',#3678,.T.);
#1298=FACE_BOUND('',#3695,.T.);
#1299=FACE_BOUND('',#3696,.T.);
#1300=FACE_BOUND('',#3697,.T.);
#1301=FACE_BOUND('',#3698,.T.);
#1302=FACE_BOUND('',#3699,.T.);
#1303=FACE_BOUND('',#3700,.T.);
#1304=FACE_BOUND('',#3701,.T.);
#1305=FACE_BOUND('',#3704,.T.);
#1306=FACE_BOUND('',#3705,.T.);
#1307=FACE_BOUND('',#3706,.T.);
#1308=FACE_BOUND('',#3738,.T.);
#1309=FACE_BOUND('',#3739,.T.);
#1310=FACE_BOUND('',#3740,.T.);
#1311=FACE_BOUND('',#3741,.T.);
#1312=FACE_BOUND('',#3742,.T.);
#1313=FACE_BOUND('',#3743,.T.);
#1314=FACE_BOUND('',#3744,.T.);
#1315=FACE_BOUND('',#3745,.T.);
#1316=FACE_BOUND('',#3746,.T.);
#1317=FACE_BOUND('',#3747,.T.);
#1318=FACE_BOUND('',#3754,.T.);
#1319=FACE_BOUND('',#3773,.T.);
#1320=FACE_BOUND('',#3813,.T.);
#1321=FACE_BOUND('',#3814,.T.);
#1322=FACE_BOUND('',#3815,.T.);
#1323=FACE_BOUND('',#3816,.T.);
#1324=FACE_BOUND('',#3857,.T.);
#1325=FACE_BOUND('',#3861,.T.);
#1326=FACE_BOUND('',#3888,.T.);
#1327=FACE_BOUND('',#3889,.T.);
#1328=FACE_BOUND('',#3890,.T.);
#1329=FACE_BOUND('',#3891,.T.);
#1330=FACE_BOUND('',#3896,.T.);
#1331=FACE_BOUND('',#3914,.T.);
#1332=FACE_BOUND('',#3915,.T.);
#1333=FACE_BOUND('',#3916,.T.);
#1334=FACE_BOUND('',#3917,.T.);
#1335=FACE_BOUND('',#3918,.T.);
#1336=FACE_BOUND('',#3919,.T.);
#1337=FACE_BOUND('',#3920,.T.);
#1338=FACE_BOUND('',#3923,.T.);
#1339=FACE_BOUND('',#3924,.T.);
#1340=FACE_BOUND('',#3925,.T.);
#1341=FACE_BOUND('',#3926,.T.);
#1342=FACE_BOUND('',#3927,.T.);
#1343=FACE_BOUND('',#3928,.T.);
#1344=FACE_BOUND('',#3929,.T.);
#1345=FACE_BOUND('',#4080,.T.);
#1346=FACE_BOUND('',#4083,.T.);
#1347=FACE_BOUND('',#4084,.T.);
#1348=FACE_BOUND('',#4085,.T.);
#1349=FACE_BOUND('',#4086,.T.);
#1350=FACE_BOUND('',#4087,.T.);
#1351=FACE_BOUND('',#4088,.T.);
#1352=FACE_BOUND('',#4089,.T.);
#1353=FACE_BOUND('',#4090,.T.);
#1354=FACE_BOUND('',#4091,.T.);
#1355=FACE_BOUND('',#4092,.T.);
#1356=FACE_BOUND('',#4093,.T.);
#1357=FACE_BOUND('',#4094,.T.);
#1358=FACE_BOUND('',#4095,.T.);
#1359=FACE_BOUND('',#4096,.T.);
#1360=FACE_BOUND('',#4097,.T.);
#1361=FACE_BOUND('',#4098,.T.);
#1362=FACE_BOUND('',#4099,.T.);
#1363=FACE_BOUND('',#4100,.T.);
#1364=FACE_BOUND('',#4101,.T.);
#1365=FACE_BOUND('',#4102,.T.);
#1366=FACE_BOUND('',#4103,.T.);
#1367=FACE_BOUND('',#4104,.T.);
#1368=FACE_BOUND('',#4105,.T.);
#1369=FACE_BOUND('',#4107,.T.);
#1370=FACE_BOUND('',#4111,.T.);
#1371=FACE_BOUND('',#4119,.T.);
#1372=FACE_BOUND('',#4121,.T.);
#1373=FACE_BOUND('',#4122,.T.);
#1374=FACE_BOUND('',#4123,.T.);
#1375=FACE_BOUND('',#4124,.T.);
#1376=FACE_BOUND('',#4125,.T.);
#1377=FACE_BOUND('',#4131,.T.);
#1378=FACE_BOUND('',#4132,.T.);
#1379=FACE_BOUND('',#4133,.T.);
#1380=FACE_BOUND('',#4134,.T.);
#1381=FACE_BOUND('',#4135,.T.);
#1382=FACE_BOUND('',#4146,.T.);
#1383=FACE_BOUND('',#4148,.T.);
#1384=FACE_BOUND('',#4152,.T.);
#1385=FACE_BOUND('',#4154,.T.);
#1386=FACE_BOUND('',#4159,.T.);
#1387=FACE_BOUND('',#4162,.T.);
#1388=FACE_BOUND('',#4169,.T.);
#1389=FACE_BOUND('',#4245,.T.);
#1390=FACE_BOUND('',#4247,.T.);
#1391=FACE_BOUND('',#4252,.T.);
#1392=FACE_BOUND('',#4254,.T.);
#1393=FACE_BOUND('',#4255,.T.);
#1394=FACE_BOUND('',#4256,.T.);
#1395=FACE_BOUND('',#4257,.T.);
#1396=FACE_BOUND('',#4258,.T.);
#1397=FACE_BOUND('',#4259,.T.);
#1398=FACE_BOUND('',#4260,.T.);
#1399=FACE_BOUND('',#4261,.T.);
#1400=FACE_BOUND('',#4262,.T.);
#1401=FACE_BOUND('',#4263,.T.);
#1402=FACE_BOUND('',#4264,.T.);
#1403=FACE_BOUND('',#4265,.T.);
#1404=FACE_BOUND('',#4266,.T.);
#1405=FACE_BOUND('',#4267,.T.);
#1406=FACE_BOUND('',#4268,.T.);
#1407=FACE_BOUND('',#4269,.T.);
#1408=FACE_BOUND('',#4270,.T.);
#1409=FACE_BOUND('',#4272,.T.);
#1410=FACE_BOUND('',#4277,.T.);
#1411=FACE_BOUND('',#4280,.T.);
#1412=FACE_BOUND('',#4284,.T.);
#1413=FACE_BOUND('',#4287,.T.);
#1414=FACE_BOUND('',#4455,.T.);
#1415=FACE_BOUND('',#4458,.T.);
#1416=FACE_BOUND('',#4459,.T.);
#1417=FACE_BOUND('',#4460,.T.);
#1418=FACE_BOUND('',#4461,.T.);
#1419=FACE_BOUND('',#4462,.T.);
#1420=FACE_BOUND('',#4463,.T.);
#1421=FACE_BOUND('',#4464,.T.);
#1422=FACE_BOUND('',#4465,.T.);
#1423=FACE_BOUND('',#4466,.T.);
#1424=FACE_BOUND('',#4467,.T.);
#1425=FACE_BOUND('',#4468,.T.);
#1426=FACE_BOUND('',#4469,.T.);
#1427=FACE_BOUND('',#4470,.T.);
#1428=FACE_BOUND('',#4471,.T.);
#1429=FACE_BOUND('',#4472,.T.);
#1430=FACE_BOUND('',#4473,.T.);
#1431=FACE_BOUND('',#4474,.T.);
#1432=FACE_BOUND('',#4475,.T.);
#1433=FACE_BOUND('',#4476,.T.);
#1434=FACE_BOUND('',#4477,.T.);
#1435=FACE_BOUND('',#4478,.T.);
#1436=FACE_BOUND('',#4479,.T.);
#1437=FACE_BOUND('',#4480,.T.);
#1438=FACE_BOUND('',#4483,.T.);
#1439=FACE_BOUND('',#4636,.T.);
#1440=FACE_BOUND('',#4642,.T.);
#1441=FACE_BOUND('',#4644,.T.);
#1442=FACE_BOUND('',#4885,.T.);
#1443=FACE_BOUND('',#4891,.T.);
#1444=FACE_BOUND('',#4893,.T.);
#1445=FACE_BOUND('',#5054,.T.);
#1446=FACE_BOUND('',#5060,.T.);
#1447=FACE_BOUND('',#5062,.T.);
#1448=PLANE('',#23501);
#1449=PLANE('',#23505);
#1450=PLANE('',#23509);
#1451=PLANE('',#23513);
#1452=PLANE('',#23514);
#1453=PLANE('',#23517);
#1454=PLANE('',#23520);
#1455=PLANE('',#23530);
#1456=PLANE('',#23533);
#1457=PLANE('',#23537);
#1458=PLANE('',#23541);
#1459=PLANE('',#23542);
#1460=PLANE('',#23545);
#1461=PLANE('',#23548);
#1462=PLANE('',#23550);
#1463=PLANE('',#23551);
#1464=PLANE('',#23555);
#1465=PLANE('',#23559);
#1466=PLANE('',#23563);
#1467=PLANE('',#23569);
#1468=PLANE('',#23572);
#1469=PLANE('',#23573);
#1470=PLANE('',#23581);
#1471=PLANE('',#23583);
#1472=PLANE('',#23585);
#1473=PLANE('',#23589);
#1474=PLANE('',#23594);
#1475=PLANE('',#23637);
#1476=PLANE('',#23644);
#1477=PLANE('',#23651);
#1478=PLANE('',#23658);
#1479=PLANE('',#23665);
#1480=PLANE('',#23672);
#1481=PLANE('',#23679);
#1482=PLANE('',#23680);
#1483=PLANE('',#23682);
#1484=PLANE('',#23685);
#1485=PLANE('',#23687);
#1486=PLANE('',#23688);
#1487=PLANE('',#23692);
#1488=PLANE('',#23696);
#1489=PLANE('',#23699);
#1490=PLANE('',#23700);
#1491=PLANE('',#23701);
#1492=PLANE('',#23709);
#1493=PLANE('',#23710);
#1494=PLANE('',#23714);
#1495=PLANE('',#23715);
#1496=PLANE('',#23716);
#1497=PLANE('',#23719);
#1498=PLANE('',#23723);
#1499=PLANE('',#23725);
#1500=PLANE('',#23726);
#1501=PLANE('',#23727);
#1502=PLANE('',#23728);
#1503=PLANE('',#23729);
#1504=PLANE('',#23730);
#1505=PLANE('',#23734);
#1506=PLANE('',#23740);
#1507=PLANE('',#23741);
#1508=PLANE('',#23743);
#1509=PLANE('',#23744);
#1510=PLANE('',#23745);
#1511=PLANE('',#23748);
#1512=PLANE('',#23752);
#1513=PLANE('',#23754);
#1514=PLANE('',#23755);
#1515=PLANE('',#23777);
#1516=PLANE('',#23814);
#1517=PLANE('',#23854);
#1518=PLANE('',#23860);
#1519=PLANE('',#23864);
#1520=PLANE('',#23868);
#1521=PLANE('',#23872);
#1522=PLANE('',#23873);
#1523=PLANE('',#23876);
#1524=PLANE('',#23879);
#1525=PLANE('',#23884);
#1526=PLANE('',#23888);
#1527=PLANE('',#23891);
#1528=PLANE('',#23894);
#1529=PLANE('',#23900);
#1530=PLANE('',#23903);
#1531=PLANE('',#23905);
#1532=PLANE('',#23908);
#1533=PLANE('',#23911);
#1534=PLANE('',#23915);
#1535=PLANE('',#23919);
#1536=PLANE('',#23920);
#1537=PLANE('',#23923);
#1538=PLANE('',#23933);
#1539=PLANE('',#23936);
#1540=PLANE('',#23940);
#1541=PLANE('',#23944);
#1542=PLANE('',#23945);
#1543=PLANE('',#23947);
#1544=PLANE('',#23948);
#1545=PLANE('',#23955);
#1546=PLANE('',#23977);
#1547=PLANE('',#23979);
#1548=PLANE('',#23981);
#1549=PLANE('',#23999);
#1550=PLANE('',#24010);
#1551=PLANE('',#24045);
#1552=PLANE('',#24055);
#1553=PLANE('',#24132);
#1554=PLANE('',#24147);
#1555=PLANE('',#24148);
#1556=PLANE('',#24150);
#1557=PLANE('',#24151);
#1558=PLANE('',#24153);
#1559=PLANE('',#24154);
#1560=PLANE('',#24156);
#1561=PLANE('',#24157);
#1562=PLANE('',#24159);
#1563=PLANE('',#24160);
#1564=PLANE('',#24162);
#1565=PLANE('',#24163);
#1566=PLANE('',#24165);
#1567=PLANE('',#24166);
#1568=PLANE('',#24168);
#1569=PLANE('',#24169);
#1570=PLANE('',#24171);
#1571=PLANE('',#24172);
#1572=PLANE('',#24174);
#1573=PLANE('',#24175);
#1574=PLANE('',#24177);
#1575=PLANE('',#24178);
#1576=PLANE('',#24180);
#1577=PLANE('',#24181);
#1578=PLANE('',#24183);
#1579=PLANE('',#24184);
#1580=PLANE('',#24186);
#1581=PLANE('',#24187);
#1582=PLANE('',#24189);
#1583=PLANE('',#24190);
#1584=PLANE('',#24192);
#1585=PLANE('',#24193);
#1586=PLANE('',#24195);
#1587=PLANE('',#24196);
#1588=PLANE('',#24198);
#1589=PLANE('',#24199);
#1590=PLANE('',#24201);
#1591=PLANE('',#24202);
#1592=PLANE('',#24204);
#1593=PLANE('',#24205);
#1594=PLANE('',#24207);
#1595=PLANE('',#24208);
#1596=PLANE('',#24210);
#1597=PLANE('',#24211);
#1598=PLANE('',#24213);
#1599=PLANE('',#24214);
#1600=PLANE('',#24217);
#1601=PLANE('',#24218);
#1602=PLANE('',#24221);
#1603=PLANE('',#24222);
#1604=PLANE('',#24224);
#1605=PLANE('',#24225);
#1606=PLANE('',#24227);
#1607=PLANE('',#24228);
#1608=PLANE('',#24230);
#1609=PLANE('',#24231);
#1610=PLANE('',#24233);
#1611=PLANE('',#24234);
#1612=PLANE('',#24236);
#1613=PLANE('',#24237);
#1614=PLANE('',#24239);
#1615=PLANE('',#24240);
#1616=PLANE('',#24242);
#1617=PLANE('',#24243);
#1618=PLANE('',#24245);
#1619=PLANE('',#24246);
#1620=PLANE('',#24248);
#1621=PLANE('',#24249);
#1622=PLANE('',#24251);
#1623=PLANE('',#24252);
#1624=PLANE('',#24254);
#1625=PLANE('',#24255);
#1626=PLANE('',#24257);
#1627=PLANE('',#24258);
#1628=PLANE('',#24260);
#1629=PLANE('',#24261);
#1630=PLANE('',#24263);
#1631=PLANE('',#24264);
#1632=PLANE('',#24266);
#1633=PLANE('',#24267);
#1634=PLANE('',#24269);
#1635=PLANE('',#24270);
#1636=PLANE('',#24272);
#1637=PLANE('',#24273);
#1638=PLANE('',#24275);
#1639=PLANE('',#24276);
#1640=PLANE('',#24278);
#1641=PLANE('',#24279);
#1642=PLANE('',#24281);
#1643=PLANE('',#24282);
#1644=PLANE('',#24284);
#1645=PLANE('',#24285);
#1646=PLANE('',#24287);
#1647=PLANE('',#24288);
#1648=PLANE('',#24290);
#1649=PLANE('',#24291);
#1650=PLANE('',#24298);
#1651=PLANE('',#24299);
#1652=PLANE('',#24306);
#1653=PLANE('',#24312);
#1654=PLANE('',#24313);
#1655=PLANE('',#24314);
#1656=PLANE('',#24315);
#1657=PLANE('',#24316);
#1658=PLANE('',#24317);
#1659=PLANE('',#24318);
#1660=PLANE('',#24319);
#1661=PLANE('',#24320);
#1662=PLANE('',#24322);
#1663=PLANE('',#24323);
#1664=PLANE('',#24324);
#1665=PLANE('',#24325);
#1666=PLANE('',#24326);
#1667=PLANE('',#24327);
#1668=PLANE('',#24339);
#1669=PLANE('',#24342);
#1670=PLANE('',#24347);
#1671=PLANE('',#24349);
#1672=PLANE('',#24357);
#1673=PLANE('',#24359);
#1674=PLANE('',#24367);
#1675=PLANE('',#24371);
#1676=PLANE('',#24387);
#1677=PLANE('',#24389);
#1678=PLANE('',#24390);
#1679=PLANE('',#24392);
#1680=PLANE('',#24393);
#1681=PLANE('',#24395);
#1682=PLANE('',#24396);
#1683=PLANE('',#24398);
#1684=PLANE('',#24399);
#1685=PLANE('',#24401);
#1686=PLANE('',#24402);
#1687=PLANE('',#24404);
#1688=PLANE('',#24405);
#1689=PLANE('',#24407);
#1690=PLANE('',#24408);
#1691=PLANE('',#24410);
#1692=PLANE('',#24411);
#1693=PLANE('',#24413);
#1694=PLANE('',#24414);
#1695=PLANE('',#24416);
#1696=PLANE('',#24417);
#1697=PLANE('',#24419);
#1698=PLANE('',#24420);
#1699=PLANE('',#24422);
#1700=PLANE('',#24423);
#1701=PLANE('',#24425);
#1702=PLANE('',#24426);
#1703=PLANE('',#24428);
#1704=PLANE('',#24429);
#1705=PLANE('',#24431);
#1706=PLANE('',#24432);
#1707=PLANE('',#24434);
#1708=PLANE('',#24435);
#1709=PLANE('',#24437);
#1710=PLANE('',#24438);
#1711=PLANE('',#24441);
#1712=PLANE('',#24442);
#1713=PLANE('',#24445);
#1714=PLANE('',#24446);
#1715=PLANE('',#24448);
#1716=PLANE('',#24449);
#1717=PLANE('',#24451);
#1718=PLANE('',#24452);
#1719=PLANE('',#24454);
#1720=PLANE('',#24455);
#1721=PLANE('',#24457);
#1722=PLANE('',#24458);
#1723=PLANE('',#24460);
#1724=PLANE('',#24461);
#1725=PLANE('',#24463);
#1726=PLANE('',#24464);
#1727=PLANE('',#24466);
#1728=PLANE('',#24467);
#1729=PLANE('',#24469);
#1730=PLANE('',#24470);
#1731=PLANE('',#24472);
#1732=PLANE('',#24473);
#1733=PLANE('',#24475);
#1734=PLANE('',#24476);
#1735=PLANE('',#24478);
#1736=PLANE('',#24479);
#1737=PLANE('',#24481);
#1738=PLANE('',#24482);
#1739=PLANE('',#24484);
#1740=PLANE('',#24485);
#1741=PLANE('',#24487);
#1742=PLANE('',#24488);
#1743=PLANE('',#24490);
#1744=PLANE('',#24491);
#1745=PLANE('',#24493);
#1746=PLANE('',#24494);
#1747=PLANE('',#24496);
#1748=PLANE('',#24497);
#1749=PLANE('',#24505);
#1750=PLANE('',#24506);
#1751=PLANE('',#24508);
#1752=PLANE('',#24512);
#1753=PLANE('',#24516);
#1754=PLANE('',#24520);
#1755=PLANE('',#24525);
#1756=PLANE('',#24529);
#1757=PLANE('',#24537);
#1758=PLANE('',#24542);
#1759=PLANE('',#24547);
#1760=PLANE('',#24550);
#1761=PLANE('',#24553);
#1762=PLANE('',#24554);
#1763=PLANE('',#24555);
#1764=PLANE('',#24559);
#1765=PLANE('',#24563);
#1766=PLANE('',#24566);
#1767=PLANE('',#24567);
#1768=PLANE('',#24568);
#1769=PLANE('',#24571);
#1770=PLANE('',#24574);
#1771=PLANE('',#24577);
#1772=PLANE('',#24579);
#1773=PLANE('',#24580);
#1774=PLANE('',#24582);
#1775=PLANE('',#24584);
#1776=PLANE('',#24630);
#1777=PLANE('',#24637);
#1778=PLANE('',#24638);
#1779=PLANE('',#24640);
#1780=PLANE('',#24641);
#1781=PLANE('',#24643);
#1782=PLANE('',#24644);
#1783=PLANE('',#24646);
#1784=PLANE('',#24647);
#1785=PLANE('',#24649);
#1786=PLANE('',#24650);
#1787=PLANE('',#24652);
#1788=PLANE('',#24653);
#1789=PLANE('',#24655);
#1790=PLANE('',#24656);
#1791=PLANE('',#24658);
#1792=PLANE('',#24659);
#1793=PLANE('',#24661);
#1794=PLANE('',#24662);
#1795=PLANE('',#24664);
#1796=PLANE('',#24665);
#1797=PLANE('',#24667);
#1798=PLANE('',#24668);
#1799=PLANE('',#24670);
#1800=PLANE('',#24671);
#1801=PLANE('',#24673);
#1802=PLANE('',#24674);
#1803=PLANE('',#24676);
#1804=PLANE('',#24677);
#1805=PLANE('',#24679);
#1806=PLANE('',#24680);
#1807=PLANE('',#24682);
#1808=PLANE('',#24683);
#1809=PLANE('',#24685);
#1810=PLANE('',#24686);
#1811=PLANE('',#24688);
#1812=PLANE('',#24689);
#1813=PLANE('',#24691);
#1814=PLANE('',#24692);
#1815=PLANE('',#24694);
#1816=PLANE('',#24695);
#1817=PLANE('',#24697);
#1818=PLANE('',#24698);
#1819=PLANE('',#24700);
#1820=PLANE('',#24701);
#1821=PLANE('',#24703);
#1822=PLANE('',#24704);
#1823=PLANE('',#24707);
#1824=PLANE('',#24708);
#1825=PLANE('',#24711);
#1826=PLANE('',#24712);
#1827=PLANE('',#24714);
#1828=PLANE('',#24715);
#1829=PLANE('',#24717);
#1830=PLANE('',#24718);
#1831=PLANE('',#24720);
#1832=PLANE('',#24721);
#1833=PLANE('',#24723);
#1834=PLANE('',#24724);
#1835=PLANE('',#24726);
#1836=PLANE('',#24727);
#1837=PLANE('',#24729);
#1838=PLANE('',#24730);
#1839=PLANE('',#24732);
#1840=PLANE('',#24733);
#1841=PLANE('',#24735);
#1842=PLANE('',#24736);
#1843=PLANE('',#24738);
#1844=PLANE('',#24739);
#1845=PLANE('',#24741);
#1846=PLANE('',#24742);
#1847=PLANE('',#24744);
#1848=PLANE('',#24745);
#1849=PLANE('',#24747);
#1850=PLANE('',#24748);
#1851=PLANE('',#24750);
#1852=PLANE('',#24751);
#1853=PLANE('',#24753);
#1854=PLANE('',#24754);
#1855=PLANE('',#24756);
#1856=PLANE('',#24757);
#1857=PLANE('',#24759);
#1858=PLANE('',#24760);
#1859=PLANE('',#24762);
#1860=PLANE('',#24763);
#1861=PLANE('',#24765);
#1862=PLANE('',#24766);
#1863=PLANE('',#24768);
#1864=PLANE('',#24769);
#1865=PLANE('',#24771);
#1866=PLANE('',#24772);
#1867=PLANE('',#24774);
#1868=PLANE('',#24775);
#1869=PLANE('',#24777);
#1870=PLANE('',#24778);
#1871=PLANE('',#24780);
#1872=PLANE('',#24781);
#1873=PLANE('',#24783);
#1874=PLANE('',#24786);
#1875=PLANE('',#24794);
#1876=PLANE('',#24829);
#1877=PLANE('',#24832);
#1878=PLANE('',#24835);
#1879=PLANE('',#24837);
#1880=PLANE('',#24838);
#1881=PLANE('',#24839);
#1882=PLANE('',#24841);
#1883=PLANE('',#24842);
#1884=PLANE('',#24843);
#1885=PLANE('',#24845);
#1886=PLANE('',#24846);
#1887=PLANE('',#24847);
#1888=PLANE('',#24849);
#1889=PLANE('',#24850);
#1890=PLANE('',#24851);
#1891=PLANE('',#24853);
#1892=PLANE('',#24854);
#1893=PLANE('',#24855);
#1894=PLANE('',#24857);
#1895=PLANE('',#24858);
#1896=PLANE('',#24859);
#1897=PLANE('',#24861);
#1898=PLANE('',#24862);
#1899=PLANE('',#24863);
#1900=PLANE('',#24865);
#1901=PLANE('',#24866);
#1902=PLANE('',#24867);
#1903=PLANE('',#24869);
#1904=PLANE('',#24870);
#1905=PLANE('',#24871);
#1906=PLANE('',#24873);
#1907=PLANE('',#24874);
#1908=PLANE('',#24875);
#1909=PLANE('',#24877);
#1910=PLANE('',#24878);
#1911=PLANE('',#24879);
#1912=PLANE('',#24881);
#1913=PLANE('',#24882);
#1914=PLANE('',#24883);
#1915=PLANE('',#24885);
#1916=PLANE('',#24886);
#1917=PLANE('',#24887);
#1918=PLANE('',#24889);
#1919=PLANE('',#24890);
#1920=PLANE('',#24891);
#1921=PLANE('',#24893);
#1922=PLANE('',#24894);
#1923=PLANE('',#24895);
#1924=PLANE('',#24897);
#1925=PLANE('',#24898);
#1926=PLANE('',#24899);
#1927=PLANE('',#24901);
#1928=PLANE('',#24902);
#1929=PLANE('',#24903);
#1930=PLANE('',#24906);
#1931=PLANE('',#24907);
#1932=PLANE('',#24908);
#1933=PLANE('',#24910);
#1934=PLANE('',#24911);
#1935=PLANE('',#24912);
#1936=PLANE('',#24914);
#1937=PLANE('',#24915);
#1938=PLANE('',#24916);
#1939=PLANE('',#24918);
#1940=PLANE('',#24919);
#1941=PLANE('',#24920);
#1942=PLANE('',#24922);
#1943=PLANE('',#24923);
#1944=PLANE('',#24924);
#1945=PLANE('',#24926);
#1946=PLANE('',#24927);
#1947=PLANE('',#24928);
#1948=PLANE('',#24930);
#1949=PLANE('',#24931);
#1950=PLANE('',#24932);
#1951=PLANE('',#24934);
#1952=PLANE('',#24935);
#1953=PLANE('',#24936);
#1954=PLANE('',#24938);
#1955=PLANE('',#24939);
#1956=PLANE('',#24940);
#1957=PLANE('',#24942);
#1958=PLANE('',#24943);
#1959=PLANE('',#24944);
#1960=PLANE('',#24946);
#1961=PLANE('',#24947);
#1962=PLANE('',#24948);
#1963=PLANE('',#24950);
#1964=PLANE('',#24951);
#1965=PLANE('',#24952);
#1966=PLANE('',#24954);
#1967=PLANE('',#24955);
#1968=PLANE('',#24956);
#1969=PLANE('',#24958);
#1970=PLANE('',#24959);
#1971=PLANE('',#24960);
#1972=PLANE('',#24962);
#1973=PLANE('',#24963);
#1974=PLANE('',#24964);
#1975=PLANE('',#24966);
#1976=PLANE('',#24967);
#1977=PLANE('',#24968);
#1978=PLANE('',#24970);
#1979=PLANE('',#24971);
#1980=PLANE('',#24972);
#1981=PLANE('',#24974);
#1982=PLANE('',#24975);
#1983=PLANE('',#25015);
#1984=PLANE('',#25016);
#1985=PLANE('',#25017);
#1986=PLANE('',#25022);
#1987=PLANE('',#25023);
#1988=PLANE('',#25024);
#1989=PLANE('',#25025);
#1990=PLANE('',#25026);
#1991=PLANE('',#25027);
#1992=PLANE('',#25028);
#1993=PLANE('',#25029);
#1994=PLANE('',#25036);
#1995=PLANE('',#25037);
#1996=PLANE('',#25160);
#1997=PLANE('',#25163);
#1998=PLANE('',#25166);
#1999=PLANE('',#25168);
#2000=PLANE('',#25169);
#2001=PLANE('',#25170);
#2002=PLANE('',#25172);
#2003=PLANE('',#25173);
#2004=PLANE('',#25174);
#2005=PLANE('',#25176);
#2006=PLANE('',#25177);
#2007=PLANE('',#25178);
#2008=PLANE('',#25180);
#2009=PLANE('',#25181);
#2010=PLANE('',#25182);
#2011=PLANE('',#25184);
#2012=PLANE('',#25185);
#2013=PLANE('',#25186);
#2014=PLANE('',#25188);
#2015=PLANE('',#25189);
#2016=PLANE('',#25190);
#2017=PLANE('',#25192);
#2018=PLANE('',#25193);
#2019=PLANE('',#25194);
#2020=PLANE('',#25196);
#2021=PLANE('',#25197);
#2022=PLANE('',#25198);
#2023=PLANE('',#25200);
#2024=PLANE('',#25201);
#2025=PLANE('',#25202);
#2026=PLANE('',#25204);
#2027=PLANE('',#25205);
#2028=PLANE('',#25206);
#2029=PLANE('',#25208);
#2030=PLANE('',#25209);
#2031=PLANE('',#25210);
#2032=PLANE('',#25212);
#2033=PLANE('',#25213);
#2034=PLANE('',#25214);
#2035=PLANE('',#25216);
#2036=PLANE('',#25217);
#2037=PLANE('',#25218);
#2038=PLANE('',#25220);
#2039=PLANE('',#25221);
#2040=PLANE('',#25222);
#2041=PLANE('',#25224);
#2042=PLANE('',#25225);
#2043=PLANE('',#25226);
#2044=PLANE('',#25228);
#2045=PLANE('',#25229);
#2046=PLANE('',#25230);
#2047=PLANE('',#25232);
#2048=PLANE('',#25233);
#2049=PLANE('',#25234);
#2050=PLANE('',#25237);
#2051=PLANE('',#25238);
#2052=PLANE('',#25239);
#2053=PLANE('',#25241);
#2054=PLANE('',#25242);
#2055=PLANE('',#25243);
#2056=PLANE('',#25245);
#2057=PLANE('',#25246);
#2058=PLANE('',#25247);
#2059=PLANE('',#25249);
#2060=PLANE('',#25250);
#2061=PLANE('',#25251);
#2062=PLANE('',#25253);
#2063=PLANE('',#25254);
#2064=PLANE('',#25255);
#2065=PLANE('',#25257);
#2066=PLANE('',#25258);
#2067=PLANE('',#25259);
#2068=PLANE('',#25261);
#2069=PLANE('',#25262);
#2070=PLANE('',#25263);
#2071=PLANE('',#25265);
#2072=PLANE('',#25266);
#2073=PLANE('',#25267);
#2074=PLANE('',#25269);
#2075=PLANE('',#25270);
#2076=PLANE('',#25271);
#2077=PLANE('',#25273);
#2078=PLANE('',#25274);
#2079=PLANE('',#25275);
#2080=PLANE('',#25277);
#2081=PLANE('',#25278);
#2082=PLANE('',#25279);
#2083=PLANE('',#25281);
#2084=PLANE('',#25282);
#2085=PLANE('',#25283);
#2086=PLANE('',#25285);
#2087=PLANE('',#25286);
#2088=PLANE('',#25287);
#2089=PLANE('',#25289);
#2090=PLANE('',#25290);
#2091=PLANE('',#25291);
#2092=PLANE('',#25293);
#2093=PLANE('',#25294);
#2094=PLANE('',#25295);
#2095=PLANE('',#25297);
#2096=PLANE('',#25298);
#2097=PLANE('',#25299);
#2098=PLANE('',#25301);
#2099=PLANE('',#25302);
#2100=PLANE('',#25303);
#2101=PLANE('',#25305);
#2102=PLANE('',#25306);
#2103=PLANE('',#25346);
#2104=PLANE('',#25347);
#2105=PLANE('',#25348);
#2106=PLANE('',#25353);
#2107=PLANE('',#25354);
#2108=PLANE('',#25355);
#2109=PLANE('',#25356);
#2110=PLANE('',#25357);
#2111=PLANE('',#25358);
#2112=PLANE('',#25359);
#2113=PLANE('',#25360);
#2114=PLANE('',#25367);
#2115=PLANE('',#25368);
#2116=PLANE('',#25411);
#2117=PLANE('',#25414);
#2118=PLANE('',#25417);
#2119=PLANE('',#25419);
#2120=PLANE('',#25420);
#2121=PLANE('',#25421);
#2122=PLANE('',#25423);
#2123=PLANE('',#25424);
#2124=PLANE('',#25425);
#2125=PLANE('',#25427);
#2126=PLANE('',#25428);
#2127=PLANE('',#25429);
#2128=PLANE('',#25431);
#2129=PLANE('',#25432);
#2130=PLANE('',#25433);
#2131=PLANE('',#25435);
#2132=PLANE('',#25436);
#2133=PLANE('',#25437);
#2134=PLANE('',#25439);
#2135=PLANE('',#25440);
#2136=PLANE('',#25441);
#2137=PLANE('',#25443);
#2138=PLANE('',#25444);
#2139=PLANE('',#25445);
#2140=PLANE('',#25447);
#2141=PLANE('',#25448);
#2142=PLANE('',#25449);
#2143=PLANE('',#25451);
#2144=PLANE('',#25452);
#2145=PLANE('',#25453);
#2146=PLANE('',#25455);
#2147=PLANE('',#25456);
#2148=PLANE('',#25457);
#2149=PLANE('',#25459);
#2150=PLANE('',#25460);
#2151=PLANE('',#25461);
#2152=PLANE('',#25463);
#2153=PLANE('',#25464);
#2154=PLANE('',#25465);
#2155=PLANE('',#25467);
#2156=PLANE('',#25468);
#2157=PLANE('',#25469);
#2158=PLANE('',#25471);
#2159=PLANE('',#25472);
#2160=PLANE('',#25473);
#2161=PLANE('',#25475);
#2162=PLANE('',#25476);
#2163=PLANE('',#25477);
#2164=PLANE('',#25479);
#2165=PLANE('',#25480);
#2166=PLANE('',#25481);
#2167=PLANE('',#25483);
#2168=PLANE('',#25484);
#2169=PLANE('',#25485);
#2170=PLANE('',#25488);
#2171=PLANE('',#25489);
#2172=PLANE('',#25490);
#2173=PLANE('',#25492);
#2174=PLANE('',#25493);
#2175=PLANE('',#25494);
#2176=PLANE('',#25496);
#2177=PLANE('',#25497);
#2178=PLANE('',#25498);
#2179=PLANE('',#25500);
#2180=PLANE('',#25501);
#2181=PLANE('',#25502);
#2182=PLANE('',#25504);
#2183=PLANE('',#25505);
#2184=PLANE('',#25506);
#2185=PLANE('',#25508);
#2186=PLANE('',#25509);
#2187=PLANE('',#25510);
#2188=PLANE('',#25512);
#2189=PLANE('',#25513);
#2190=PLANE('',#25514);
#2191=PLANE('',#25516);
#2192=PLANE('',#25517);
#2193=PLANE('',#25518);
#2194=PLANE('',#25520);
#2195=PLANE('',#25521);
#2196=PLANE('',#25522);
#2197=PLANE('',#25524);
#2198=PLANE('',#25525);
#2199=PLANE('',#25526);
#2200=PLANE('',#25528);
#2201=PLANE('',#25529);
#2202=PLANE('',#25530);
#2203=PLANE('',#25532);
#2204=PLANE('',#25533);
#2205=PLANE('',#25534);
#2206=PLANE('',#25536);
#2207=PLANE('',#25537);
#2208=PLANE('',#25538);
#2209=PLANE('',#25540);
#2210=PLANE('',#25541);
#2211=PLANE('',#25542);
#2212=PLANE('',#25544);
#2213=PLANE('',#25545);
#2214=PLANE('',#25546);
#2215=PLANE('',#25548);
#2216=PLANE('',#25549);
#2217=PLANE('',#25550);
#2218=PLANE('',#25552);
#2219=PLANE('',#25553);
#2220=PLANE('',#25554);
#2221=PLANE('',#25556);
#2222=PLANE('',#25557);
#2223=PLANE('',#25597);
#2224=PLANE('',#25598);
#2225=PLANE('',#25599);
#2226=PLANE('',#25604);
#2227=PLANE('',#25605);
#2228=PLANE('',#25606);
#2229=PLANE('',#25607);
#2230=PLANE('',#25608);
#2231=PLANE('',#25609);
#2232=PLANE('',#25610);
#2233=PLANE('',#25611);
#2234=PLANE('',#25618);
#2235=PLANE('',#25619);
#2236=FACE_OUTER_BOUND('',#3564,.T.);
#2237=FACE_OUTER_BOUND('',#3565,.T.);
#2238=FACE_OUTER_BOUND('',#3566,.T.);
#2239=FACE_OUTER_BOUND('',#3567,.T.);
#2240=FACE_OUTER_BOUND('',#3568,.T.);
#2241=FACE_OUTER_BOUND('',#3569,.T.);
#2242=FACE_OUTER_BOUND('',#3570,.T.);
#2243=FACE_OUTER_BOUND('',#3571,.T.);
#2244=FACE_OUTER_BOUND('',#3572,.T.);
#2245=FACE_OUTER_BOUND('',#3573,.T.);
#2246=FACE_OUTER_BOUND('',#3574,.T.);
#2247=FACE_OUTER_BOUND('',#3575,.T.);
#2248=FACE_OUTER_BOUND('',#3576,.T.);
#2249=FACE_OUTER_BOUND('',#3584,.T.);
#2250=FACE_OUTER_BOUND('',#3585,.T.);
#2251=FACE_OUTER_BOUND('',#3586,.T.);
#2252=FACE_OUTER_BOUND('',#3587,.T.);
#2253=FACE_OUTER_BOUND('',#3588,.T.);
#2254=FACE_OUTER_BOUND('',#3589,.T.);
#2255=FACE_OUTER_BOUND('',#3590,.T.);
#2256=FACE_OUTER_BOUND('',#3591,.T.);
#2257=FACE_OUTER_BOUND('',#3592,.T.);
#2258=FACE_OUTER_BOUND('',#3593,.T.);
#2259=FACE_OUTER_BOUND('',#3594,.T.);
#2260=FACE_OUTER_BOUND('',#3595,.T.);
#2261=FACE_OUTER_BOUND('',#3596,.T.);
#2262=FACE_OUTER_BOUND('',#3597,.T.);
#2263=FACE_OUTER_BOUND('',#3598,.T.);
#2264=FACE_OUTER_BOUND('',#3599,.T.);
#2265=FACE_OUTER_BOUND('',#3600,.T.);
#2266=FACE_OUTER_BOUND('',#3601,.T.);
#2267=FACE_OUTER_BOUND('',#3602,.T.);
#2268=FACE_OUTER_BOUND('',#3603,.T.);
#2269=FACE_OUTER_BOUND('',#3604,.T.);
#2270=FACE_OUTER_BOUND('',#3605,.T.);
#2271=FACE_OUTER_BOUND('',#3606,.T.);
#2272=FACE_OUTER_BOUND('',#3607,.T.);
#2273=FACE_OUTER_BOUND('',#3608,.T.);
#2274=FACE_OUTER_BOUND('',#3609,.T.);
#2275=FACE_OUTER_BOUND('',#3610,.T.);
#2276=FACE_OUTER_BOUND('',#3611,.T.);
#2277=FACE_OUTER_BOUND('',#3619,.T.);
#2278=FACE_OUTER_BOUND('',#3620,.T.);
#2279=FACE_OUTER_BOUND('',#3621,.T.);
#2280=FACE_OUTER_BOUND('',#3622,.T.);
#2281=FACE_OUTER_BOUND('',#3623,.T.);
#2282=FACE_OUTER_BOUND('',#3624,.T.);
#2283=FACE_OUTER_BOUND('',#3625,.T.);
#2284=FACE_OUTER_BOUND('',#3626,.T.);
#2285=FACE_OUTER_BOUND('',#3627,.T.);
#2286=FACE_OUTER_BOUND('',#3628,.T.);
#2287=FACE_OUTER_BOUND('',#3629,.T.);
#2288=FACE_OUTER_BOUND('',#3630,.T.);
#2289=FACE_OUTER_BOUND('',#3631,.T.);
#2290=FACE_OUTER_BOUND('',#3632,.T.);
#2291=FACE_OUTER_BOUND('',#3633,.T.);
#2292=FACE_OUTER_BOUND('',#3634,.T.);
#2293=FACE_OUTER_BOUND('',#3635,.T.);
#2294=FACE_OUTER_BOUND('',#3636,.T.);
#2295=FACE_OUTER_BOUND('',#3637,.T.);
#2296=FACE_OUTER_BOUND('',#3638,.T.);
#2297=FACE_OUTER_BOUND('',#3639,.T.);
#2298=FACE_OUTER_BOUND('',#3640,.T.);
#2299=FACE_OUTER_BOUND('',#3641,.T.);
#2300=FACE_OUTER_BOUND('',#3642,.T.);
#2301=FACE_OUTER_BOUND('',#3643,.T.);
#2302=FACE_OUTER_BOUND('',#3644,.T.);
#2303=FACE_OUTER_BOUND('',#3645,.T.);
#2304=FACE_OUTER_BOUND('',#3646,.T.);
#2305=FACE_OUTER_BOUND('',#3647,.T.);
#2306=FACE_OUTER_BOUND('',#3649,.T.);
#2307=FACE_OUTER_BOUND('',#3650,.T.);
#2308=FACE_OUTER_BOUND('',#3651,.T.);
#2309=FACE_OUTER_BOUND('',#3652,.T.);
#2310=FACE_OUTER_BOUND('',#3654,.T.);
#2311=FACE_OUTER_BOUND('',#3655,.T.);
#2312=FACE_OUTER_BOUND('',#3656,.T.);
#2313=FACE_OUTER_BOUND('',#3657,.T.);
#2314=FACE_OUTER_BOUND('',#3659,.T.);
#2315=FACE_OUTER_BOUND('',#3660,.T.);
#2316=FACE_OUTER_BOUND('',#3661,.T.);
#2317=FACE_OUTER_BOUND('',#3662,.T.);
#2318=FACE_OUTER_BOUND('',#3664,.T.);
#2319=FACE_OUTER_BOUND('',#3665,.T.);
#2320=FACE_OUTER_BOUND('',#3666,.T.);
#2321=FACE_OUTER_BOUND('',#3667,.T.);
#2322=FACE_OUTER_BOUND('',#3669,.T.);
#2323=FACE_OUTER_BOUND('',#3670,.T.);
#2324=FACE_OUTER_BOUND('',#3671,.T.);
#2325=FACE_OUTER_BOUND('',#3672,.T.);
#2326=FACE_OUTER_BOUND('',#3674,.T.);
#2327=FACE_OUTER_BOUND('',#3675,.T.);
#2328=FACE_OUTER_BOUND('',#3676,.T.);
#2329=FACE_OUTER_BOUND('',#3677,.T.);
#2330=FACE_OUTER_BOUND('',#3679,.T.);
#2331=FACE_OUTER_BOUND('',#3680,.T.);
#2332=FACE_OUTER_BOUND('',#3681,.T.);
#2333=FACE_OUTER_BOUND('',#3682,.T.);
#2334=FACE_OUTER_BOUND('',#3683,.T.);
#2335=FACE_OUTER_BOUND('',#3684,.T.);
#2336=FACE_OUTER_BOUND('',#3685,.T.);
#2337=FACE_OUTER_BOUND('',#3686,.T.);
#2338=FACE_OUTER_BOUND('',#3687,.T.);
#2339=FACE_OUTER_BOUND('',#3688,.T.);
#2340=FACE_OUTER_BOUND('',#3689,.T.);
#2341=FACE_OUTER_BOUND('',#3690,.T.);
#2342=FACE_OUTER_BOUND('',#3691,.T.);
#2343=FACE_OUTER_BOUND('',#3692,.T.);
#2344=FACE_OUTER_BOUND('',#3693,.T.);
#2345=FACE_OUTER_BOUND('',#3694,.T.);
#2346=FACE_OUTER_BOUND('',#3702,.T.);
#2347=FACE_OUTER_BOUND('',#3703,.T.);
#2348=FACE_OUTER_BOUND('',#3707,.T.);
#2349=FACE_OUTER_BOUND('',#3708,.T.);
#2350=FACE_OUTER_BOUND('',#3709,.T.);
#2351=FACE_OUTER_BOUND('',#3710,.T.);
#2352=FACE_OUTER_BOUND('',#3711,.T.);
#2353=FACE_OUTER_BOUND('',#3712,.T.);
#2354=FACE_OUTER_BOUND('',#3713,.T.);
#2355=FACE_OUTER_BOUND('',#3714,.T.);
#2356=FACE_OUTER_BOUND('',#3715,.T.);
#2357=FACE_OUTER_BOUND('',#3716,.T.);
#2358=FACE_OUTER_BOUND('',#3717,.T.);
#2359=FACE_OUTER_BOUND('',#3718,.T.);
#2360=FACE_OUTER_BOUND('',#3719,.T.);
#2361=FACE_OUTER_BOUND('',#3720,.T.);
#2362=FACE_OUTER_BOUND('',#3721,.T.);
#2363=FACE_OUTER_BOUND('',#3722,.T.);
#2364=FACE_OUTER_BOUND('',#3723,.T.);
#2365=FACE_OUTER_BOUND('',#3724,.T.);
#2366=FACE_OUTER_BOUND('',#3725,.T.);
#2367=FACE_OUTER_BOUND('',#3726,.T.);
#2368=FACE_OUTER_BOUND('',#3727,.T.);
#2369=FACE_OUTER_BOUND('',#3728,.T.);
#2370=FACE_OUTER_BOUND('',#3729,.T.);
#2371=FACE_OUTER_BOUND('',#3730,.T.);
#2372=FACE_OUTER_BOUND('',#3731,.T.);
#2373=FACE_OUTER_BOUND('',#3732,.T.);
#2374=FACE_OUTER_BOUND('',#3733,.T.);
#2375=FACE_OUTER_BOUND('',#3734,.T.);
#2376=FACE_OUTER_BOUND('',#3735,.T.);
#2377=FACE_OUTER_BOUND('',#3736,.T.);
#2378=FACE_OUTER_BOUND('',#3737,.T.);
#2379=FACE_OUTER_BOUND('',#3748,.T.);
#2380=FACE_OUTER_BOUND('',#3749,.T.);
#2381=FACE_OUTER_BOUND('',#3750,.T.);
#2382=FACE_OUTER_BOUND('',#3751,.T.);
#2383=FACE_OUTER_BOUND('',#3752,.T.);
#2384=FACE_OUTER_BOUND('',#3753,.T.);
#2385=FACE_OUTER_BOUND('',#3755,.T.);
#2386=FACE_OUTER_BOUND('',#3756,.T.);
#2387=FACE_OUTER_BOUND('',#3757,.T.);
#2388=FACE_OUTER_BOUND('',#3758,.T.);
#2389=FACE_OUTER_BOUND('',#3759,.T.);
#2390=FACE_OUTER_BOUND('',#3760,.T.);
#2391=FACE_OUTER_BOUND('',#3761,.T.);
#2392=FACE_OUTER_BOUND('',#3762,.T.);
#2393=FACE_OUTER_BOUND('',#3763,.T.);
#2394=FACE_OUTER_BOUND('',#3764,.T.);
#2395=FACE_OUTER_BOUND('',#3765,.T.);
#2396=FACE_OUTER_BOUND('',#3766,.T.);
#2397=FACE_OUTER_BOUND('',#3767,.T.);
#2398=FACE_OUTER_BOUND('',#3768,.T.);
#2399=FACE_OUTER_BOUND('',#3769,.T.);
#2400=FACE_OUTER_BOUND('',#3770,.T.);
#2401=FACE_OUTER_BOUND('',#3771,.T.);
#2402=FACE_OUTER_BOUND('',#3772,.T.);
#2403=FACE_OUTER_BOUND('',#3774,.T.);
#2404=FACE_OUTER_BOUND('',#3775,.T.);
#2405=FACE_OUTER_BOUND('',#3776,.T.);
#2406=FACE_OUTER_BOUND('',#3777,.T.);
#2407=FACE_OUTER_BOUND('',#3778,.T.);
#2408=FACE_OUTER_BOUND('',#3779,.T.);
#2409=FACE_OUTER_BOUND('',#3780,.T.);
#2410=FACE_OUTER_BOUND('',#3781,.T.);
#2411=FACE_OUTER_BOUND('',#3782,.T.);
#2412=FACE_OUTER_BOUND('',#3783,.T.);
#2413=FACE_OUTER_BOUND('',#3784,.T.);
#2414=FACE_OUTER_BOUND('',#3785,.T.);
#2415=FACE_OUTER_BOUND('',#3786,.T.);
#2416=FACE_OUTER_BOUND('',#3787,.T.);
#2417=FACE_OUTER_BOUND('',#3788,.T.);
#2418=FACE_OUTER_BOUND('',#3789,.T.);
#2419=FACE_OUTER_BOUND('',#3790,.T.);
#2420=FACE_OUTER_BOUND('',#3791,.T.);
#2421=FACE_OUTER_BOUND('',#3792,.T.);
#2422=FACE_OUTER_BOUND('',#3793,.T.);
#2423=FACE_OUTER_BOUND('',#3794,.T.);
#2424=FACE_OUTER_BOUND('',#3795,.T.);
#2425=FACE_OUTER_BOUND('',#3796,.T.);
#2426=FACE_OUTER_BOUND('',#3797,.T.);
#2427=FACE_OUTER_BOUND('',#3798,.T.);
#2428=FACE_OUTER_BOUND('',#3799,.T.);
#2429=FACE_OUTER_BOUND('',#3800,.T.);
#2430=FACE_OUTER_BOUND('',#3801,.T.);
#2431=FACE_OUTER_BOUND('',#3802,.T.);
#2432=FACE_OUTER_BOUND('',#3803,.T.);
#2433=FACE_OUTER_BOUND('',#3804,.T.);
#2434=FACE_OUTER_BOUND('',#3805,.T.);
#2435=FACE_OUTER_BOUND('',#3806,.T.);
#2436=FACE_OUTER_BOUND('',#3807,.T.);
#2437=FACE_OUTER_BOUND('',#3808,.T.);
#2438=FACE_OUTER_BOUND('',#3809,.T.);
#2439=FACE_OUTER_BOUND('',#3810,.T.);
#2440=FACE_OUTER_BOUND('',#3811,.T.);
#2441=FACE_OUTER_BOUND('',#3812,.T.);
#2442=FACE_OUTER_BOUND('',#3817,.T.);
#2443=FACE_OUTER_BOUND('',#3818,.T.);
#2444=FACE_OUTER_BOUND('',#3819,.T.);
#2445=FACE_OUTER_BOUND('',#3820,.T.);
#2446=FACE_OUTER_BOUND('',#3821,.T.);
#2447=FACE_OUTER_BOUND('',#3822,.T.);
#2448=FACE_OUTER_BOUND('',#3823,.T.);
#2449=FACE_OUTER_BOUND('',#3824,.T.);
#2450=FACE_OUTER_BOUND('',#3825,.T.);
#2451=FACE_OUTER_BOUND('',#3826,.T.);
#2452=FACE_OUTER_BOUND('',#3827,.T.);
#2453=FACE_OUTER_BOUND('',#3828,.T.);
#2454=FACE_OUTER_BOUND('',#3829,.T.);
#2455=FACE_OUTER_BOUND('',#3830,.T.);
#2456=FACE_OUTER_BOUND('',#3831,.T.);
#2457=FACE_OUTER_BOUND('',#3832,.T.);
#2458=FACE_OUTER_BOUND('',#3833,.T.);
#2459=FACE_OUTER_BOUND('',#3834,.T.);
#2460=FACE_OUTER_BOUND('',#3835,.T.);
#2461=FACE_OUTER_BOUND('',#3836,.T.);
#2462=FACE_OUTER_BOUND('',#3837,.T.);
#2463=FACE_OUTER_BOUND('',#3838,.T.);
#2464=FACE_OUTER_BOUND('',#3839,.T.);
#2465=FACE_OUTER_BOUND('',#3840,.T.);
#2466=FACE_OUTER_BOUND('',#3841,.T.);
#2467=FACE_OUTER_BOUND('',#3842,.T.);
#2468=FACE_OUTER_BOUND('',#3843,.T.);
#2469=FACE_OUTER_BOUND('',#3844,.T.);
#2470=FACE_OUTER_BOUND('',#3845,.T.);
#2471=FACE_OUTER_BOUND('',#3846,.T.);
#2472=FACE_OUTER_BOUND('',#3847,.T.);
#2473=FACE_OUTER_BOUND('',#3848,.T.);
#2474=FACE_OUTER_BOUND('',#3849,.T.);
#2475=FACE_OUTER_BOUND('',#3850,.T.);
#2476=FACE_OUTER_BOUND('',#3851,.T.);
#2477=FACE_OUTER_BOUND('',#3852,.T.);
#2478=FACE_OUTER_BOUND('',#3853,.T.);
#2479=FACE_OUTER_BOUND('',#3854,.T.);
#2480=FACE_OUTER_BOUND('',#3855,.T.);
#2481=FACE_OUTER_BOUND('',#3856,.T.);
#2482=FACE_OUTER_BOUND('',#3858,.T.);
#2483=FACE_OUTER_BOUND('',#3859,.T.);
#2484=FACE_OUTER_BOUND('',#3860,.T.);
#2485=FACE_OUTER_BOUND('',#3862,.T.);
#2486=FACE_OUTER_BOUND('',#3863,.T.);
#2487=FACE_OUTER_BOUND('',#3864,.T.);
#2488=FACE_OUTER_BOUND('',#3865,.T.);
#2489=FACE_OUTER_BOUND('',#3866,.T.);
#2490=FACE_OUTER_BOUND('',#3867,.T.);
#2491=FACE_OUTER_BOUND('',#3868,.T.);
#2492=FACE_OUTER_BOUND('',#3869,.T.);
#2493=FACE_OUTER_BOUND('',#3870,.T.);
#2494=FACE_OUTER_BOUND('',#3871,.T.);
#2495=FACE_OUTER_BOUND('',#3872,.T.);
#2496=FACE_OUTER_BOUND('',#3873,.T.);
#2497=FACE_OUTER_BOUND('',#3874,.T.);
#2498=FACE_OUTER_BOUND('',#3875,.T.);
#2499=FACE_OUTER_BOUND('',#3876,.T.);
#2500=FACE_OUTER_BOUND('',#3877,.T.);
#2501=FACE_OUTER_BOUND('',#3878,.T.);
#2502=FACE_OUTER_BOUND('',#3879,.T.);
#2503=FACE_OUTER_BOUND('',#3880,.T.);
#2504=FACE_OUTER_BOUND('',#3881,.T.);
#2505=FACE_OUTER_BOUND('',#3882,.T.);
#2506=FACE_OUTER_BOUND('',#3883,.T.);
#2507=FACE_OUTER_BOUND('',#3884,.T.);
#2508=FACE_OUTER_BOUND('',#3885,.T.);
#2509=FACE_OUTER_BOUND('',#3886,.T.);
#2510=FACE_OUTER_BOUND('',#3887,.T.);
#2511=FACE_OUTER_BOUND('',#3892,.T.);
#2512=FACE_OUTER_BOUND('',#3893,.T.);
#2513=FACE_OUTER_BOUND('',#3894,.T.);
#2514=FACE_OUTER_BOUND('',#3895,.T.);
#2515=FACE_OUTER_BOUND('',#3897,.T.);
#2516=FACE_OUTER_BOUND('',#3898,.T.);
#2517=FACE_OUTER_BOUND('',#3899,.T.);
#2518=FACE_OUTER_BOUND('',#3900,.T.);
#2519=FACE_OUTER_BOUND('',#3901,.T.);
#2520=FACE_OUTER_BOUND('',#3902,.T.);
#2521=FACE_OUTER_BOUND('',#3903,.T.);
#2522=FACE_OUTER_BOUND('',#3904,.T.);
#2523=FACE_OUTER_BOUND('',#3905,.T.);
#2524=FACE_OUTER_BOUND('',#3906,.T.);
#2525=FACE_OUTER_BOUND('',#3907,.T.);
#2526=FACE_OUTER_BOUND('',#3908,.T.);
#2527=FACE_OUTER_BOUND('',#3909,.T.);
#2528=FACE_OUTER_BOUND('',#3910,.T.);
#2529=FACE_OUTER_BOUND('',#3911,.T.);
#2530=FACE_OUTER_BOUND('',#3912,.T.);
#2531=FACE_OUTER_BOUND('',#3913,.T.);
#2532=FACE_OUTER_BOUND('',#3921,.T.);
#2533=FACE_OUTER_BOUND('',#3922,.T.);
#2534=FACE_OUTER_BOUND('',#3930,.T.);
#2535=FACE_OUTER_BOUND('',#3931,.T.);
#2536=FACE_OUTER_BOUND('',#3932,.T.);
#2537=FACE_OUTER_BOUND('',#3933,.T.);
#2538=FACE_OUTER_BOUND('',#3934,.T.);
#2539=FACE_OUTER_BOUND('',#3935,.T.);
#2540=FACE_OUTER_BOUND('',#3936,.T.);
#2541=FACE_OUTER_BOUND('',#3937,.T.);
#2542=FACE_OUTER_BOUND('',#3938,.T.);
#2543=FACE_OUTER_BOUND('',#3939,.T.);
#2544=FACE_OUTER_BOUND('',#3940,.T.);
#2545=FACE_OUTER_BOUND('',#3941,.T.);
#2546=FACE_OUTER_BOUND('',#3942,.T.);
#2547=FACE_OUTER_BOUND('',#3943,.T.);
#2548=FACE_OUTER_BOUND('',#3944,.T.);
#2549=FACE_OUTER_BOUND('',#3945,.T.);
#2550=FACE_OUTER_BOUND('',#3946,.T.);
#2551=FACE_OUTER_BOUND('',#3947,.T.);
#2552=FACE_OUTER_BOUND('',#3948,.T.);
#2553=FACE_OUTER_BOUND('',#3949,.T.);
#2554=FACE_OUTER_BOUND('',#3950,.T.);
#2555=FACE_OUTER_BOUND('',#3951,.T.);
#2556=FACE_OUTER_BOUND('',#3952,.T.);
#2557=FACE_OUTER_BOUND('',#3953,.T.);
#2558=FACE_OUTER_BOUND('',#3954,.T.);
#2559=FACE_OUTER_BOUND('',#3955,.T.);
#2560=FACE_OUTER_BOUND('',#3956,.T.);
#2561=FACE_OUTER_BOUND('',#3957,.T.);
#2562=FACE_OUTER_BOUND('',#3958,.T.);
#2563=FACE_OUTER_BOUND('',#3959,.T.);
#2564=FACE_OUTER_BOUND('',#3960,.T.);
#2565=FACE_OUTER_BOUND('',#3961,.T.);
#2566=FACE_OUTER_BOUND('',#3962,.T.);
#2567=FACE_OUTER_BOUND('',#3963,.T.);
#2568=FACE_OUTER_BOUND('',#3964,.T.);
#2569=FACE_OUTER_BOUND('',#3965,.T.);
#2570=FACE_OUTER_BOUND('',#3966,.T.);
#2571=FACE_OUTER_BOUND('',#3967,.T.);
#2572=FACE_OUTER_BOUND('',#3968,.T.);
#2573=FACE_OUTER_BOUND('',#3969,.T.);
#2574=FACE_OUTER_BOUND('',#3970,.T.);
#2575=FACE_OUTER_BOUND('',#3971,.T.);
#2576=FACE_OUTER_BOUND('',#3972,.T.);
#2577=FACE_OUTER_BOUND('',#3973,.T.);
#2578=FACE_OUTER_BOUND('',#3974,.T.);
#2579=FACE_OUTER_BOUND('',#3975,.T.);
#2580=FACE_OUTER_BOUND('',#3976,.T.);
#2581=FACE_OUTER_BOUND('',#3977,.T.);
#2582=FACE_OUTER_BOUND('',#3978,.T.);
#2583=FACE_OUTER_BOUND('',#3979,.T.);
#2584=FACE_OUTER_BOUND('',#3980,.T.);
#2585=FACE_OUTER_BOUND('',#3981,.T.);
#2586=FACE_OUTER_BOUND('',#3982,.T.);
#2587=FACE_OUTER_BOUND('',#3983,.T.);
#2588=FACE_OUTER_BOUND('',#3984,.T.);
#2589=FACE_OUTER_BOUND('',#3985,.T.);
#2590=FACE_OUTER_BOUND('',#3986,.T.);
#2591=FACE_OUTER_BOUND('',#3987,.T.);
#2592=FACE_OUTER_BOUND('',#3988,.T.);
#2593=FACE_OUTER_BOUND('',#3989,.T.);
#2594=FACE_OUTER_BOUND('',#3990,.T.);
#2595=FACE_OUTER_BOUND('',#3991,.T.);
#2596=FACE_OUTER_BOUND('',#3992,.T.);
#2597=FACE_OUTER_BOUND('',#3993,.T.);
#2598=FACE_OUTER_BOUND('',#3994,.T.);
#2599=FACE_OUTER_BOUND('',#3995,.T.);
#2600=FACE_OUTER_BOUND('',#3996,.T.);
#2601=FACE_OUTER_BOUND('',#3997,.T.);
#2602=FACE_OUTER_BOUND('',#3998,.T.);
#2603=FACE_OUTER_BOUND('',#3999,.T.);
#2604=FACE_OUTER_BOUND('',#4000,.T.);
#2605=FACE_OUTER_BOUND('',#4001,.T.);
#2606=FACE_OUTER_BOUND('',#4002,.T.);
#2607=FACE_OUTER_BOUND('',#4003,.T.);
#2608=FACE_OUTER_BOUND('',#4004,.T.);
#2609=FACE_OUTER_BOUND('',#4005,.T.);
#2610=FACE_OUTER_BOUND('',#4006,.T.);
#2611=FACE_OUTER_BOUND('',#4007,.T.);
#2612=FACE_OUTER_BOUND('',#4008,.T.);
#2613=FACE_OUTER_BOUND('',#4009,.T.);
#2614=FACE_OUTER_BOUND('',#4010,.T.);
#2615=FACE_OUTER_BOUND('',#4011,.T.);
#2616=FACE_OUTER_BOUND('',#4012,.T.);
#2617=FACE_OUTER_BOUND('',#4013,.T.);
#2618=FACE_OUTER_BOUND('',#4014,.T.);
#2619=FACE_OUTER_BOUND('',#4015,.T.);
#2620=FACE_OUTER_BOUND('',#4016,.T.);
#2621=FACE_OUTER_BOUND('',#4017,.T.);
#2622=FACE_OUTER_BOUND('',#4018,.T.);
#2623=FACE_OUTER_BOUND('',#4019,.T.);
#2624=FACE_OUTER_BOUND('',#4020,.T.);
#2625=FACE_OUTER_BOUND('',#4021,.T.);
#2626=FACE_OUTER_BOUND('',#4022,.T.);
#2627=FACE_OUTER_BOUND('',#4023,.T.);
#2628=FACE_OUTER_BOUND('',#4024,.T.);
#2629=FACE_OUTER_BOUND('',#4025,.T.);
#2630=FACE_OUTER_BOUND('',#4026,.T.);
#2631=FACE_OUTER_BOUND('',#4027,.T.);
#2632=FACE_OUTER_BOUND('',#4028,.T.);
#2633=FACE_OUTER_BOUND('',#4029,.T.);
#2634=FACE_OUTER_BOUND('',#4030,.T.);
#2635=FACE_OUTER_BOUND('',#4031,.T.);
#2636=FACE_OUTER_BOUND('',#4032,.T.);
#2637=FACE_OUTER_BOUND('',#4033,.T.);
#2638=FACE_OUTER_BOUND('',#4034,.T.);
#2639=FACE_OUTER_BOUND('',#4035,.T.);
#2640=FACE_OUTER_BOUND('',#4036,.T.);
#2641=FACE_OUTER_BOUND('',#4037,.T.);
#2642=FACE_OUTER_BOUND('',#4038,.T.);
#2643=FACE_OUTER_BOUND('',#4039,.T.);
#2644=FACE_OUTER_BOUND('',#4040,.T.);
#2645=FACE_OUTER_BOUND('',#4041,.T.);
#2646=FACE_OUTER_BOUND('',#4042,.T.);
#2647=FACE_OUTER_BOUND('',#4043,.T.);
#2648=FACE_OUTER_BOUND('',#4044,.T.);
#2649=FACE_OUTER_BOUND('',#4045,.T.);
#2650=FACE_OUTER_BOUND('',#4046,.T.);
#2651=FACE_OUTER_BOUND('',#4047,.T.);
#2652=FACE_OUTER_BOUND('',#4048,.T.);
#2653=FACE_OUTER_BOUND('',#4049,.T.);
#2654=FACE_OUTER_BOUND('',#4050,.T.);
#2655=FACE_OUTER_BOUND('',#4051,.T.);
#2656=FACE_OUTER_BOUND('',#4052,.T.);
#2657=FACE_OUTER_BOUND('',#4053,.T.);
#2658=FACE_OUTER_BOUND('',#4054,.T.);
#2659=FACE_OUTER_BOUND('',#4055,.T.);
#2660=FACE_OUTER_BOUND('',#4056,.T.);
#2661=FACE_OUTER_BOUND('',#4057,.T.);
#2662=FACE_OUTER_BOUND('',#4058,.T.);
#2663=FACE_OUTER_BOUND('',#4059,.T.);
#2664=FACE_OUTER_BOUND('',#4060,.T.);
#2665=FACE_OUTER_BOUND('',#4061,.T.);
#2666=FACE_OUTER_BOUND('',#4062,.T.);
#2667=FACE_OUTER_BOUND('',#4063,.T.);
#2668=FACE_OUTER_BOUND('',#4064,.T.);
#2669=FACE_OUTER_BOUND('',#4065,.T.);
#2670=FACE_OUTER_BOUND('',#4066,.T.);
#2671=FACE_OUTER_BOUND('',#4067,.T.);
#2672=FACE_OUTER_BOUND('',#4068,.T.);
#2673=FACE_OUTER_BOUND('',#4069,.T.);
#2674=FACE_OUTER_BOUND('',#4070,.T.);
#2675=FACE_OUTER_BOUND('',#4071,.T.);
#2676=FACE_OUTER_BOUND('',#4072,.T.);
#2677=FACE_OUTER_BOUND('',#4073,.T.);
#2678=FACE_OUTER_BOUND('',#4074,.T.);
#2679=FACE_OUTER_BOUND('',#4075,.T.);
#2680=FACE_OUTER_BOUND('',#4076,.T.);
#2681=FACE_OUTER_BOUND('',#4077,.T.);
#2682=FACE_OUTER_BOUND('',#4078,.T.);
#2683=FACE_OUTER_BOUND('',#4079,.T.);
#2684=FACE_OUTER_BOUND('',#4081,.T.);
#2685=FACE_OUTER_BOUND('',#4082,.T.);
#2686=FACE_OUTER_BOUND('',#4106,.T.);
#2687=FACE_OUTER_BOUND('',#4108,.T.);
#2688=FACE_OUTER_BOUND('',#4109,.T.);
#2689=FACE_OUTER_BOUND('',#4110,.T.);
#2690=FACE_OUTER_BOUND('',#4112,.T.);
#2691=FACE_OUTER_BOUND('',#4113,.T.);
#2692=FACE_OUTER_BOUND('',#4114,.T.);
#2693=FACE_OUTER_BOUND('',#4115,.T.);
#2694=FACE_OUTER_BOUND('',#4116,.T.);
#2695=FACE_OUTER_BOUND('',#4117,.T.);
#2696=FACE_OUTER_BOUND('',#4118,.T.);
#2697=FACE_OUTER_BOUND('',#4120,.T.);
#2698=FACE_OUTER_BOUND('',#4126,.T.);
#2699=FACE_OUTER_BOUND('',#4127,.T.);
#2700=FACE_OUTER_BOUND('',#4128,.T.);
#2701=FACE_OUTER_BOUND('',#4129,.T.);
#2702=FACE_OUTER_BOUND('',#4130,.T.);
#2703=FACE_OUTER_BOUND('',#4136,.T.);
#2704=FACE_OUTER_BOUND('',#4137,.T.);
#2705=FACE_OUTER_BOUND('',#4138,.T.);
#2706=FACE_OUTER_BOUND('',#4139,.T.);
#2707=FACE_OUTER_BOUND('',#4140,.T.);
#2708=FACE_OUTER_BOUND('',#4141,.T.);
#2709=FACE_OUTER_BOUND('',#4142,.T.);
#2710=FACE_OUTER_BOUND('',#4143,.T.);
#2711=FACE_OUTER_BOUND('',#4144,.T.);
#2712=FACE_OUTER_BOUND('',#4145,.T.);
#2713=FACE_OUTER_BOUND('',#4147,.T.);
#2714=FACE_OUTER_BOUND('',#4149,.T.);
#2715=FACE_OUTER_BOUND('',#4150,.T.);
#2716=FACE_OUTER_BOUND('',#4151,.T.);
#2717=FACE_OUTER_BOUND('',#4153,.T.);
#2718=FACE_OUTER_BOUND('',#4155,.T.);
#2719=FACE_OUTER_BOUND('',#4156,.T.);
#2720=FACE_OUTER_BOUND('',#4157,.T.);
#2721=FACE_OUTER_BOUND('',#4158,.T.);
#2722=FACE_OUTER_BOUND('',#4160,.T.);
#2723=FACE_OUTER_BOUND('',#4161,.T.);
#2724=FACE_OUTER_BOUND('',#4163,.T.);
#2725=FACE_OUTER_BOUND('',#4164,.T.);
#2726=FACE_OUTER_BOUND('',#4165,.T.);
#2727=FACE_OUTER_BOUND('',#4166,.T.);
#2728=FACE_OUTER_BOUND('',#4167,.T.);
#2729=FACE_OUTER_BOUND('',#4168,.T.);
#2730=FACE_OUTER_BOUND('',#4170,.T.);
#2731=FACE_OUTER_BOUND('',#4171,.T.);
#2732=FACE_OUTER_BOUND('',#4172,.T.);
#2733=FACE_OUTER_BOUND('',#4173,.T.);
#2734=FACE_OUTER_BOUND('',#4174,.T.);
#2735=FACE_OUTER_BOUND('',#4175,.T.);
#2736=FACE_OUTER_BOUND('',#4176,.T.);
#2737=FACE_OUTER_BOUND('',#4177,.T.);
#2738=FACE_OUTER_BOUND('',#4178,.T.);
#2739=FACE_OUTER_BOUND('',#4179,.T.);
#2740=FACE_OUTER_BOUND('',#4180,.T.);
#2741=FACE_OUTER_BOUND('',#4181,.T.);
#2742=FACE_OUTER_BOUND('',#4182,.T.);
#2743=FACE_OUTER_BOUND('',#4183,.T.);
#2744=FACE_OUTER_BOUND('',#4184,.T.);
#2745=FACE_OUTER_BOUND('',#4185,.T.);
#2746=FACE_OUTER_BOUND('',#4186,.T.);
#2747=FACE_OUTER_BOUND('',#4187,.T.);
#2748=FACE_OUTER_BOUND('',#4188,.T.);
#2749=FACE_OUTER_BOUND('',#4189,.T.);
#2750=FACE_OUTER_BOUND('',#4190,.T.);
#2751=FACE_OUTER_BOUND('',#4191,.T.);
#2752=FACE_OUTER_BOUND('',#4192,.T.);
#2753=FACE_OUTER_BOUND('',#4193,.T.);
#2754=FACE_OUTER_BOUND('',#4194,.T.);
#2755=FACE_OUTER_BOUND('',#4195,.T.);
#2756=FACE_OUTER_BOUND('',#4196,.T.);
#2757=FACE_OUTER_BOUND('',#4197,.T.);
#2758=FACE_OUTER_BOUND('',#4198,.T.);
#2759=FACE_OUTER_BOUND('',#4199,.T.);
#2760=FACE_OUTER_BOUND('',#4200,.T.);
#2761=FACE_OUTER_BOUND('',#4201,.T.);
#2762=FACE_OUTER_BOUND('',#4202,.T.);
#2763=FACE_OUTER_BOUND('',#4203,.T.);
#2764=FACE_OUTER_BOUND('',#4204,.T.);
#2765=FACE_OUTER_BOUND('',#4205,.T.);
#2766=FACE_OUTER_BOUND('',#4206,.T.);
#2767=FACE_OUTER_BOUND('',#4207,.T.);
#2768=FACE_OUTER_BOUND('',#4208,.T.);
#2769=FACE_OUTER_BOUND('',#4209,.T.);
#2770=FACE_OUTER_BOUND('',#4210,.T.);
#2771=FACE_OUTER_BOUND('',#4211,.T.);
#2772=FACE_OUTER_BOUND('',#4212,.T.);
#2773=FACE_OUTER_BOUND('',#4213,.T.);
#2774=FACE_OUTER_BOUND('',#4214,.T.);
#2775=FACE_OUTER_BOUND('',#4215,.T.);
#2776=FACE_OUTER_BOUND('',#4216,.T.);
#2777=FACE_OUTER_BOUND('',#4217,.T.);
#2778=FACE_OUTER_BOUND('',#4218,.T.);
#2779=FACE_OUTER_BOUND('',#4219,.T.);
#2780=FACE_OUTER_BOUND('',#4220,.T.);
#2781=FACE_OUTER_BOUND('',#4221,.T.);
#2782=FACE_OUTER_BOUND('',#4222,.T.);
#2783=FACE_OUTER_BOUND('',#4223,.T.);
#2784=FACE_OUTER_BOUND('',#4224,.T.);
#2785=FACE_OUTER_BOUND('',#4225,.T.);
#2786=FACE_OUTER_BOUND('',#4226,.T.);
#2787=FACE_OUTER_BOUND('',#4227,.T.);
#2788=FACE_OUTER_BOUND('',#4228,.T.);
#2789=FACE_OUTER_BOUND('',#4229,.T.);
#2790=FACE_OUTER_BOUND('',#4230,.T.);
#2791=FACE_OUTER_BOUND('',#4231,.T.);
#2792=FACE_OUTER_BOUND('',#4232,.T.);
#2793=FACE_OUTER_BOUND('',#4233,.T.);
#2794=FACE_OUTER_BOUND('',#4234,.T.);
#2795=FACE_OUTER_BOUND('',#4235,.T.);
#2796=FACE_OUTER_BOUND('',#4236,.T.);
#2797=FACE_OUTER_BOUND('',#4237,.T.);
#2798=FACE_OUTER_BOUND('',#4238,.T.);
#2799=FACE_OUTER_BOUND('',#4239,.T.);
#2800=FACE_OUTER_BOUND('',#4240,.T.);
#2801=FACE_OUTER_BOUND('',#4241,.T.);
#2802=FACE_OUTER_BOUND('',#4242,.T.);
#2803=FACE_OUTER_BOUND('',#4243,.T.);
#2804=FACE_OUTER_BOUND('',#4244,.T.);
#2805=FACE_OUTER_BOUND('',#4246,.T.);
#2806=FACE_OUTER_BOUND('',#4248,.T.);
#2807=FACE_OUTER_BOUND('',#4249,.T.);
#2808=FACE_OUTER_BOUND('',#4250,.T.);
#2809=FACE_OUTER_BOUND('',#4251,.T.);
#2810=FACE_OUTER_BOUND('',#4253,.T.);
#2811=FACE_OUTER_BOUND('',#4271,.T.);
#2812=FACE_OUTER_BOUND('',#4273,.T.);
#2813=FACE_OUTER_BOUND('',#4274,.T.);
#2814=FACE_OUTER_BOUND('',#4275,.T.);
#2815=FACE_OUTER_BOUND('',#4276,.T.);
#2816=FACE_OUTER_BOUND('',#4278,.T.);
#2817=FACE_OUTER_BOUND('',#4279,.T.);
#2818=FACE_OUTER_BOUND('',#4281,.T.);
#2819=FACE_OUTER_BOUND('',#4282,.T.);
#2820=FACE_OUTER_BOUND('',#4283,.T.);
#2821=FACE_OUTER_BOUND('',#4285,.T.);
#2822=FACE_OUTER_BOUND('',#4286,.T.);
#2823=FACE_OUTER_BOUND('',#4288,.T.);
#2824=FACE_OUTER_BOUND('',#4289,.T.);
#2825=FACE_OUTER_BOUND('',#4290,.T.);
#2826=FACE_OUTER_BOUND('',#4291,.T.);
#2827=FACE_OUTER_BOUND('',#4292,.T.);
#2828=FACE_OUTER_BOUND('',#4293,.T.);
#2829=FACE_OUTER_BOUND('',#4294,.T.);
#2830=FACE_OUTER_BOUND('',#4295,.T.);
#2831=FACE_OUTER_BOUND('',#4296,.T.);
#2832=FACE_OUTER_BOUND('',#4297,.T.);
#2833=FACE_OUTER_BOUND('',#4298,.T.);
#2834=FACE_OUTER_BOUND('',#4299,.T.);
#2835=FACE_OUTER_BOUND('',#4300,.T.);
#2836=FACE_OUTER_BOUND('',#4301,.T.);
#2837=FACE_OUTER_BOUND('',#4302,.T.);
#2838=FACE_OUTER_BOUND('',#4303,.T.);
#2839=FACE_OUTER_BOUND('',#4304,.T.);
#2840=FACE_OUTER_BOUND('',#4305,.T.);
#2841=FACE_OUTER_BOUND('',#4306,.T.);
#2842=FACE_OUTER_BOUND('',#4307,.T.);
#2843=FACE_OUTER_BOUND('',#4308,.T.);
#2844=FACE_OUTER_BOUND('',#4309,.T.);
#2845=FACE_OUTER_BOUND('',#4310,.T.);
#2846=FACE_OUTER_BOUND('',#4311,.T.);
#2847=FACE_OUTER_BOUND('',#4312,.T.);
#2848=FACE_OUTER_BOUND('',#4313,.T.);
#2849=FACE_OUTER_BOUND('',#4314,.T.);
#2850=FACE_OUTER_BOUND('',#4315,.T.);
#2851=FACE_OUTER_BOUND('',#4316,.T.);
#2852=FACE_OUTER_BOUND('',#4317,.T.);
#2853=FACE_OUTER_BOUND('',#4318,.T.);
#2854=FACE_OUTER_BOUND('',#4319,.T.);
#2855=FACE_OUTER_BOUND('',#4320,.T.);
#2856=FACE_OUTER_BOUND('',#4321,.T.);
#2857=FACE_OUTER_BOUND('',#4322,.T.);
#2858=FACE_OUTER_BOUND('',#4323,.T.);
#2859=FACE_OUTER_BOUND('',#4324,.T.);
#2860=FACE_OUTER_BOUND('',#4325,.T.);
#2861=FACE_OUTER_BOUND('',#4326,.T.);
#2862=FACE_OUTER_BOUND('',#4327,.T.);
#2863=FACE_OUTER_BOUND('',#4328,.T.);
#2864=FACE_OUTER_BOUND('',#4329,.T.);
#2865=FACE_OUTER_BOUND('',#4330,.T.);
#2866=FACE_OUTER_BOUND('',#4331,.T.);
#2867=FACE_OUTER_BOUND('',#4332,.T.);
#2868=FACE_OUTER_BOUND('',#4333,.T.);
#2869=FACE_OUTER_BOUND('',#4334,.T.);
#2870=FACE_OUTER_BOUND('',#4335,.T.);
#2871=FACE_OUTER_BOUND('',#4336,.T.);
#2872=FACE_OUTER_BOUND('',#4337,.T.);
#2873=FACE_OUTER_BOUND('',#4338,.T.);
#2874=FACE_OUTER_BOUND('',#4339,.T.);
#2875=FACE_OUTER_BOUND('',#4340,.T.);
#2876=FACE_OUTER_BOUND('',#4341,.T.);
#2877=FACE_OUTER_BOUND('',#4342,.T.);
#2878=FACE_OUTER_BOUND('',#4343,.T.);
#2879=FACE_OUTER_BOUND('',#4344,.T.);
#2880=FACE_OUTER_BOUND('',#4345,.T.);
#2881=FACE_OUTER_BOUND('',#4346,.T.);
#2882=FACE_OUTER_BOUND('',#4347,.T.);
#2883=FACE_OUTER_BOUND('',#4348,.T.);
#2884=FACE_OUTER_BOUND('',#4349,.T.);
#2885=FACE_OUTER_BOUND('',#4350,.T.);
#2886=FACE_OUTER_BOUND('',#4351,.T.);
#2887=FACE_OUTER_BOUND('',#4352,.T.);
#2888=FACE_OUTER_BOUND('',#4353,.T.);
#2889=FACE_OUTER_BOUND('',#4354,.T.);
#2890=FACE_OUTER_BOUND('',#4355,.T.);
#2891=FACE_OUTER_BOUND('',#4356,.T.);
#2892=FACE_OUTER_BOUND('',#4357,.T.);
#2893=FACE_OUTER_BOUND('',#4358,.T.);
#2894=FACE_OUTER_BOUND('',#4359,.T.);
#2895=FACE_OUTER_BOUND('',#4360,.T.);
#2896=FACE_OUTER_BOUND('',#4361,.T.);
#2897=FACE_OUTER_BOUND('',#4362,.T.);
#2898=FACE_OUTER_BOUND('',#4363,.T.);
#2899=FACE_OUTER_BOUND('',#4364,.T.);
#2900=FACE_OUTER_BOUND('',#4365,.T.);
#2901=FACE_OUTER_BOUND('',#4366,.T.);
#2902=FACE_OUTER_BOUND('',#4367,.T.);
#2903=FACE_OUTER_BOUND('',#4368,.T.);
#2904=FACE_OUTER_BOUND('',#4369,.T.);
#2905=FACE_OUTER_BOUND('',#4370,.T.);
#2906=FACE_OUTER_BOUND('',#4371,.T.);
#2907=FACE_OUTER_BOUND('',#4372,.T.);
#2908=FACE_OUTER_BOUND('',#4373,.T.);
#2909=FACE_OUTER_BOUND('',#4374,.T.);
#2910=FACE_OUTER_BOUND('',#4375,.T.);
#2911=FACE_OUTER_BOUND('',#4376,.T.);
#2912=FACE_OUTER_BOUND('',#4377,.T.);
#2913=FACE_OUTER_BOUND('',#4378,.T.);
#2914=FACE_OUTER_BOUND('',#4379,.T.);
#2915=FACE_OUTER_BOUND('',#4380,.T.);
#2916=FACE_OUTER_BOUND('',#4381,.T.);
#2917=FACE_OUTER_BOUND('',#4382,.T.);
#2918=FACE_OUTER_BOUND('',#4383,.T.);
#2919=FACE_OUTER_BOUND('',#4384,.T.);
#2920=FACE_OUTER_BOUND('',#4385,.T.);
#2921=FACE_OUTER_BOUND('',#4386,.T.);
#2922=FACE_OUTER_BOUND('',#4387,.T.);
#2923=FACE_OUTER_BOUND('',#4388,.T.);
#2924=FACE_OUTER_BOUND('',#4389,.T.);
#2925=FACE_OUTER_BOUND('',#4390,.T.);
#2926=FACE_OUTER_BOUND('',#4391,.T.);
#2927=FACE_OUTER_BOUND('',#4392,.T.);
#2928=FACE_OUTER_BOUND('',#4393,.T.);
#2929=FACE_OUTER_BOUND('',#4394,.T.);
#2930=FACE_OUTER_BOUND('',#4395,.T.);
#2931=FACE_OUTER_BOUND('',#4396,.T.);
#2932=FACE_OUTER_BOUND('',#4397,.T.);
#2933=FACE_OUTER_BOUND('',#4398,.T.);
#2934=FACE_OUTER_BOUND('',#4399,.T.);
#2935=FACE_OUTER_BOUND('',#4400,.T.);
#2936=FACE_OUTER_BOUND('',#4401,.T.);
#2937=FACE_OUTER_BOUND('',#4402,.T.);
#2938=FACE_OUTER_BOUND('',#4403,.T.);
#2939=FACE_OUTER_BOUND('',#4404,.T.);
#2940=FACE_OUTER_BOUND('',#4405,.T.);
#2941=FACE_OUTER_BOUND('',#4406,.T.);
#2942=FACE_OUTER_BOUND('',#4407,.T.);
#2943=FACE_OUTER_BOUND('',#4408,.T.);
#2944=FACE_OUTER_BOUND('',#4409,.T.);
#2945=FACE_OUTER_BOUND('',#4410,.T.);
#2946=FACE_OUTER_BOUND('',#4411,.T.);
#2947=FACE_OUTER_BOUND('',#4412,.T.);
#2948=FACE_OUTER_BOUND('',#4413,.T.);
#2949=FACE_OUTER_BOUND('',#4414,.T.);
#2950=FACE_OUTER_BOUND('',#4415,.T.);
#2951=FACE_OUTER_BOUND('',#4416,.T.);
#2952=FACE_OUTER_BOUND('',#4417,.T.);
#2953=FACE_OUTER_BOUND('',#4418,.T.);
#2954=FACE_OUTER_BOUND('',#4419,.T.);
#2955=FACE_OUTER_BOUND('',#4420,.T.);
#2956=FACE_OUTER_BOUND('',#4421,.T.);
#2957=FACE_OUTER_BOUND('',#4422,.T.);
#2958=FACE_OUTER_BOUND('',#4423,.T.);
#2959=FACE_OUTER_BOUND('',#4424,.T.);
#2960=FACE_OUTER_BOUND('',#4425,.T.);
#2961=FACE_OUTER_BOUND('',#4426,.T.);
#2962=FACE_OUTER_BOUND('',#4427,.T.);
#2963=FACE_OUTER_BOUND('',#4428,.T.);
#2964=FACE_OUTER_BOUND('',#4429,.T.);
#2965=FACE_OUTER_BOUND('',#4430,.T.);
#2966=FACE_OUTER_BOUND('',#4431,.T.);
#2967=FACE_OUTER_BOUND('',#4432,.T.);
#2968=FACE_OUTER_BOUND('',#4433,.T.);
#2969=FACE_OUTER_BOUND('',#4434,.T.);
#2970=FACE_OUTER_BOUND('',#4435,.T.);
#2971=FACE_OUTER_BOUND('',#4436,.T.);
#2972=FACE_OUTER_BOUND('',#4437,.T.);
#2973=FACE_OUTER_BOUND('',#4438,.T.);
#2974=FACE_OUTER_BOUND('',#4439,.T.);
#2975=FACE_OUTER_BOUND('',#4440,.T.);
#2976=FACE_OUTER_BOUND('',#4441,.T.);
#2977=FACE_OUTER_BOUND('',#4442,.T.);
#2978=FACE_OUTER_BOUND('',#4443,.T.);
#2979=FACE_OUTER_BOUND('',#4444,.T.);
#2980=FACE_OUTER_BOUND('',#4445,.T.);
#2981=FACE_OUTER_BOUND('',#4446,.T.);
#2982=FACE_OUTER_BOUND('',#4447,.T.);
#2983=FACE_OUTER_BOUND('',#4448,.T.);
#2984=FACE_OUTER_BOUND('',#4449,.T.);
#2985=FACE_OUTER_BOUND('',#4450,.T.);
#2986=FACE_OUTER_BOUND('',#4451,.T.);
#2987=FACE_OUTER_BOUND('',#4452,.T.);
#2988=FACE_OUTER_BOUND('',#4453,.T.);
#2989=FACE_OUTER_BOUND('',#4454,.T.);
#2990=FACE_OUTER_BOUND('',#4456,.T.);
#2991=FACE_OUTER_BOUND('',#4457,.T.);
#2992=FACE_OUTER_BOUND('',#4481,.T.);
#2993=FACE_OUTER_BOUND('',#4482,.T.);
#2994=FACE_OUTER_BOUND('',#4484,.T.);
#2995=FACE_OUTER_BOUND('',#4485,.T.);
#2996=FACE_OUTER_BOUND('',#4486,.T.);
#2997=FACE_OUTER_BOUND('',#4487,.T.);
#2998=FACE_OUTER_BOUND('',#4488,.T.);
#2999=FACE_OUTER_BOUND('',#4489,.T.);
#3000=FACE_OUTER_BOUND('',#4490,.T.);
#3001=FACE_OUTER_BOUND('',#4491,.T.);
#3002=FACE_OUTER_BOUND('',#4492,.T.);
#3003=FACE_OUTER_BOUND('',#4493,.T.);
#3004=FACE_OUTER_BOUND('',#4494,.T.);
#3005=FACE_OUTER_BOUND('',#4495,.T.);
#3006=FACE_OUTER_BOUND('',#4496,.T.);
#3007=FACE_OUTER_BOUND('',#4497,.T.);
#3008=FACE_OUTER_BOUND('',#4498,.T.);
#3009=FACE_OUTER_BOUND('',#4499,.T.);
#3010=FACE_OUTER_BOUND('',#4500,.T.);
#3011=FACE_OUTER_BOUND('',#4501,.T.);
#3012=FACE_OUTER_BOUND('',#4502,.T.);
#3013=FACE_OUTER_BOUND('',#4503,.T.);
#3014=FACE_OUTER_BOUND('',#4504,.T.);
#3015=FACE_OUTER_BOUND('',#4505,.T.);
#3016=FACE_OUTER_BOUND('',#4506,.T.);
#3017=FACE_OUTER_BOUND('',#4507,.T.);
#3018=FACE_OUTER_BOUND('',#4508,.T.);
#3019=FACE_OUTER_BOUND('',#4509,.T.);
#3020=FACE_OUTER_BOUND('',#4510,.T.);
#3021=FACE_OUTER_BOUND('',#4511,.T.);
#3022=FACE_OUTER_BOUND('',#4512,.T.);
#3023=FACE_OUTER_BOUND('',#4513,.T.);
#3024=FACE_OUTER_BOUND('',#4514,.T.);
#3025=FACE_OUTER_BOUND('',#4515,.T.);
#3026=FACE_OUTER_BOUND('',#4516,.T.);
#3027=FACE_OUTER_BOUND('',#4517,.T.);
#3028=FACE_OUTER_BOUND('',#4518,.T.);
#3029=FACE_OUTER_BOUND('',#4519,.T.);
#3030=FACE_OUTER_BOUND('',#4520,.T.);
#3031=FACE_OUTER_BOUND('',#4521,.T.);
#3032=FACE_OUTER_BOUND('',#4522,.T.);
#3033=FACE_OUTER_BOUND('',#4523,.T.);
#3034=FACE_OUTER_BOUND('',#4524,.T.);
#3035=FACE_OUTER_BOUND('',#4525,.T.);
#3036=FACE_OUTER_BOUND('',#4526,.T.);
#3037=FACE_OUTER_BOUND('',#4527,.T.);
#3038=FACE_OUTER_BOUND('',#4528,.T.);
#3039=FACE_OUTER_BOUND('',#4529,.T.);
#3040=FACE_OUTER_BOUND('',#4530,.T.);
#3041=FACE_OUTER_BOUND('',#4531,.T.);
#3042=FACE_OUTER_BOUND('',#4532,.T.);
#3043=FACE_OUTER_BOUND('',#4533,.T.);
#3044=FACE_OUTER_BOUND('',#4534,.T.);
#3045=FACE_OUTER_BOUND('',#4535,.T.);
#3046=FACE_OUTER_BOUND('',#4536,.T.);
#3047=FACE_OUTER_BOUND('',#4537,.T.);
#3048=FACE_OUTER_BOUND('',#4538,.T.);
#3049=FACE_OUTER_BOUND('',#4539,.T.);
#3050=FACE_OUTER_BOUND('',#4540,.T.);
#3051=FACE_OUTER_BOUND('',#4541,.T.);
#3052=FACE_OUTER_BOUND('',#4542,.T.);
#3053=FACE_OUTER_BOUND('',#4543,.T.);
#3054=FACE_OUTER_BOUND('',#4544,.T.);
#3055=FACE_OUTER_BOUND('',#4545,.T.);
#3056=FACE_OUTER_BOUND('',#4546,.T.);
#3057=FACE_OUTER_BOUND('',#4547,.T.);
#3058=FACE_OUTER_BOUND('',#4548,.T.);
#3059=FACE_OUTER_BOUND('',#4549,.T.);
#3060=FACE_OUTER_BOUND('',#4550,.T.);
#3061=FACE_OUTER_BOUND('',#4551,.T.);
#3062=FACE_OUTER_BOUND('',#4552,.T.);
#3063=FACE_OUTER_BOUND('',#4553,.T.);
#3064=FACE_OUTER_BOUND('',#4554,.T.);
#3065=FACE_OUTER_BOUND('',#4555,.T.);
#3066=FACE_OUTER_BOUND('',#4556,.T.);
#3067=FACE_OUTER_BOUND('',#4557,.T.);
#3068=FACE_OUTER_BOUND('',#4558,.T.);
#3069=FACE_OUTER_BOUND('',#4559,.T.);
#3070=FACE_OUTER_BOUND('',#4560,.T.);
#3071=FACE_OUTER_BOUND('',#4561,.T.);
#3072=FACE_OUTER_BOUND('',#4562,.T.);
#3073=FACE_OUTER_BOUND('',#4563,.T.);
#3074=FACE_OUTER_BOUND('',#4564,.T.);
#3075=FACE_OUTER_BOUND('',#4565,.T.);
#3076=FACE_OUTER_BOUND('',#4566,.T.);
#3077=FACE_OUTER_BOUND('',#4567,.T.);
#3078=FACE_OUTER_BOUND('',#4568,.T.);
#3079=FACE_OUTER_BOUND('',#4569,.T.);
#3080=FACE_OUTER_BOUND('',#4570,.T.);
#3081=FACE_OUTER_BOUND('',#4571,.T.);
#3082=FACE_OUTER_BOUND('',#4572,.T.);
#3083=FACE_OUTER_BOUND('',#4573,.T.);
#3084=FACE_OUTER_BOUND('',#4574,.T.);
#3085=FACE_OUTER_BOUND('',#4575,.T.);
#3086=FACE_OUTER_BOUND('',#4576,.T.);
#3087=FACE_OUTER_BOUND('',#4577,.T.);
#3088=FACE_OUTER_BOUND('',#4578,.T.);
#3089=FACE_OUTER_BOUND('',#4579,.T.);
#3090=FACE_OUTER_BOUND('',#4580,.T.);
#3091=FACE_OUTER_BOUND('',#4581,.T.);
#3092=FACE_OUTER_BOUND('',#4582,.T.);
#3093=FACE_OUTER_BOUND('',#4583,.T.);
#3094=FACE_OUTER_BOUND('',#4584,.T.);
#3095=FACE_OUTER_BOUND('',#4585,.T.);
#3096=FACE_OUTER_BOUND('',#4586,.T.);
#3097=FACE_OUTER_BOUND('',#4587,.T.);
#3098=FACE_OUTER_BOUND('',#4588,.T.);
#3099=FACE_OUTER_BOUND('',#4589,.T.);
#3100=FACE_OUTER_BOUND('',#4590,.T.);
#3101=FACE_OUTER_BOUND('',#4591,.T.);
#3102=FACE_OUTER_BOUND('',#4592,.T.);
#3103=FACE_OUTER_BOUND('',#4593,.T.);
#3104=FACE_OUTER_BOUND('',#4594,.T.);
#3105=FACE_OUTER_BOUND('',#4595,.T.);
#3106=FACE_OUTER_BOUND('',#4596,.T.);
#3107=FACE_OUTER_BOUND('',#4597,.T.);
#3108=FACE_OUTER_BOUND('',#4598,.T.);
#3109=FACE_OUTER_BOUND('',#4599,.T.);
#3110=FACE_OUTER_BOUND('',#4600,.T.);
#3111=FACE_OUTER_BOUND('',#4601,.T.);
#3112=FACE_OUTER_BOUND('',#4602,.T.);
#3113=FACE_OUTER_BOUND('',#4603,.T.);
#3114=FACE_OUTER_BOUND('',#4604,.T.);
#3115=FACE_OUTER_BOUND('',#4605,.T.);
#3116=FACE_OUTER_BOUND('',#4606,.T.);
#3117=FACE_OUTER_BOUND('',#4607,.T.);
#3118=FACE_OUTER_BOUND('',#4608,.T.);
#3119=FACE_OUTER_BOUND('',#4609,.T.);
#3120=FACE_OUTER_BOUND('',#4610,.T.);
#3121=FACE_OUTER_BOUND('',#4611,.T.);
#3122=FACE_OUTER_BOUND('',#4612,.T.);
#3123=FACE_OUTER_BOUND('',#4613,.T.);
#3124=FACE_OUTER_BOUND('',#4614,.T.);
#3125=FACE_OUTER_BOUND('',#4615,.T.);
#3126=FACE_OUTER_BOUND('',#4616,.T.);
#3127=FACE_OUTER_BOUND('',#4617,.T.);
#3128=FACE_OUTER_BOUND('',#4618,.T.);
#3129=FACE_OUTER_BOUND('',#4619,.T.);
#3130=FACE_OUTER_BOUND('',#4620,.T.);
#3131=FACE_OUTER_BOUND('',#4621,.T.);
#3132=FACE_OUTER_BOUND('',#4622,.T.);
#3133=FACE_OUTER_BOUND('',#4623,.T.);
#3134=FACE_OUTER_BOUND('',#4624,.T.);
#3135=FACE_OUTER_BOUND('',#4625,.T.);
#3136=FACE_OUTER_BOUND('',#4626,.T.);
#3137=FACE_OUTER_BOUND('',#4627,.T.);
#3138=FACE_OUTER_BOUND('',#4628,.T.);
#3139=FACE_OUTER_BOUND('',#4629,.T.);
#3140=FACE_OUTER_BOUND('',#4630,.T.);
#3141=FACE_OUTER_BOUND('',#4631,.T.);
#3142=FACE_OUTER_BOUND('',#4632,.T.);
#3143=FACE_OUTER_BOUND('',#4633,.T.);
#3144=FACE_OUTER_BOUND('',#4634,.T.);
#3145=FACE_OUTER_BOUND('',#4635,.T.);
#3146=FACE_OUTER_BOUND('',#4637,.T.);
#3147=FACE_OUTER_BOUND('',#4638,.T.);
#3148=FACE_OUTER_BOUND('',#4639,.T.);
#3149=FACE_OUTER_BOUND('',#4640,.T.);
#3150=FACE_OUTER_BOUND('',#4641,.T.);
#3151=FACE_OUTER_BOUND('',#4643,.T.);
#3152=FACE_OUTER_BOUND('',#4645,.T.);
#3153=FACE_OUTER_BOUND('',#4646,.T.);
#3154=FACE_OUTER_BOUND('',#4647,.T.);
#3155=FACE_OUTER_BOUND('',#4648,.T.);
#3156=FACE_OUTER_BOUND('',#4649,.T.);
#3157=FACE_OUTER_BOUND('',#4650,.T.);
#3158=FACE_OUTER_BOUND('',#4651,.T.);
#3159=FACE_OUTER_BOUND('',#4652,.T.);
#3160=FACE_OUTER_BOUND('',#4653,.T.);
#3161=FACE_OUTER_BOUND('',#4654,.T.);
#3162=FACE_OUTER_BOUND('',#4655,.T.);
#3163=FACE_OUTER_BOUND('',#4656,.T.);
#3164=FACE_OUTER_BOUND('',#4657,.T.);
#3165=FACE_OUTER_BOUND('',#4658,.T.);
#3166=FACE_OUTER_BOUND('',#4659,.T.);
#3167=FACE_OUTER_BOUND('',#4660,.T.);
#3168=FACE_OUTER_BOUND('',#4661,.T.);
#3169=FACE_OUTER_BOUND('',#4662,.T.);
#3170=FACE_OUTER_BOUND('',#4663,.T.);
#3171=FACE_OUTER_BOUND('',#4664,.T.);
#3172=FACE_OUTER_BOUND('',#4665,.T.);
#3173=FACE_OUTER_BOUND('',#4666,.T.);
#3174=FACE_OUTER_BOUND('',#4667,.T.);
#3175=FACE_OUTER_BOUND('',#4668,.T.);
#3176=FACE_OUTER_BOUND('',#4669,.T.);
#3177=FACE_OUTER_BOUND('',#4670,.T.);
#3178=FACE_OUTER_BOUND('',#4671,.T.);
#3179=FACE_OUTER_BOUND('',#4672,.T.);
#3180=FACE_OUTER_BOUND('',#4673,.T.);
#3181=FACE_OUTER_BOUND('',#4674,.T.);
#3182=FACE_OUTER_BOUND('',#4675,.T.);
#3183=FACE_OUTER_BOUND('',#4676,.T.);
#3184=FACE_OUTER_BOUND('',#4677,.T.);
#3185=FACE_OUTER_BOUND('',#4678,.T.);
#3186=FACE_OUTER_BOUND('',#4679,.T.);
#3187=FACE_OUTER_BOUND('',#4680,.T.);
#3188=FACE_OUTER_BOUND('',#4681,.T.);
#3189=FACE_OUTER_BOUND('',#4682,.T.);
#3190=FACE_OUTER_BOUND('',#4683,.T.);
#3191=FACE_OUTER_BOUND('',#4684,.T.);
#3192=FACE_OUTER_BOUND('',#4685,.T.);
#3193=FACE_OUTER_BOUND('',#4686,.T.);
#3194=FACE_OUTER_BOUND('',#4687,.T.);
#3195=FACE_OUTER_BOUND('',#4688,.T.);
#3196=FACE_OUTER_BOUND('',#4689,.T.);
#3197=FACE_OUTER_BOUND('',#4690,.T.);
#3198=FACE_OUTER_BOUND('',#4691,.T.);
#3199=FACE_OUTER_BOUND('',#4692,.T.);
#3200=FACE_OUTER_BOUND('',#4693,.T.);
#3201=FACE_OUTER_BOUND('',#4694,.T.);
#3202=FACE_OUTER_BOUND('',#4695,.T.);
#3203=FACE_OUTER_BOUND('',#4696,.T.);
#3204=FACE_OUTER_BOUND('',#4697,.T.);
#3205=FACE_OUTER_BOUND('',#4698,.T.);
#3206=FACE_OUTER_BOUND('',#4699,.T.);
#3207=FACE_OUTER_BOUND('',#4700,.T.);
#3208=FACE_OUTER_BOUND('',#4701,.T.);
#3209=FACE_OUTER_BOUND('',#4702,.T.);
#3210=FACE_OUTER_BOUND('',#4703,.T.);
#3211=FACE_OUTER_BOUND('',#4704,.T.);
#3212=FACE_OUTER_BOUND('',#4705,.T.);
#3213=FACE_OUTER_BOUND('',#4706,.T.);
#3214=FACE_OUTER_BOUND('',#4707,.T.);
#3215=FACE_OUTER_BOUND('',#4708,.T.);
#3216=FACE_OUTER_BOUND('',#4709,.T.);
#3217=FACE_OUTER_BOUND('',#4710,.T.);
#3218=FACE_OUTER_BOUND('',#4711,.T.);
#3219=FACE_OUTER_BOUND('',#4712,.T.);
#3220=FACE_OUTER_BOUND('',#4713,.T.);
#3221=FACE_OUTER_BOUND('',#4714,.T.);
#3222=FACE_OUTER_BOUND('',#4715,.T.);
#3223=FACE_OUTER_BOUND('',#4716,.T.);
#3224=FACE_OUTER_BOUND('',#4717,.T.);
#3225=FACE_OUTER_BOUND('',#4718,.T.);
#3226=FACE_OUTER_BOUND('',#4719,.T.);
#3227=FACE_OUTER_BOUND('',#4720,.T.);
#3228=FACE_OUTER_BOUND('',#4721,.T.);
#3229=FACE_OUTER_BOUND('',#4722,.T.);
#3230=FACE_OUTER_BOUND('',#4723,.T.);
#3231=FACE_OUTER_BOUND('',#4724,.T.);
#3232=FACE_OUTER_BOUND('',#4725,.T.);
#3233=FACE_OUTER_BOUND('',#4726,.T.);
#3234=FACE_OUTER_BOUND('',#4727,.T.);
#3235=FACE_OUTER_BOUND('',#4728,.T.);
#3236=FACE_OUTER_BOUND('',#4729,.T.);
#3237=FACE_OUTER_BOUND('',#4730,.T.);
#3238=FACE_OUTER_BOUND('',#4731,.T.);
#3239=FACE_OUTER_BOUND('',#4732,.T.);
#3240=FACE_OUTER_BOUND('',#4733,.T.);
#3241=FACE_OUTER_BOUND('',#4734,.T.);
#3242=FACE_OUTER_BOUND('',#4735,.T.);
#3243=FACE_OUTER_BOUND('',#4736,.T.);
#3244=FACE_OUTER_BOUND('',#4737,.T.);
#3245=FACE_OUTER_BOUND('',#4738,.T.);
#3246=FACE_OUTER_BOUND('',#4739,.T.);
#3247=FACE_OUTER_BOUND('',#4740,.T.);
#3248=FACE_OUTER_BOUND('',#4741,.T.);
#3249=FACE_OUTER_BOUND('',#4742,.T.);
#3250=FACE_OUTER_BOUND('',#4743,.T.);
#3251=FACE_OUTER_BOUND('',#4744,.T.);
#3252=FACE_OUTER_BOUND('',#4745,.T.);
#3253=FACE_OUTER_BOUND('',#4746,.T.);
#3254=FACE_OUTER_BOUND('',#4747,.T.);
#3255=FACE_OUTER_BOUND('',#4748,.T.);
#3256=FACE_OUTER_BOUND('',#4749,.T.);
#3257=FACE_OUTER_BOUND('',#4750,.T.);
#3258=FACE_OUTER_BOUND('',#4751,.T.);
#3259=FACE_OUTER_BOUND('',#4752,.T.);
#3260=FACE_OUTER_BOUND('',#4753,.T.);
#3261=FACE_OUTER_BOUND('',#4754,.T.);
#3262=FACE_OUTER_BOUND('',#4755,.T.);
#3263=FACE_OUTER_BOUND('',#4756,.T.);
#3264=FACE_OUTER_BOUND('',#4757,.T.);
#3265=FACE_OUTER_BOUND('',#4758,.T.);
#3266=FACE_OUTER_BOUND('',#4759,.T.);
#3267=FACE_OUTER_BOUND('',#4760,.T.);
#3268=FACE_OUTER_BOUND('',#4761,.T.);
#3269=FACE_OUTER_BOUND('',#4762,.T.);
#3270=FACE_OUTER_BOUND('',#4763,.T.);
#3271=FACE_OUTER_BOUND('',#4764,.T.);
#3272=FACE_OUTER_BOUND('',#4765,.T.);
#3273=FACE_OUTER_BOUND('',#4766,.T.);
#3274=FACE_OUTER_BOUND('',#4767,.T.);
#3275=FACE_OUTER_BOUND('',#4768,.T.);
#3276=FACE_OUTER_BOUND('',#4769,.T.);
#3277=FACE_OUTER_BOUND('',#4770,.T.);
#3278=FACE_OUTER_BOUND('',#4771,.T.);
#3279=FACE_OUTER_BOUND('',#4772,.T.);
#3280=FACE_OUTER_BOUND('',#4773,.T.);
#3281=FACE_OUTER_BOUND('',#4774,.T.);
#3282=FACE_OUTER_BOUND('',#4775,.T.);
#3283=FACE_OUTER_BOUND('',#4776,.T.);
#3284=FACE_OUTER_BOUND('',#4777,.T.);
#3285=FACE_OUTER_BOUND('',#4778,.T.);
#3286=FACE_OUTER_BOUND('',#4779,.T.);
#3287=FACE_OUTER_BOUND('',#4780,.T.);
#3288=FACE_OUTER_BOUND('',#4781,.T.);
#3289=FACE_OUTER_BOUND('',#4782,.T.);
#3290=FACE_OUTER_BOUND('',#4783,.T.);
#3291=FACE_OUTER_BOUND('',#4784,.T.);
#3292=FACE_OUTER_BOUND('',#4785,.T.);
#3293=FACE_OUTER_BOUND('',#4786,.T.);
#3294=FACE_OUTER_BOUND('',#4787,.T.);
#3295=FACE_OUTER_BOUND('',#4788,.T.);
#3296=FACE_OUTER_BOUND('',#4789,.T.);
#3297=FACE_OUTER_BOUND('',#4790,.T.);
#3298=FACE_OUTER_BOUND('',#4791,.T.);
#3299=FACE_OUTER_BOUND('',#4792,.T.);
#3300=FACE_OUTER_BOUND('',#4793,.T.);
#3301=FACE_OUTER_BOUND('',#4794,.T.);
#3302=FACE_OUTER_BOUND('',#4795,.T.);
#3303=FACE_OUTER_BOUND('',#4796,.T.);
#3304=FACE_OUTER_BOUND('',#4797,.T.);
#3305=FACE_OUTER_BOUND('',#4798,.T.);
#3306=FACE_OUTER_BOUND('',#4799,.T.);
#3307=FACE_OUTER_BOUND('',#4800,.T.);
#3308=FACE_OUTER_BOUND('',#4801,.T.);
#3309=FACE_OUTER_BOUND('',#4802,.T.);
#3310=FACE_OUTER_BOUND('',#4803,.T.);
#3311=FACE_OUTER_BOUND('',#4804,.T.);
#3312=FACE_OUTER_BOUND('',#4805,.T.);
#3313=FACE_OUTER_BOUND('',#4806,.T.);
#3314=FACE_OUTER_BOUND('',#4807,.T.);
#3315=FACE_OUTER_BOUND('',#4808,.T.);
#3316=FACE_OUTER_BOUND('',#4809,.T.);
#3317=FACE_OUTER_BOUND('',#4810,.T.);
#3318=FACE_OUTER_BOUND('',#4811,.T.);
#3319=FACE_OUTER_BOUND('',#4812,.T.);
#3320=FACE_OUTER_BOUND('',#4813,.T.);
#3321=FACE_OUTER_BOUND('',#4814,.T.);
#3322=FACE_OUTER_BOUND('',#4815,.T.);
#3323=FACE_OUTER_BOUND('',#4816,.T.);
#3324=FACE_OUTER_BOUND('',#4817,.T.);
#3325=FACE_OUTER_BOUND('',#4818,.T.);
#3326=FACE_OUTER_BOUND('',#4819,.T.);
#3327=FACE_OUTER_BOUND('',#4820,.T.);
#3328=FACE_OUTER_BOUND('',#4821,.T.);
#3329=FACE_OUTER_BOUND('',#4822,.T.);
#3330=FACE_OUTER_BOUND('',#4823,.T.);
#3331=FACE_OUTER_BOUND('',#4824,.T.);
#3332=FACE_OUTER_BOUND('',#4825,.T.);
#3333=FACE_OUTER_BOUND('',#4826,.T.);
#3334=FACE_OUTER_BOUND('',#4827,.T.);
#3335=FACE_OUTER_BOUND('',#4828,.T.);
#3336=FACE_OUTER_BOUND('',#4829,.T.);
#3337=FACE_OUTER_BOUND('',#4830,.T.);
#3338=FACE_OUTER_BOUND('',#4831,.T.);
#3339=FACE_OUTER_BOUND('',#4832,.T.);
#3340=FACE_OUTER_BOUND('',#4833,.T.);
#3341=FACE_OUTER_BOUND('',#4834,.T.);
#3342=FACE_OUTER_BOUND('',#4835,.T.);
#3343=FACE_OUTER_BOUND('',#4836,.T.);
#3344=FACE_OUTER_BOUND('',#4837,.T.);
#3345=FACE_OUTER_BOUND('',#4838,.T.);
#3346=FACE_OUTER_BOUND('',#4839,.T.);
#3347=FACE_OUTER_BOUND('',#4840,.T.);
#3348=FACE_OUTER_BOUND('',#4841,.T.);
#3349=FACE_OUTER_BOUND('',#4842,.T.);
#3350=FACE_OUTER_BOUND('',#4843,.T.);
#3351=FACE_OUTER_BOUND('',#4844,.T.);
#3352=FACE_OUTER_BOUND('',#4845,.T.);
#3353=FACE_OUTER_BOUND('',#4846,.T.);
#3354=FACE_OUTER_BOUND('',#4847,.T.);
#3355=FACE_OUTER_BOUND('',#4848,.T.);
#3356=FACE_OUTER_BOUND('',#4849,.T.);
#3357=FACE_OUTER_BOUND('',#4850,.T.);
#3358=FACE_OUTER_BOUND('',#4851,.T.);
#3359=FACE_OUTER_BOUND('',#4852,.T.);
#3360=FACE_OUTER_BOUND('',#4853,.T.);
#3361=FACE_OUTER_BOUND('',#4854,.T.);
#3362=FACE_OUTER_BOUND('',#4855,.T.);
#3363=FACE_OUTER_BOUND('',#4856,.T.);
#3364=FACE_OUTER_BOUND('',#4857,.T.);
#3365=FACE_OUTER_BOUND('',#4858,.T.);
#3366=FACE_OUTER_BOUND('',#4859,.T.);
#3367=FACE_OUTER_BOUND('',#4860,.T.);
#3368=FACE_OUTER_BOUND('',#4861,.T.);
#3369=FACE_OUTER_BOUND('',#4862,.T.);
#3370=FACE_OUTER_BOUND('',#4863,.T.);
#3371=FACE_OUTER_BOUND('',#4864,.T.);
#3372=FACE_OUTER_BOUND('',#4865,.T.);
#3373=FACE_OUTER_BOUND('',#4866,.T.);
#3374=FACE_OUTER_BOUND('',#4867,.T.);
#3375=FACE_OUTER_BOUND('',#4868,.T.);
#3376=FACE_OUTER_BOUND('',#4869,.T.);
#3377=FACE_OUTER_BOUND('',#4870,.T.);
#3378=FACE_OUTER_BOUND('',#4871,.T.);
#3379=FACE_OUTER_BOUND('',#4872,.T.);
#3380=FACE_OUTER_BOUND('',#4873,.T.);
#3381=FACE_OUTER_BOUND('',#4874,.T.);
#3382=FACE_OUTER_BOUND('',#4875,.T.);
#3383=FACE_OUTER_BOUND('',#4876,.T.);
#3384=FACE_OUTER_BOUND('',#4877,.T.);
#3385=FACE_OUTER_BOUND('',#4878,.T.);
#3386=FACE_OUTER_BOUND('',#4879,.T.);
#3387=FACE_OUTER_BOUND('',#4880,.T.);
#3388=FACE_OUTER_BOUND('',#4881,.T.);
#3389=FACE_OUTER_BOUND('',#4882,.T.);
#3390=FACE_OUTER_BOUND('',#4883,.T.);
#3391=FACE_OUTER_BOUND('',#4884,.T.);
#3392=FACE_OUTER_BOUND('',#4886,.T.);
#3393=FACE_OUTER_BOUND('',#4887,.T.);
#3394=FACE_OUTER_BOUND('',#4888,.T.);
#3395=FACE_OUTER_BOUND('',#4889,.T.);
#3396=FACE_OUTER_BOUND('',#4890,.T.);
#3397=FACE_OUTER_BOUND('',#4892,.T.);
#3398=FACE_OUTER_BOUND('',#4894,.T.);
#3399=FACE_OUTER_BOUND('',#4895,.T.);
#3400=FACE_OUTER_BOUND('',#4896,.T.);
#3401=FACE_OUTER_BOUND('',#4897,.T.);
#3402=FACE_OUTER_BOUND('',#4898,.T.);
#3403=FACE_OUTER_BOUND('',#4899,.T.);
#3404=FACE_OUTER_BOUND('',#4900,.T.);
#3405=FACE_OUTER_BOUND('',#4901,.T.);
#3406=FACE_OUTER_BOUND('',#4902,.T.);
#3407=FACE_OUTER_BOUND('',#4903,.T.);
#3408=FACE_OUTER_BOUND('',#4904,.T.);
#3409=FACE_OUTER_BOUND('',#4905,.T.);
#3410=FACE_OUTER_BOUND('',#4906,.T.);
#3411=FACE_OUTER_BOUND('',#4907,.T.);
#3412=FACE_OUTER_BOUND('',#4908,.T.);
#3413=FACE_OUTER_BOUND('',#4909,.T.);
#3414=FACE_OUTER_BOUND('',#4910,.T.);
#3415=FACE_OUTER_BOUND('',#4911,.T.);
#3416=FACE_OUTER_BOUND('',#4912,.T.);
#3417=FACE_OUTER_BOUND('',#4913,.T.);
#3418=FACE_OUTER_BOUND('',#4914,.T.);
#3419=FACE_OUTER_BOUND('',#4915,.T.);
#3420=FACE_OUTER_BOUND('',#4916,.T.);
#3421=FACE_OUTER_BOUND('',#4917,.T.);
#3422=FACE_OUTER_BOUND('',#4918,.T.);
#3423=FACE_OUTER_BOUND('',#4919,.T.);
#3424=FACE_OUTER_BOUND('',#4920,.T.);
#3425=FACE_OUTER_BOUND('',#4921,.T.);
#3426=FACE_OUTER_BOUND('',#4922,.T.);
#3427=FACE_OUTER_BOUND('',#4923,.T.);
#3428=FACE_OUTER_BOUND('',#4924,.T.);
#3429=FACE_OUTER_BOUND('',#4925,.T.);
#3430=FACE_OUTER_BOUND('',#4926,.T.);
#3431=FACE_OUTER_BOUND('',#4927,.T.);
#3432=FACE_OUTER_BOUND('',#4928,.T.);
#3433=FACE_OUTER_BOUND('',#4929,.T.);
#3434=FACE_OUTER_BOUND('',#4930,.T.);
#3435=FACE_OUTER_BOUND('',#4931,.T.);
#3436=FACE_OUTER_BOUND('',#4932,.T.);
#3437=FACE_OUTER_BOUND('',#4933,.T.);
#3438=FACE_OUTER_BOUND('',#4934,.T.);
#3439=FACE_OUTER_BOUND('',#4935,.T.);
#3440=FACE_OUTER_BOUND('',#4936,.T.);
#3441=FACE_OUTER_BOUND('',#4937,.T.);
#3442=FACE_OUTER_BOUND('',#4938,.T.);
#3443=FACE_OUTER_BOUND('',#4939,.T.);
#3444=FACE_OUTER_BOUND('',#4940,.T.);
#3445=FACE_OUTER_BOUND('',#4941,.T.);
#3446=FACE_OUTER_BOUND('',#4942,.T.);
#3447=FACE_OUTER_BOUND('',#4943,.T.);
#3448=FACE_OUTER_BOUND('',#4944,.T.);
#3449=FACE_OUTER_BOUND('',#4945,.T.);
#3450=FACE_OUTER_BOUND('',#4946,.T.);
#3451=FACE_OUTER_BOUND('',#4947,.T.);
#3452=FACE_OUTER_BOUND('',#4948,.T.);
#3453=FACE_OUTER_BOUND('',#4949,.T.);
#3454=FACE_OUTER_BOUND('',#4950,.T.);
#3455=FACE_OUTER_BOUND('',#4951,.T.);
#3456=FACE_OUTER_BOUND('',#4952,.T.);
#3457=FACE_OUTER_BOUND('',#4953,.T.);
#3458=FACE_OUTER_BOUND('',#4954,.T.);
#3459=FACE_OUTER_BOUND('',#4955,.T.);
#3460=FACE_OUTER_BOUND('',#4956,.T.);
#3461=FACE_OUTER_BOUND('',#4957,.T.);
#3462=FACE_OUTER_BOUND('',#4958,.T.);
#3463=FACE_OUTER_BOUND('',#4959,.T.);
#3464=FACE_OUTER_BOUND('',#4960,.T.);
#3465=FACE_OUTER_BOUND('',#4961,.T.);
#3466=FACE_OUTER_BOUND('',#4962,.T.);
#3467=FACE_OUTER_BOUND('',#4963,.T.);
#3468=FACE_OUTER_BOUND('',#4964,.T.);
#3469=FACE_OUTER_BOUND('',#4965,.T.);
#3470=FACE_OUTER_BOUND('',#4966,.T.);
#3471=FACE_OUTER_BOUND('',#4967,.T.);
#3472=FACE_OUTER_BOUND('',#4968,.T.);
#3473=FACE_OUTER_BOUND('',#4969,.T.);
#3474=FACE_OUTER_BOUND('',#4970,.T.);
#3475=FACE_OUTER_BOUND('',#4971,.T.);
#3476=FACE_OUTER_BOUND('',#4972,.T.);
#3477=FACE_OUTER_BOUND('',#4973,.T.);
#3478=FACE_OUTER_BOUND('',#4974,.T.);
#3479=FACE_OUTER_BOUND('',#4975,.T.);
#3480=FACE_OUTER_BOUND('',#4976,.T.);
#3481=FACE_OUTER_BOUND('',#4977,.T.);
#3482=FACE_OUTER_BOUND('',#4978,.T.);
#3483=FACE_OUTER_BOUND('',#4979,.T.);
#3484=FACE_OUTER_BOUND('',#4980,.T.);
#3485=FACE_OUTER_BOUND('',#4981,.T.);
#3486=FACE_OUTER_BOUND('',#4982,.T.);
#3487=FACE_OUTER_BOUND('',#4983,.T.);
#3488=FACE_OUTER_BOUND('',#4984,.T.);
#3489=FACE_OUTER_BOUND('',#4985,.T.);
#3490=FACE_OUTER_BOUND('',#4986,.T.);
#3491=FACE_OUTER_BOUND('',#4987,.T.);
#3492=FACE_OUTER_BOUND('',#4988,.T.);
#3493=FACE_OUTER_BOUND('',#4989,.T.);
#3494=FACE_OUTER_BOUND('',#4990,.T.);
#3495=FACE_OUTER_BOUND('',#4991,.T.);
#3496=FACE_OUTER_BOUND('',#4992,.T.);
#3497=FACE_OUTER_BOUND('',#4993,.T.);
#3498=FACE_OUTER_BOUND('',#4994,.T.);
#3499=FACE_OUTER_BOUND('',#4995,.T.);
#3500=FACE_OUTER_BOUND('',#4996,.T.);
#3501=FACE_OUTER_BOUND('',#4997,.T.);
#3502=FACE_OUTER_BOUND('',#4998,.T.);
#3503=FACE_OUTER_BOUND('',#4999,.T.);
#3504=FACE_OUTER_BOUND('',#5000,.T.);
#3505=FACE_OUTER_BOUND('',#5001,.T.);
#3506=FACE_OUTER_BOUND('',#5002,.T.);
#3507=FACE_OUTER_BOUND('',#5003,.T.);
#3508=FACE_OUTER_BOUND('',#5004,.T.);
#3509=FACE_OUTER_BOUND('',#5005,.T.);
#3510=FACE_OUTER_BOUND('',#5006,.T.);
#3511=FACE_OUTER_BOUND('',#5007,.T.);
#3512=FACE_OUTER_BOUND('',#5008,.T.);
#3513=FACE_OUTER_BOUND('',#5009,.T.);
#3514=FACE_OUTER_BOUND('',#5010,.T.);
#3515=FACE_OUTER_BOUND('',#5011,.T.);
#3516=FACE_OUTER_BOUND('',#5012,.T.);
#3517=FACE_OUTER_BOUND('',#5013,.T.);
#3518=FACE_OUTER_BOUND('',#5014,.T.);
#3519=FACE_OUTER_BOUND('',#5015,.T.);
#3520=FACE_OUTER_BOUND('',#5016,.T.);
#3521=FACE_OUTER_BOUND('',#5017,.T.);
#3522=FACE_OUTER_BOUND('',#5018,.T.);
#3523=FACE_OUTER_BOUND('',#5019,.T.);
#3524=FACE_OUTER_BOUND('',#5020,.T.);
#3525=FACE_OUTER_BOUND('',#5021,.T.);
#3526=FACE_OUTER_BOUND('',#5022,.T.);
#3527=FACE_OUTER_BOUND('',#5023,.T.);
#3528=FACE_OUTER_BOUND('',#5024,.T.);
#3529=FACE_OUTER_BOUND('',#5025,.T.);
#3530=FACE_OUTER_BOUND('',#5026,.T.);
#3531=FACE_OUTER_BOUND('',#5027,.T.);
#3532=FACE_OUTER_BOUND('',#5028,.T.);
#3533=FACE_OUTER_BOUND('',#5029,.T.);
#3534=FACE_OUTER_BOUND('',#5030,.T.);
#3535=FACE_OUTER_BOUND('',#5031,.T.);
#3536=FACE_OUTER_BOUND('',#5032,.T.);
#3537=FACE_OUTER_BOUND('',#5033,.T.);
#3538=FACE_OUTER_BOUND('',#5034,.T.);
#3539=FACE_OUTER_BOUND('',#5035,.T.);
#3540=FACE_OUTER_BOUND('',#5036,.T.);
#3541=FACE_OUTER_BOUND('',#5037,.T.);
#3542=FACE_OUTER_BOUND('',#5038,.T.);
#3543=FACE_OUTER_BOUND('',#5039,.T.);
#3544=FACE_OUTER_BOUND('',#5040,.T.);
#3545=FACE_OUTER_BOUND('',#5041,.T.);
#3546=FACE_OUTER_BOUND('',#5042,.T.);
#3547=FACE_OUTER_BOUND('',#5043,.T.);
#3548=FACE_OUTER_BOUND('',#5044,.T.);
#3549=FACE_OUTER_BOUND('',#5045,.T.);
#3550=FACE_OUTER_BOUND('',#5046,.T.);
#3551=FACE_OUTER_BOUND('',#5047,.T.);
#3552=FACE_OUTER_BOUND('',#5048,.T.);
#3553=FACE_OUTER_BOUND('',#5049,.T.);
#3554=FACE_OUTER_BOUND('',#5050,.T.);
#3555=FACE_OUTER_BOUND('',#5051,.T.);
#3556=FACE_OUTER_BOUND('',#5052,.T.);
#3557=FACE_OUTER_BOUND('',#5053,.T.);
#3558=FACE_OUTER_BOUND('',#5055,.T.);
#3559=FACE_OUTER_BOUND('',#5056,.T.);
#3560=FACE_OUTER_BOUND('',#5057,.T.);
#3561=FACE_OUTER_BOUND('',#5058,.T.);
#3562=FACE_OUTER_BOUND('',#5059,.T.);
#3563=FACE_OUTER_BOUND('',#5061,.T.);
#3564=EDGE_LOOP('',(#15067,#15068,#15069,#15070));
#3565=EDGE_LOOP('',(#15071,#15072,#15073,#15074));
#3566=EDGE_LOOP('',(#15075,#15076,#15077,#15078));
#3567=EDGE_LOOP('',(#15079,#15080,#15081,#15082));
#3568=EDGE_LOOP('',(#15083,#15084,#15085,#15086));
#3569=EDGE_LOOP('',(#15087,#15088,#15089,#15090));
#3570=EDGE_LOOP('',(#15091,#15092,#15093,#15094));
#3571=EDGE_LOOP('',(#15095,#15096,#15097,#15098));
#3572=EDGE_LOOP('',(#15099,#15100,#15101,#15102));
#3573=EDGE_LOOP('',(#15103,#15104,#15105,#15106));
#3574=EDGE_LOOP('',(#15107,#15108,#15109,#15110));
#3575=EDGE_LOOP('',(#15111,#15112,#15113,#15114));
#3576=EDGE_LOOP('',(#15115,#15116,#15117,#15118,#15119,#15120,#15121,#15122));
#3577=EDGE_LOOP('',(#15123));
#3578=EDGE_LOOP('',(#15124));
#3579=EDGE_LOOP('',(#15125));
#3580=EDGE_LOOP('',(#15126));
#3581=EDGE_LOOP('',(#15127));
#3582=EDGE_LOOP('',(#15128));
#3583=EDGE_LOOP('',(#15129));
#3584=EDGE_LOOP('',(#15130,#15131,#15132,#15133));
#3585=EDGE_LOOP('',(#15134,#15135,#15136,#15137));
#3586=EDGE_LOOP('',(#15138,#15139,#15140,#15141));
#3587=EDGE_LOOP('',(#15142,#15143,#15144,#15145));
#3588=EDGE_LOOP('',(#15146,#15147,#15148,#15149));
#3589=EDGE_LOOP('',(#15150,#15151,#15152,#15153));
#3590=EDGE_LOOP('',(#15154,#15155,#15156,#15157));
#3591=EDGE_LOOP('',(#15158,#15159,#15160,#15161));
#3592=EDGE_LOOP('',(#15162,#15163,#15164,#15165));
#3593=EDGE_LOOP('',(#15166,#15167,#15168,#15169));
#3594=EDGE_LOOP('',(#15170,#15171,#15172,#15173));
#3595=EDGE_LOOP('',(#15174,#15175,#15176,#15177));
#3596=EDGE_LOOP('',(#15178,#15179,#15180,#15181));
#3597=EDGE_LOOP('',(#15182,#15183,#15184,#15185));
#3598=EDGE_LOOP('',(#15186,#15187,#15188,#15189));
#3599=EDGE_LOOP('',(#15190,#15191,#15192,#15193));
#3600=EDGE_LOOP('',(#15194,#15195,#15196,#15197));
#3601=EDGE_LOOP('',(#15198,#15199,#15200,#15201));
#3602=EDGE_LOOP('',(#15202,#15203,#15204,#15205));
#3603=EDGE_LOOP('',(#15206,#15207,#15208,#15209));
#3604=EDGE_LOOP('',(#15210,#15211,#15212,#15213));
#3605=EDGE_LOOP('',(#15214,#15215,#15216,#15217));
#3606=EDGE_LOOP('',(#15218,#15219,#15220,#15221));
#3607=EDGE_LOOP('',(#15222,#15223,#15224,#15225));
#3608=EDGE_LOOP('',(#15226,#15227,#15228,#15229));
#3609=EDGE_LOOP('',(#15230,#15231,#15232,#15233));
#3610=EDGE_LOOP('',(#15234,#15235,#15236,#15237));
#3611=EDGE_LOOP('',(#15238,#15239,#15240,#15241,#15242,#15243,#15244,#15245));
#3612=EDGE_LOOP('',(#15246));
#3613=EDGE_LOOP('',(#15247));
#3614=EDGE_LOOP('',(#15248));
#3615=EDGE_LOOP('',(#15249));
#3616=EDGE_LOOP('',(#15250));
#3617=EDGE_LOOP('',(#15251));
#3618=EDGE_LOOP('',(#15252));
#3619=EDGE_LOOP('',(#15253,#15254,#15255,#15256));
#3620=EDGE_LOOP('',(#15257,#15258,#15259,#15260));
#3621=EDGE_LOOP('',(#15261,#15262,#15263,#15264));
#3622=EDGE_LOOP('',(#15265,#15266,#15267,#15268));
#3623=EDGE_LOOP('',(#15269,#15270,#15271,#15272));
#3624=EDGE_LOOP('',(#15273,#15274,#15275,#15276));
#3625=EDGE_LOOP('',(#15277,#15278,#15279,#15280));
#3626=EDGE_LOOP('',(#15281,#15282,#15283,#15284));
#3627=EDGE_LOOP('',(#15285,#15286,#15287,#15288));
#3628=EDGE_LOOP('',(#15289,#15290,#15291,#15292));
#3629=EDGE_LOOP('',(#15293,#15294,#15295,#15296));
#3630=EDGE_LOOP('',(#15297,#15298,#15299,#15300,#15301));
#3631=EDGE_LOOP('',(#15302,#15303,#15304,#15305,#15306));
#3632=EDGE_LOOP('',(#15307,#15308,#15309,#15310,#15311));
#3633=EDGE_LOOP('',(#15312,#15313,#15314,#15315,#15316));
#3634=EDGE_LOOP('',(#15317,#15318,#15319,#15320,#15321));
#3635=EDGE_LOOP('',(#15322,#15323,#15324,#15325,#15326));
#3636=EDGE_LOOP('',(#15327,#15328,#15329,#15330,#15331));
#3637=EDGE_LOOP('',(#15332,#15333,#15334,#15335,#15336));
#3638=EDGE_LOOP('',(#15337,#15338,#15339,#15340,#15341));
#3639=EDGE_LOOP('',(#15342,#15343,#15344,#15345,#15346));
#3640=EDGE_LOOP('',(#15347,#15348,#15349,#15350,#15351));
#3641=EDGE_LOOP('',(#15352,#15353,#15354,#15355,#15356));
#3642=EDGE_LOOP('',(#15357,#15358,#15359,#15360,#15361));
#3643=EDGE_LOOP('',(#15362,#15363,#15364,#15365,#15366));
#3644=EDGE_LOOP('',(#15367,#15368,#15369,#15370));
#3645=EDGE_LOOP('',(#15371,#15372,#15373,#15374));
#3646=EDGE_LOOP('',(#15375,#15376,#15377,#15378));
#3647=EDGE_LOOP('',(#15379));
#3648=EDGE_LOOP('',(#15380));
#3649=EDGE_LOOP('',(#15381,#15382,#15383,#15384));
#3650=EDGE_LOOP('',(#15385,#15386,#15387,#15388));
#3651=EDGE_LOOP('',(#15389,#15390,#15391,#15392));
#3652=EDGE_LOOP('',(#15393));
#3653=EDGE_LOOP('',(#15394));
#3654=EDGE_LOOP('',(#15395,#15396,#15397,#15398));
#3655=EDGE_LOOP('',(#15399,#15400,#15401,#15402));
#3656=EDGE_LOOP('',(#15403,#15404,#15405,#15406));
#3657=EDGE_LOOP('',(#15407));
#3658=EDGE_LOOP('',(#15408));
#3659=EDGE_LOOP('',(#15409,#15410,#15411,#15412));
#3660=EDGE_LOOP('',(#15413,#15414,#15415,#15416));
#3661=EDGE_LOOP('',(#15417,#15418,#15419,#15420));
#3662=EDGE_LOOP('',(#15421));
#3663=EDGE_LOOP('',(#15422));
#3664=EDGE_LOOP('',(#15423,#15424,#15425,#15426));
#3665=EDGE_LOOP('',(#15427,#15428,#15429,#15430));
#3666=EDGE_LOOP('',(#15431,#15432,#15433,#15434));
#3667=EDGE_LOOP('',(#15435));
#3668=EDGE_LOOP('',(#15436));
#3669=EDGE_LOOP('',(#15437,#15438,#15439,#15440));
#3670=EDGE_LOOP('',(#15441,#15442,#15443,#15444));
#3671=EDGE_LOOP('',(#15445,#15446,#15447,#15448));
#3672=EDGE_LOOP('',(#15449));
#3673=EDGE_LOOP('',(#15450));
#3674=EDGE_LOOP('',(#15451,#15452,#15453,#15454));
#3675=EDGE_LOOP('',(#15455,#15456,#15457,#15458));
#3676=EDGE_LOOP('',(#15459,#15460,#15461,#15462));
#3677=EDGE_LOOP('',(#15463));
#3678=EDGE_LOOP('',(#15464));
#3679=EDGE_LOOP('',(#15465,#15466,#15467,#15468));
#3680=EDGE_LOOP('',(#15469,#15470,#15471,#15472));
#3681=EDGE_LOOP('',(#15473,#15474,#15475,#15476));
#3682=EDGE_LOOP('',(#15477,#15478,#15479,#15480));
#3683=EDGE_LOOP('',(#15481,#15482,#15483,#15484));
#3684=EDGE_LOOP('',(#15485,#15486,#15487,#15488));
#3685=EDGE_LOOP('',(#15489,#15490,#15491,#15492));
#3686=EDGE_LOOP('',(#15493,#15494,#15495,#15496));
#3687=EDGE_LOOP('',(#15497,#15498,#15499,#15500));
#3688=EDGE_LOOP('',(#15501,#15502,#15503,#15504));
#3689=EDGE_LOOP('',(#15505,#15506,#15507,#15508));
#3690=EDGE_LOOP('',(#15509,#15510,#15511,#15512));
#3691=EDGE_LOOP('',(#15513,#15514,#15515,#15516));
#3692=EDGE_LOOP('',(#15517,#15518,#15519,#15520));
#3693=EDGE_LOOP('',(#15521,#15522,#15523,#15524));
#3694=EDGE_LOOP('',(#15525,#15526,#15527,#15528,#15529,#15530));
#3695=EDGE_LOOP('',(#15531));
#3696=EDGE_LOOP('',(#15532));
#3697=EDGE_LOOP('',(#15533));
#3698=EDGE_LOOP('',(#15534));
#3699=EDGE_LOOP('',(#15535));
#3700=EDGE_LOOP('',(#15536));
#3701=EDGE_LOOP('',(#15537));
#3702=EDGE_LOOP('',(#15538,#15539,#15540,#15541,#15542,#15543));
#3703=EDGE_LOOP('',(#15544,#15545,#15546,#15547));
#3704=EDGE_LOOP('',(#15548));
#3705=EDGE_LOOP('',(#15549));
#3706=EDGE_LOOP('',(#15550));
#3707=EDGE_LOOP('',(#15551,#15552,#15553,#15554,#15555,#15556));
#3708=EDGE_LOOP('',(#15557,#15558,#15559,#15560,#15561));
#3709=EDGE_LOOP('',(#15562,#15563,#15564,#15565,#15566));
#3710=EDGE_LOOP('',(#15567,#15568,#15569,#15570));
#3711=EDGE_LOOP('',(#15571,#15572,#15573,#15574));
#3712=EDGE_LOOP('',(#15575,#15576,#15577,#15578));
#3713=EDGE_LOOP('',(#15579,#15580,#15581,#15582));
#3714=EDGE_LOOP('',(#15583,#15584,#15585,#15586));
#3715=EDGE_LOOP('',(#15587,#15588,#15589,#15590));
#3716=EDGE_LOOP('',(#15591,#15592,#15593,#15594,#15595,#15596));
#3717=EDGE_LOOP('',(#15597,#15598,#15599,#15600,#15601,#15602));
#3718=EDGE_LOOP('',(#15603,#15604,#15605,#15606));
#3719=EDGE_LOOP('',(#15607,#15608,#15609,#15610,#15611));
#3720=EDGE_LOOP('',(#15612,#15613,#15614,#15615,#15616));
#3721=EDGE_LOOP('',(#15617,#15618,#15619,#15620));
#3722=EDGE_LOOP('',(#15621,#15622,#15623,#15624));
#3723=EDGE_LOOP('',(#15625,#15626,#15627,#15628));
#3724=EDGE_LOOP('',(#15629,#15630,#15631,#15632));
#3725=EDGE_LOOP('',(#15633,#15634,#15635,#15636));
#3726=EDGE_LOOP('',(#15637,#15638,#15639,#15640));
#3727=EDGE_LOOP('',(#15641,#15642,#15643,#15644));
#3728=EDGE_LOOP('',(#15645,#15646,#15647,#15648));
#3729=EDGE_LOOP('',(#15649,#15650,#15651,#15652));
#3730=EDGE_LOOP('',(#15653,#15654,#15655,#15656));
#3731=EDGE_LOOP('',(#15657,#15658,#15659,#15660));
#3732=EDGE_LOOP('',(#15661,#15662,#15663,#15664));
#3733=EDGE_LOOP('',(#15665,#15666,#15667,#15668));
#3734=EDGE_LOOP('',(#15669,#15670,#15671,#15672));
#3735=EDGE_LOOP('',(#15673,#15674,#15675,#15676));
#3736=EDGE_LOOP('',(#15677,#15678,#15679,#15680));
#3737=EDGE_LOOP('',(#15681,#15682,#15683,#15684,#15685,#15686));
#3738=EDGE_LOOP('',(#15687));
#3739=EDGE_LOOP('',(#15688));
#3740=EDGE_LOOP('',(#15689));
#3741=EDGE_LOOP('',(#15690));
#3742=EDGE_LOOP('',(#15691));
#3743=EDGE_LOOP('',(#15692));
#3744=EDGE_LOOP('',(#15693));
#3745=EDGE_LOOP('',(#15694));
#3746=EDGE_LOOP('',(#15695));
#3747=EDGE_LOOP('',(#15696));
#3748=EDGE_LOOP('',(#15697,#15698,#15699,#15700));
#3749=EDGE_LOOP('',(#15701,#15702,#15703,#15704));
#3750=EDGE_LOOP('',(#15705,#15706,#15707,#15708,#15709));
#3751=EDGE_LOOP('',(#15710,#15711,#15712,#15713,#15714));
#3752=EDGE_LOOP('',(#15715,#15716,#15717,#15718));
#3753=EDGE_LOOP('',(#15719));
#3754=EDGE_LOOP('',(#15720));
#3755=EDGE_LOOP('',(#15721,#15722,#15723,#15724,#15725));
#3756=EDGE_LOOP('',(#15726,#15727,#15728,#15729,#15730));
#3757=EDGE_LOOP('',(#15731,#15732,#15733,#15734));
#3758=EDGE_LOOP('',(#15735,#15736,#15737,#15738,#15739));
#3759=EDGE_LOOP('',(#15740,#15741,#15742,#15743,#15744));
#3760=EDGE_LOOP('',(#15745,#15746,#15747,#15748));
#3761=EDGE_LOOP('',(#15749,#15750,#15751,#15752,#15753));
#3762=EDGE_LOOP('',(#15754,#15755,#15756,#15757,#15758));
#3763=EDGE_LOOP('',(#15759,#15760,#15761,#15762));
#3764=EDGE_LOOP('',(#15763,#15764,#15765,#15766));
#3765=EDGE_LOOP('',(#15767,#15768,#15769,#15770));
#3766=EDGE_LOOP('',(#15771,#15772,#15773,#15774));
#3767=EDGE_LOOP('',(#15775,#15776,#15777,#15778));
#3768=EDGE_LOOP('',(#15779,#15780,#15781,#15782));
#3769=EDGE_LOOP('',(#15783,#15784,#15785,#15786));
#3770=EDGE_LOOP('',(#15787,#15788,#15789,#15790));
#3771=EDGE_LOOP('',(#15791,#15792,#15793,#15794,#15795));
#3772=EDGE_LOOP('',(#15796,#15797,#15798,#15799));
#3773=EDGE_LOOP('',(#15800));
#3774=EDGE_LOOP('',(#15801,#15802,#15803,#15804,#15805,#15806));
#3775=EDGE_LOOP('',(#15807,#15808,#15809,#15810,#15811));
#3776=EDGE_LOOP('',(#15812,#15813,#15814));
#3777=EDGE_LOOP('',(#15815,#15816,#15817));
#3778=EDGE_LOOP('',(#15818,#15819,#15820,#15821));
#3779=EDGE_LOOP('',(#15822,#15823,#15824,#15825));
#3780=EDGE_LOOP('',(#15826,#15827,#15828));
#3781=EDGE_LOOP('',(#15829,#15830,#15831,#15832));
#3782=EDGE_LOOP('',(#15833,#15834,#15835,#15836));
#3783=EDGE_LOOP('',(#15837,#15838,#15839));
#3784=EDGE_LOOP('',(#15840,#15841,#15842,#15843));
#3785=EDGE_LOOP('',(#15844,#15845,#15846,#15847));
#3786=EDGE_LOOP('',(#15848,#15849,#15850,#15851));
#3787=EDGE_LOOP('',(#15852,#15853,#15854,#15855));
#3788=EDGE_LOOP('',(#15856,#15857,#15858,#15859));
#3789=EDGE_LOOP('',(#15860,#15861,#15862));
#3790=EDGE_LOOP('',(#15863,#15864,#15865,#15866));
#3791=EDGE_LOOP('',(#15867,#15868,#15869,#15870));
#3792=EDGE_LOOP('',(#15871,#15872,#15873));
#3793=EDGE_LOOP('',(#15874,#15875,#15876,#15877));
#3794=EDGE_LOOP('',(#15878,#15879,#15880,#15881));
#3795=EDGE_LOOP('',(#15882,#15883,#15884));
#3796=EDGE_LOOP('',(#15885,#15886,#15887,#15888));
#3797=EDGE_LOOP('',(#15889,#15890,#15891,#15892));
#3798=EDGE_LOOP('',(#15893,#15894,#15895,#15896));
#3799=EDGE_LOOP('',(#15897,#15898,#15899,#15900));
#3800=EDGE_LOOP('',(#15901,#15902,#15903,#15904));
#3801=EDGE_LOOP('',(#15905,#15906,#15907,#15908));
#3802=EDGE_LOOP('',(#15909,#15910,#15911,#15912));
#3803=EDGE_LOOP('',(#15913,#15914,#15915,#15916));
#3804=EDGE_LOOP('',(#15917,#15918,#15919,#15920));
#3805=EDGE_LOOP('',(#15921,#15922,#15923,#15924));
#3806=EDGE_LOOP('',(#15925,#15926,#15927,#15928));
#3807=EDGE_LOOP('',(#15929,#15930,#15931,#15932));
#3808=EDGE_LOOP('',(#15933,#15934,#15935,#15936));
#3809=EDGE_LOOP('',(#15937,#15938,#15939,#15940));
#3810=EDGE_LOOP('',(#15941,#15942,#15943,#15944));
#3811=EDGE_LOOP('',(#15945,#15946,#15947,#15948));
#3812=EDGE_LOOP('',(#15949,#15950,#15951,#15952,#15953,#15954,#15955,#15956));
#3813=EDGE_LOOP('',(#15957));
#3814=EDGE_LOOP('',(#15958));
#3815=EDGE_LOOP('',(#15959));
#3816=EDGE_LOOP('',(#15960));
#3817=EDGE_LOOP('',(#15961,#15962,#15963,#15964));
#3818=EDGE_LOOP('',(#15965,#15966,#15967,#15968));
#3819=EDGE_LOOP('',(#15969,#15970,#15971,#15972));
#3820=EDGE_LOOP('',(#15973,#15974,#15975,#15976));
#3821=EDGE_LOOP('',(#15977,#15978,#15979,#15980));
#3822=EDGE_LOOP('',(#15981,#15982,#15983,#15984));
#3823=EDGE_LOOP('',(#15985,#15986,#15987,#15988));
#3824=EDGE_LOOP('',(#15989,#15990,#15991,#15992));
#3825=EDGE_LOOP('',(#15993,#15994,#15995,#15996));
#3826=EDGE_LOOP('',(#15997,#15998,#15999,#16000));
#3827=EDGE_LOOP('',(#16001,#16002,#16003,#16004));
#3828=EDGE_LOOP('',(#16005,#16006,#16007,#16008));
#3829=EDGE_LOOP('',(#16009,#16010,#16011,#16012));
#3830=EDGE_LOOP('',(#16013,#16014,#16015,#16016));
#3831=EDGE_LOOP('',(#16017,#16018,#16019,#16020));
#3832=EDGE_LOOP('',(#16021,#16022,#16023,#16024));
#3833=EDGE_LOOP('',(#16025,#16026,#16027,#16028));
#3834=EDGE_LOOP('',(#16029,#16030,#16031,#16032));
#3835=EDGE_LOOP('',(#16033,#16034,#16035,#16036));
#3836=EDGE_LOOP('',(#16037,#16038,#16039,#16040));
#3837=EDGE_LOOP('',(#16041,#16042,#16043,#16044));
#3838=EDGE_LOOP('',(#16045,#16046,#16047,#16048));
#3839=EDGE_LOOP('',(#16049,#16050,#16051,#16052));
#3840=EDGE_LOOP('',(#16053,#16054,#16055,#16056));
#3841=EDGE_LOOP('',(#16057,#16058,#16059,#16060));
#3842=EDGE_LOOP('',(#16061,#16062,#16063,#16064));
#3843=EDGE_LOOP('',(#16065,#16066,#16067,#16068,#16069));
#3844=EDGE_LOOP('',(#16070,#16071,#16072,#16073,#16074));
#3845=EDGE_LOOP('',(#16075,#16076,#16077,#16078));
#3846=EDGE_LOOP('',(#16079,#16080,#16081,#16082));
#3847=EDGE_LOOP('',(#16083,#16084,#16085,#16086));
#3848=EDGE_LOOP('',(#16087,#16088,#16089,#16090));
#3849=EDGE_LOOP('',(#16091,#16092,#16093,#16094));
#3850=EDGE_LOOP('',(#16095,#16096,#16097,#16098));
#3851=EDGE_LOOP('',(#16099,#16100,#16101,#16102));
#3852=EDGE_LOOP('',(#16103,#16104,#16105,#16106));
#3853=EDGE_LOOP('',(#16107,#16108,#16109,#16110));
#3854=EDGE_LOOP('',(#16111,#16112,#16113,#16114));
#3855=EDGE_LOOP('',(#16115,#16116,#16117,#16118));
#3856=EDGE_LOOP('',(#16119,#16120,#16121,#16122,#16123,#16124,#16125,#16126));
#3857=EDGE_LOOP('',(#16127));
#3858=EDGE_LOOP('',(#16128,#16129,#16130,#16131));
#3859=EDGE_LOOP('',(#16132,#16133,#16134,#16135));
#3860=EDGE_LOOP('',(#16136));
#3861=EDGE_LOOP('',(#16137));
#3862=EDGE_LOOP('',(#16138,#16139,#16140,#16141));
#3863=EDGE_LOOP('',(#16142,#16143,#16144,#16145));
#3864=EDGE_LOOP('',(#16146,#16147,#16148,#16149));
#3865=EDGE_LOOP('',(#16150,#16151,#16152));
#3866=EDGE_LOOP('',(#16153,#16154,#16155,#16156));
#3867=EDGE_LOOP('',(#16157,#16158,#16159,#16160));
#3868=EDGE_LOOP('',(#16161,#16162,#16163));
#3869=EDGE_LOOP('',(#16164,#16165,#16166,#16167));
#3870=EDGE_LOOP('',(#16168,#16169,#16170,#16171));
#3871=EDGE_LOOP('',(#16172,#16173,#16174));
#3872=EDGE_LOOP('',(#16175,#16176,#16177,#16178));
#3873=EDGE_LOOP('',(#16179,#16180,#16181,#16182));
#3874=EDGE_LOOP('',(#16183,#16184,#16185,#16186));
#3875=EDGE_LOOP('',(#16187,#16188,#16189,#16190));
#3876=EDGE_LOOP('',(#16191,#16192,#16193,#16194));
#3877=EDGE_LOOP('',(#16195,#16196,#16197,#16198));
#3878=EDGE_LOOP('',(#16199,#16200,#16201,#16202));
#3879=EDGE_LOOP('',(#16203,#16204,#16205,#16206));
#3880=EDGE_LOOP('',(#16207,#16208,#16209,#16210));
#3881=EDGE_LOOP('',(#16211,#16212,#16213,#16214,#16215));
#3882=EDGE_LOOP('',(#16216,#16217,#16218,#16219,#16220,#16221));
#3883=EDGE_LOOP('',(#16222,#16223,#16224,#16225));
#3884=EDGE_LOOP('',(#16226,#16227,#16228,#16229,#16230));
#3885=EDGE_LOOP('',(#16231,#16232,#16233,#16234));
#3886=EDGE_LOOP('',(#16235,#16236,#16237,#16238));
#3887=EDGE_LOOP('',(#16239));
#3888=EDGE_LOOP('',(#16240));
#3889=EDGE_LOOP('',(#16241));
#3890=EDGE_LOOP('',(#16242));
#3891=EDGE_LOOP('',(#16243));
#3892=EDGE_LOOP('',(#16244,#16245,#16246,#16247));
#3893=EDGE_LOOP('',(#16248,#16249,#16250,#16251));
#3894=EDGE_LOOP('',(#16252,#16253,#16254,#16255));
#3895=EDGE_LOOP('',(#16256));
#3896=EDGE_LOOP('',(#16257));
#3897=EDGE_LOOP('',(#16258,#16259,#16260,#16261,#16262));
#3898=EDGE_LOOP('',(#16263,#16264,#16265,#16266,#16267,#16268));
#3899=EDGE_LOOP('',(#16269,#16270,#16271,#16272));
#3900=EDGE_LOOP('',(#16273,#16274,#16275,#16276));
#3901=EDGE_LOOP('',(#16277,#16278,#16279,#16280,#16281));
#3902=EDGE_LOOP('',(#16282,#16283,#16284));
#3903=EDGE_LOOP('',(#16285,#16286,#16287,#16288));
#3904=EDGE_LOOP('',(#16289,#16290,#16291,#16292));
#3905=EDGE_LOOP('',(#16293,#16294,#16295));
#3906=EDGE_LOOP('',(#16296,#16297,#16298,#16299));
#3907=EDGE_LOOP('',(#16300,#16301,#16302,#16303));
#3908=EDGE_LOOP('',(#16304,#16305,#16306));
#3909=EDGE_LOOP('',(#16307,#16308,#16309,#16310));
#3910=EDGE_LOOP('',(#16311,#16312,#16313,#16314));
#3911=EDGE_LOOP('',(#16315,#16316,#16317,#16318,#16319));
#3912=EDGE_LOOP('',(#16320,#16321,#16322,#16323,#16324));
#3913=EDGE_LOOP('',(#16325));
#3914=EDGE_LOOP('',(#16326));
#3915=EDGE_LOOP('',(#16327));
#3916=EDGE_LOOP('',(#16328));
#3917=EDGE_LOOP('',(#16329));
#3918=EDGE_LOOP('',(#16330));
#3919=EDGE_LOOP('',(#16331));
#3920=EDGE_LOOP('',(#16332));
#3921=EDGE_LOOP('',(#16333,#16334,#16335,#16336));
#3922=EDGE_LOOP('',(#16337));
#3923=EDGE_LOOP('',(#16338));
#3924=EDGE_LOOP('',(#16339));
#3925=EDGE_LOOP('',(#16340));
#3926=EDGE_LOOP('',(#16341));
#3927=EDGE_LOOP('',(#16342));
#3928=EDGE_LOOP('',(#16343));
#3929=EDGE_LOOP('',(#16344));
#3930=EDGE_LOOP('',(#16345,#16346,#16347,#16348,#16349));
#3931=EDGE_LOOP('',(#16350,#16351,#16352,#16353,#16354));
#3932=EDGE_LOOP('',(#16355,#16356,#16357,#16358));
#3933=EDGE_LOOP('',(#16359,#16360,#16361,#16362,#16363));
#3934=EDGE_LOOP('',(#16364,#16365,#16366,#16367,#16368));
#3935=EDGE_LOOP('',(#16369,#16370,#16371,#16372));
#3936=EDGE_LOOP('',(#16373,#16374,#16375,#16376,#16377));
#3937=EDGE_LOOP('',(#16378,#16379,#16380,#16381,#16382));
#3938=EDGE_LOOP('',(#16383,#16384,#16385,#16386));
#3939=EDGE_LOOP('',(#16387,#16388,#16389,#16390,#16391));
#3940=EDGE_LOOP('',(#16392,#16393,#16394,#16395,#16396));
#3941=EDGE_LOOP('',(#16397,#16398,#16399,#16400));
#3942=EDGE_LOOP('',(#16401,#16402,#16403,#16404,#16405));
#3943=EDGE_LOOP('',(#16406,#16407,#16408,#16409,#16410));
#3944=EDGE_LOOP('',(#16411,#16412,#16413,#16414));
#3945=EDGE_LOOP('',(#16415,#16416,#16417,#16418,#16419));
#3946=EDGE_LOOP('',(#16420,#16421,#16422,#16423,#16424,#16425));
#3947=EDGE_LOOP('',(#16426,#16427,#16428,#16429,#16430));
#3948=EDGE_LOOP('',(#16431,#16432,#16433,#16434,#16435));
#3949=EDGE_LOOP('',(#16436,#16437,#16438,#16439,#16440,#16441));
#3950=EDGE_LOOP('',(#16442,#16443,#16444,#16445,#16446));
#3951=EDGE_LOOP('',(#16447,#16448,#16449,#16450,#16451,#16452,#16453,#16454));
#3952=EDGE_LOOP('',(#16455,#16456,#16457,#16458));
#3953=EDGE_LOOP('',(#16459,#16460,#16461,#16462));
#3954=EDGE_LOOP('',(#16463,#16464,#16465,#16466));
#3955=EDGE_LOOP('',(#16467,#16468,#16469,#16470));
#3956=EDGE_LOOP('',(#16471,#16472,#16473,#16474));
#3957=EDGE_LOOP('',(#16475,#16476,#16477,#16478));
#3958=EDGE_LOOP('',(#16479,#16480,#16481,#16482));
#3959=EDGE_LOOP('',(#16483,#16484,#16485,#16486));
#3960=EDGE_LOOP('',(#16487,#16488,#16489,#16490));
#3961=EDGE_LOOP('',(#16491,#16492,#16493,#16494));
#3962=EDGE_LOOP('',(#16495,#16496,#16497,#16498));
#3963=EDGE_LOOP('',(#16499,#16500,#16501,#16502));
#3964=EDGE_LOOP('',(#16503,#16504,#16505,#16506));
#3965=EDGE_LOOP('',(#16507,#16508,#16509,#16510));
#3966=EDGE_LOOP('',(#16511,#16512,#16513,#16514));
#3967=EDGE_LOOP('',(#16515,#16516,#16517,#16518));
#3968=EDGE_LOOP('',(#16519,#16520,#16521,#16522));
#3969=EDGE_LOOP('',(#16523,#16524,#16525,#16526));
#3970=EDGE_LOOP('',(#16527,#16528,#16529,#16530));
#3971=EDGE_LOOP('',(#16531,#16532,#16533,#16534));
#3972=EDGE_LOOP('',(#16535,#16536,#16537,#16538,#16539,#16540,#16541,#16542,
#16543,#16544,#16545,#16546,#16547,#16548,#16549,#16550,#16551,#16552,#16553,
#16554,#16555,#16556,#16557,#16558,#16559));
#3973=EDGE_LOOP('',(#16560,#16561,#16562,#16563));
#3974=EDGE_LOOP('',(#16564,#16565,#16566,#16567));
#3975=EDGE_LOOP('',(#16568,#16569,#16570,#16571,#16572,#16573,#16574,#16575,
#16576,#16577,#16578,#16579,#16580,#16581,#16582,#16583,#16584,#16585,#16586,
#16587,#16588,#16589,#16590,#16591,#16592,#16593));
#3976=EDGE_LOOP('',(#16594,#16595,#16596,#16597));
#3977=EDGE_LOOP('',(#16598,#16599,#16600,#16601));
#3978=EDGE_LOOP('',(#16602,#16603,#16604,#16605));
#3979=EDGE_LOOP('',(#16606,#16607,#16608,#16609));
#3980=EDGE_LOOP('',(#16610,#16611,#16612,#16613));
#3981=EDGE_LOOP('',(#16614,#16615,#16616));
#3982=EDGE_LOOP('',(#16617,#16618,#16619,#16620));
#3983=EDGE_LOOP('',(#16621,#16622,#16623));
#3984=EDGE_LOOP('',(#16624,#16625,#16626,#16627));
#3985=EDGE_LOOP('',(#16628,#16629,#16630));
#3986=EDGE_LOOP('',(#16631,#16632,#16633,#16634));
#3987=EDGE_LOOP('',(#16635,#16636,#16637));
#3988=EDGE_LOOP('',(#16638,#16639,#16640,#16641));
#3989=EDGE_LOOP('',(#16642,#16643,#16644));
#3990=EDGE_LOOP('',(#16645,#16646,#16647,#16648));
#3991=EDGE_LOOP('',(#16649,#16650,#16651));
#3992=EDGE_LOOP('',(#16652,#16653,#16654,#16655));
#3993=EDGE_LOOP('',(#16656,#16657,#16658));
#3994=EDGE_LOOP('',(#16659,#16660,#16661,#16662));
#3995=EDGE_LOOP('',(#16663,#16664,#16665));
#3996=EDGE_LOOP('',(#16666,#16667,#16668,#16669));
#3997=EDGE_LOOP('',(#16670,#16671,#16672));
#3998=EDGE_LOOP('',(#16673,#16674,#16675,#16676));
#3999=EDGE_LOOP('',(#16677,#16678,#16679));
#4000=EDGE_LOOP('',(#16680,#16681,#16682,#16683));
#4001=EDGE_LOOP('',(#16684,#16685,#16686));
#4002=EDGE_LOOP('',(#16687,#16688,#16689,#16690));
#4003=EDGE_LOOP('',(#16691,#16692,#16693));
#4004=EDGE_LOOP('',(#16694,#16695,#16696,#16697));
#4005=EDGE_LOOP('',(#16698,#16699,#16700));
#4006=EDGE_LOOP('',(#16701,#16702,#16703,#16704));
#4007=EDGE_LOOP('',(#16705,#16706,#16707));
#4008=EDGE_LOOP('',(#16708,#16709,#16710,#16711));
#4009=EDGE_LOOP('',(#16712,#16713,#16714));
#4010=EDGE_LOOP('',(#16715,#16716,#16717,#16718));
#4011=EDGE_LOOP('',(#16719,#16720,#16721));
#4012=EDGE_LOOP('',(#16722,#16723,#16724,#16725));
#4013=EDGE_LOOP('',(#16726,#16727,#16728));
#4014=EDGE_LOOP('',(#16729,#16730,#16731,#16732));
#4015=EDGE_LOOP('',(#16733,#16734,#16735));
#4016=EDGE_LOOP('',(#16736,#16737,#16738,#16739));
#4017=EDGE_LOOP('',(#16740,#16741,#16742));
#4018=EDGE_LOOP('',(#16743,#16744,#16745,#16746));
#4019=EDGE_LOOP('',(#16747,#16748,#16749));
#4020=EDGE_LOOP('',(#16750,#16751,#16752,#16753));
#4021=EDGE_LOOP('',(#16754,#16755,#16756));
#4022=EDGE_LOOP('',(#16757,#16758,#16759,#16760));
#4023=EDGE_LOOP('',(#16761,#16762,#16763));
#4024=EDGE_LOOP('',(#16764,#16765,#16766,#16767));
#4025=EDGE_LOOP('',(#16768,#16769,#16770,#16771));
#4026=EDGE_LOOP('',(#16772,#16773,#16774,#16775));
#4027=EDGE_LOOP('',(#16776,#16777,#16778,#16779));
#4028=EDGE_LOOP('',(#16780,#16781,#16782,#16783));
#4029=EDGE_LOOP('',(#16784,#16785,#16786));
#4030=EDGE_LOOP('',(#16787,#16788,#16789,#16790));
#4031=EDGE_LOOP('',(#16791,#16792,#16793));
#4032=EDGE_LOOP('',(#16794,#16795,#16796,#16797));
#4033=EDGE_LOOP('',(#16798,#16799,#16800));
#4034=EDGE_LOOP('',(#16801,#16802,#16803,#16804));
#4035=EDGE_LOOP('',(#16805,#16806,#16807));
#4036=EDGE_LOOP('',(#16808,#16809,#16810,#16811));
#4037=EDGE_LOOP('',(#16812,#16813,#16814));
#4038=EDGE_LOOP('',(#16815,#16816,#16817,#16818));
#4039=EDGE_LOOP('',(#16819,#16820,#16821));
#4040=EDGE_LOOP('',(#16822,#16823,#16824,#16825));
#4041=EDGE_LOOP('',(#16826,#16827,#16828));
#4042=EDGE_LOOP('',(#16829,#16830,#16831,#16832));
#4043=EDGE_LOOP('',(#16833,#16834,#16835));
#4044=EDGE_LOOP('',(#16836,#16837,#16838,#16839));
#4045=EDGE_LOOP('',(#16840,#16841,#16842));
#4046=EDGE_LOOP('',(#16843,#16844,#16845,#16846));
#4047=EDGE_LOOP('',(#16847,#16848,#16849));
#4048=EDGE_LOOP('',(#16850,#16851,#16852,#16853));
#4049=EDGE_LOOP('',(#16854,#16855,#16856));
#4050=EDGE_LOOP('',(#16857,#16858,#16859,#16860));
#4051=EDGE_LOOP('',(#16861,#16862,#16863));
#4052=EDGE_LOOP('',(#16864,#16865,#16866,#16867));
#4053=EDGE_LOOP('',(#16868,#16869,#16870));
#4054=EDGE_LOOP('',(#16871,#16872,#16873,#16874));
#4055=EDGE_LOOP('',(#16875,#16876,#16877));
#4056=EDGE_LOOP('',(#16878,#16879,#16880,#16881));
#4057=EDGE_LOOP('',(#16882,#16883,#16884));
#4058=EDGE_LOOP('',(#16885,#16886,#16887,#16888));
#4059=EDGE_LOOP('',(#16889,#16890,#16891));
#4060=EDGE_LOOP('',(#16892,#16893,#16894,#16895));
#4061=EDGE_LOOP('',(#16896,#16897,#16898));
#4062=EDGE_LOOP('',(#16899,#16900,#16901,#16902));
#4063=EDGE_LOOP('',(#16903,#16904,#16905));
#4064=EDGE_LOOP('',(#16906,#16907,#16908,#16909));
#4065=EDGE_LOOP('',(#16910,#16911,#16912));
#4066=EDGE_LOOP('',(#16913,#16914,#16915,#16916));
#4067=EDGE_LOOP('',(#16917,#16918,#16919));
#4068=EDGE_LOOP('',(#16920,#16921,#16922,#16923));
#4069=EDGE_LOOP('',(#16924,#16925,#16926));
#4070=EDGE_LOOP('',(#16927,#16928,#16929,#16930));
#4071=EDGE_LOOP('',(#16931,#16932,#16933));
#4072=EDGE_LOOP('',(#16934,#16935,#16936,#16937));
#4073=EDGE_LOOP('',(#16938,#16939,#16940));
#4074=EDGE_LOOP('',(#16941,#16942,#16943,#16944));
#4075=EDGE_LOOP('',(#16945,#16946,#16947));
#4076=EDGE_LOOP('',(#16948,#16949,#16950,#16951));
#4077=EDGE_LOOP('',(#16952,#16953,#16954,#16955));
#4078=EDGE_LOOP('',(#16956));
#4079=EDGE_LOOP('',(#16957));
#4080=EDGE_LOOP('',(#16958));
#4081=EDGE_LOOP('',(#16959,#16960,#16961,#16962));
#4082=EDGE_LOOP('',(#16963,#16964,#16965,#16966,#16967,#16968,#16969,#16970,
#16971,#16972,#16973,#16974));
#4083=EDGE_LOOP('',(#16975,#16976,#16977,#16978));
#4084=EDGE_LOOP('',(#16979,#16980,#16981,#16982));
#4085=EDGE_LOOP('',(#16983,#16984,#16985,#16986));
#4086=EDGE_LOOP('',(#16987,#16988,#16989,#16990));
#4087=EDGE_LOOP('',(#16991,#16992,#16993,#16994));
#4088=EDGE_LOOP('',(#16995,#16996,#16997,#16998));
#4089=EDGE_LOOP('',(#16999,#17000,#17001,#17002));
#4090=EDGE_LOOP('',(#17003,#17004,#17005,#17006));
#4091=EDGE_LOOP('',(#17007,#17008,#17009,#17010));
#4092=EDGE_LOOP('',(#17011,#17012,#17013,#17014));
#4093=EDGE_LOOP('',(#17015,#17016,#17017,#17018));
#4094=EDGE_LOOP('',(#17019,#17020,#17021,#17022));
#4095=EDGE_LOOP('',(#17023,#17024,#17025,#17026));
#4096=EDGE_LOOP('',(#17027,#17028,#17029,#17030));
#4097=EDGE_LOOP('',(#17031,#17032,#17033,#17034));
#4098=EDGE_LOOP('',(#17035,#17036,#17037,#17038));
#4099=EDGE_LOOP('',(#17039,#17040,#17041,#17042));
#4100=EDGE_LOOP('',(#17043,#17044,#17045,#17046));
#4101=EDGE_LOOP('',(#17047,#17048,#17049,#17050));
#4102=EDGE_LOOP('',(#17051,#17052,#17053,#17054));
#4103=EDGE_LOOP('',(#17055,#17056,#17057,#17058));
#4104=EDGE_LOOP('',(#17059,#17060,#17061,#17062));
#4105=EDGE_LOOP('',(#17063,#17064,#17065,#17066));
#4106=EDGE_LOOP('',(#17067));
#4107=EDGE_LOOP('',(#17068));
#4108=EDGE_LOOP('',(#17069,#17070,#17071,#17072));
#4109=EDGE_LOOP('',(#17073,#17074,#17075,#17076));
#4110=EDGE_LOOP('',(#17077));
#4111=EDGE_LOOP('',(#17078));
#4112=EDGE_LOOP('',(#17079,#17080,#17081,#17082));
#4113=EDGE_LOOP('',(#17083,#17084,#17085,#17086));
#4114=EDGE_LOOP('',(#17087,#17088,#17089,#17090));
#4115=EDGE_LOOP('',(#17091,#17092,#17093,#17094));
#4116=EDGE_LOOP('',(#17095,#17096,#17097,#17098));
#4117=EDGE_LOOP('',(#17099,#17100,#17101,#17102));
#4118=EDGE_LOOP('',(#17103,#17104,#17105,#17106,#17107,#17108));
#4119=EDGE_LOOP('',(#17109));
#4120=EDGE_LOOP('',(#17110,#17111,#17112,#17113));
#4121=EDGE_LOOP('',(#17114));
#4122=EDGE_LOOP('',(#17115));
#4123=EDGE_LOOP('',(#17116));
#4124=EDGE_LOOP('',(#17117));
#4125=EDGE_LOOP('',(#17118,#17119,#17120,#17121));
#4126=EDGE_LOOP('',(#17122,#17123,#17124,#17125));
#4127=EDGE_LOOP('',(#17126,#17127,#17128,#17129));
#4128=EDGE_LOOP('',(#17130,#17131,#17132,#17133));
#4129=EDGE_LOOP('',(#17134,#17135,#17136,#17137));
#4130=EDGE_LOOP('',(#17138,#17139,#17140,#17141));
#4131=EDGE_LOOP('',(#17142));
#4132=EDGE_LOOP('',(#17143));
#4133=EDGE_LOOP('',(#17144));
#4134=EDGE_LOOP('',(#17145));
#4135=EDGE_LOOP('',(#17146,#17147,#17148,#17149,#17150,#17151));
#4136=EDGE_LOOP('',(#17152));
#4137=EDGE_LOOP('',(#17153,#17154,#17155,#17156));
#4138=EDGE_LOOP('',(#17157,#17158,#17159,#17160));
#4139=EDGE_LOOP('',(#17161,#17162,#17163,#17164,#17165));
#4140=EDGE_LOOP('',(#17166,#17167,#17168,#17169,#17170,#17171));
#4141=EDGE_LOOP('',(#17172));
#4142=EDGE_LOOP('',(#17173,#17174,#17175,#17176,#17177));
#4143=EDGE_LOOP('',(#17178));
#4144=EDGE_LOOP('',(#17179,#17180,#17181,#17182));
#4145=EDGE_LOOP('',(#17183));
#4146=EDGE_LOOP('',(#17184));
#4147=EDGE_LOOP('',(#17185));
#4148=EDGE_LOOP('',(#17186));
#4149=EDGE_LOOP('',(#17187,#17188,#17189,#17190,#17191));
#4150=EDGE_LOOP('',(#17192,#17193,#17194,#17195));
#4151=EDGE_LOOP('',(#17196));
#4152=EDGE_LOOP('',(#17197));
#4153=EDGE_LOOP('',(#17198));
#4154=EDGE_LOOP('',(#17199));
#4155=EDGE_LOOP('',(#17200,#17201,#17202,#17203));
#4156=EDGE_LOOP('',(#17204,#17205,#17206,#17207,#17208));
#4157=EDGE_LOOP('',(#17209,#17210,#17211,#17212,#17213));
#4158=EDGE_LOOP('',(#17214));
#4159=EDGE_LOOP('',(#17215));
#4160=EDGE_LOOP('',(#17216,#17217,#17218,#17219,#17220));
#4161=EDGE_LOOP('',(#17221));
#4162=EDGE_LOOP('',(#17222));
#4163=EDGE_LOOP('',(#17223,#17224,#17225,#17226));
#4164=EDGE_LOOP('',(#17227,#17228,#17229,#17230,#17231,#17232));
#4165=EDGE_LOOP('',(#17233,#17234,#17235,#17236,#17237,#17238));
#4166=EDGE_LOOP('',(#17239,#17240,#17241,#17242,#17243));
#4167=EDGE_LOOP('',(#17244,#17245,#17246,#17247,#17248));
#4168=EDGE_LOOP('',(#17249));
#4169=EDGE_LOOP('',(#17250));
#4170=EDGE_LOOP('',(#17251,#17252,#17253,#17254));
#4171=EDGE_LOOP('',(#17255,#17256,#17257));
#4172=EDGE_LOOP('',(#17258,#17259,#17260,#17261));
#4173=EDGE_LOOP('',(#17262,#17263,#17264));
#4174=EDGE_LOOP('',(#17265,#17266,#17267,#17268));
#4175=EDGE_LOOP('',(#17269,#17270,#17271));
#4176=EDGE_LOOP('',(#17272,#17273,#17274,#17275));
#4177=EDGE_LOOP('',(#17276,#17277,#17278));
#4178=EDGE_LOOP('',(#17279,#17280,#17281,#17282));
#4179=EDGE_LOOP('',(#17283,#17284,#17285));
#4180=EDGE_LOOP('',(#17286,#17287,#17288,#17289));
#4181=EDGE_LOOP('',(#17290,#17291,#17292));
#4182=EDGE_LOOP('',(#17293,#17294,#17295,#17296));
#4183=EDGE_LOOP('',(#17297,#17298,#17299));
#4184=EDGE_LOOP('',(#17300,#17301,#17302,#17303));
#4185=EDGE_LOOP('',(#17304,#17305,#17306));
#4186=EDGE_LOOP('',(#17307,#17308,#17309,#17310));
#4187=EDGE_LOOP('',(#17311,#17312,#17313));
#4188=EDGE_LOOP('',(#17314,#17315,#17316,#17317));
#4189=EDGE_LOOP('',(#17318,#17319,#17320));
#4190=EDGE_LOOP('',(#17321,#17322,#17323,#17324));
#4191=EDGE_LOOP('',(#17325,#17326,#17327));
#4192=EDGE_LOOP('',(#17328,#17329,#17330,#17331));
#4193=EDGE_LOOP('',(#17332,#17333,#17334));
#4194=EDGE_LOOP('',(#17335,#17336,#17337,#17338));
#4195=EDGE_LOOP('',(#17339,#17340,#17341));
#4196=EDGE_LOOP('',(#17342,#17343,#17344,#17345));
#4197=EDGE_LOOP('',(#17346,#17347,#17348));
#4198=EDGE_LOOP('',(#17349,#17350,#17351,#17352));
#4199=EDGE_LOOP('',(#17353,#17354,#17355));
#4200=EDGE_LOOP('',(#17356,#17357,#17358,#17359));
#4201=EDGE_LOOP('',(#17360,#17361,#17362));
#4202=EDGE_LOOP('',(#17363,#17364,#17365,#17366));
#4203=EDGE_LOOP('',(#17367,#17368,#17369,#17370));
#4204=EDGE_LOOP('',(#17371,#17372,#17373,#17374));
#4205=EDGE_LOOP('',(#17375,#17376,#17377,#17378));
#4206=EDGE_LOOP('',(#17379,#17380,#17381,#17382));
#4207=EDGE_LOOP('',(#17383,#17384,#17385));
#4208=EDGE_LOOP('',(#17386,#17387,#17388,#17389));
#4209=EDGE_LOOP('',(#17390,#17391,#17392));
#4210=EDGE_LOOP('',(#17393,#17394,#17395,#17396));
#4211=EDGE_LOOP('',(#17397,#17398,#17399));
#4212=EDGE_LOOP('',(#17400,#17401,#17402,#17403));
#4213=EDGE_LOOP('',(#17404,#17405,#17406));
#4214=EDGE_LOOP('',(#17407,#17408,#17409,#17410));
#4215=EDGE_LOOP('',(#17411,#17412,#17413));
#4216=EDGE_LOOP('',(#17414,#17415,#17416,#17417));
#4217=EDGE_LOOP('',(#17418,#17419,#17420));
#4218=EDGE_LOOP('',(#17421,#17422,#17423,#17424));
#4219=EDGE_LOOP('',(#17425,#17426,#17427));
#4220=EDGE_LOOP('',(#17428,#17429,#17430,#17431));
#4221=EDGE_LOOP('',(#17432,#17433,#17434));
#4222=EDGE_LOOP('',(#17435,#17436,#17437,#17438));
#4223=EDGE_LOOP('',(#17439,#17440,#17441));
#4224=EDGE_LOOP('',(#17442,#17443,#17444,#17445));
#4225=EDGE_LOOP('',(#17446,#17447,#17448));
#4226=EDGE_LOOP('',(#17449,#17450,#17451,#17452));
#4227=EDGE_LOOP('',(#17453,#17454,#17455));
#4228=EDGE_LOOP('',(#17456,#17457,#17458,#17459));
#4229=EDGE_LOOP('',(#17460,#17461,#17462));
#4230=EDGE_LOOP('',(#17463,#17464,#17465,#17466));
#4231=EDGE_LOOP('',(#17467,#17468,#17469));
#4232=EDGE_LOOP('',(#17470,#17471,#17472,#17473));
#4233=EDGE_LOOP('',(#17474,#17475,#17476));
#4234=EDGE_LOOP('',(#17477,#17478,#17479,#17480));
#4235=EDGE_LOOP('',(#17481,#17482,#17483));
#4236=EDGE_LOOP('',(#17484,#17485,#17486,#17487));
#4237=EDGE_LOOP('',(#17488,#17489,#17490));
#4238=EDGE_LOOP('',(#17491,#17492,#17493,#17494));
#4239=EDGE_LOOP('',(#17495,#17496,#17497));
#4240=EDGE_LOOP('',(#17498,#17499,#17500,#17501));
#4241=EDGE_LOOP('',(#17502,#17503,#17504));
#4242=EDGE_LOOP('',(#17505,#17506,#17507,#17508));
#4243=EDGE_LOOP('',(#17509,#17510,#17511,#17512));
#4244=EDGE_LOOP('',(#17513));
#4245=EDGE_LOOP('',(#17514));
#4246=EDGE_LOOP('',(#17515));
#4247=EDGE_LOOP('',(#17516));
#4248=EDGE_LOOP('',(#17517));
#4249=EDGE_LOOP('',(#17518,#17519,#17520,#17521));
#4250=EDGE_LOOP('',(#17522,#17523,#17524,#17525));
#4251=EDGE_LOOP('',(#17526));
#4252=EDGE_LOOP('',(#17527));
#4253=EDGE_LOOP('',(#17528,#17529,#17530,#17531,#17532,#17533,#17534,#17535,
#17536,#17537,#17538,#17539));
#4254=EDGE_LOOP('',(#17540,#17541,#17542,#17543));
#4255=EDGE_LOOP('',(#17544,#17545,#17546,#17547));
#4256=EDGE_LOOP('',(#17548,#17549,#17550,#17551));
#4257=EDGE_LOOP('',(#17552,#17553,#17554,#17555));
#4258=EDGE_LOOP('',(#17556,#17557,#17558,#17559));
#4259=EDGE_LOOP('',(#17560,#17561,#17562,#17563));
#4260=EDGE_LOOP('',(#17564,#17565,#17566,#17567));
#4261=EDGE_LOOP('',(#17568,#17569,#17570,#17571));
#4262=EDGE_LOOP('',(#17572,#17573,#17574,#17575));
#4263=EDGE_LOOP('',(#17576,#17577,#17578,#17579));
#4264=EDGE_LOOP('',(#17580,#17581,#17582,#17583));
#4265=EDGE_LOOP('',(#17584,#17585,#17586,#17587));
#4266=EDGE_LOOP('',(#17588,#17589,#17590,#17591));
#4267=EDGE_LOOP('',(#17592,#17593,#17594,#17595));
#4268=EDGE_LOOP('',(#17596,#17597,#17598,#17599));
#4269=EDGE_LOOP('',(#17600,#17601,#17602,#17603));
#4270=EDGE_LOOP('',(#17604,#17605,#17606,#17607));
#4271=EDGE_LOOP('',(#17608));
#4272=EDGE_LOOP('',(#17609));
#4273=EDGE_LOOP('',(#17610,#17611,#17612,#17613));
#4274=EDGE_LOOP('',(#17614));
#4275=EDGE_LOOP('',(#17615,#17616,#17617,#17618));
#4276=EDGE_LOOP('',(#17619));
#4277=EDGE_LOOP('',(#17620));
#4278=EDGE_LOOP('',(#17621,#17622,#17623,#17624));
#4279=EDGE_LOOP('',(#17625));
#4280=EDGE_LOOP('',(#17626));
#4281=EDGE_LOOP('',(#17627,#17628,#17629,#17630));
#4282=EDGE_LOOP('',(#17631,#17632,#17633,#17634,#17635));
#4283=EDGE_LOOP('',(#17636,#17637,#17638,#17639,#17640,#17641));
#4284=EDGE_LOOP('',(#17642));
#4285=EDGE_LOOP('',(#17643,#17644,#17645,#17646,#17647));
#4286=EDGE_LOOP('',(#17648,#17649,#17650,#17651,#17652,#17653,#17654,#17655));
#4287=EDGE_LOOP('',(#17656));
#4288=EDGE_LOOP('',(#17657,#17658,#17659,#17660));
#4289=EDGE_LOOP('',(#17661,#17662,#17663,#17664));
#4290=EDGE_LOOP('',(#17665,#17666,#17667,#17668));
#4291=EDGE_LOOP('',(#17669,#17670,#17671,#17672));
#4292=EDGE_LOOP('',(#17673,#17674,#17675,#17676));
#4293=EDGE_LOOP('',(#17677,#17678,#17679,#17680));
#4294=EDGE_LOOP('',(#17681,#17682,#17683,#17684));
#4295=EDGE_LOOP('',(#17685,#17686,#17687,#17688));
#4296=EDGE_LOOP('',(#17689,#17690,#17691,#17692));
#4297=EDGE_LOOP('',(#17693,#17694,#17695,#17696));
#4298=EDGE_LOOP('',(#17697,#17698,#17699,#17700));
#4299=EDGE_LOOP('',(#17701,#17702,#17703,#17704));
#4300=EDGE_LOOP('',(#17705,#17706,#17707,#17708,#17709,#17710));
#4301=EDGE_LOOP('',(#17711,#17712,#17713,#17714,#17715,#17716));
#4302=EDGE_LOOP('',(#17717,#17718,#17719,#17720,#17721,#17722));
#4303=EDGE_LOOP('',(#17723,#17724,#17725,#17726));
#4304=EDGE_LOOP('',(#17727,#17728,#17729,#17730));
#4305=EDGE_LOOP('',(#17731,#17732,#17733,#17734));
#4306=EDGE_LOOP('',(#17735,#17736,#17737,#17738));
#4307=EDGE_LOOP('',(#17739,#17740,#17741,#17742));
#4308=EDGE_LOOP('',(#17743,#17744,#17745,#17746));
#4309=EDGE_LOOP('',(#17747,#17748,#17749,#17750));
#4310=EDGE_LOOP('',(#17751,#17752,#17753,#17754));
#4311=EDGE_LOOP('',(#17755,#17756,#17757,#17758));
#4312=EDGE_LOOP('',(#17759,#17760,#17761,#17762));
#4313=EDGE_LOOP('',(#17763,#17764,#17765,#17766,#17767,#17768));
#4314=EDGE_LOOP('',(#17769,#17770,#17771,#17772));
#4315=EDGE_LOOP('',(#17773,#17774,#17775,#17776));
#4316=EDGE_LOOP('',(#17777,#17778,#17779,#17780));
#4317=EDGE_LOOP('',(#17781,#17782,#17783,#17784));
#4318=EDGE_LOOP('',(#17785,#17786,#17787,#17788));
#4319=EDGE_LOOP('',(#17789,#17790,#17791,#17792));
#4320=EDGE_LOOP('',(#17793,#17794,#17795,#17796));
#4321=EDGE_LOOP('',(#17797,#17798,#17799,#17800,#17801,#17802,#17803,#17804));
#4322=EDGE_LOOP('',(#17805,#17806,#17807,#17808));
#4323=EDGE_LOOP('',(#17809,#17810,#17811,#17812));
#4324=EDGE_LOOP('',(#17813,#17814,#17815,#17816));
#4325=EDGE_LOOP('',(#17817,#17818,#17819,#17820));
#4326=EDGE_LOOP('',(#17821,#17822,#17823,#17824));
#4327=EDGE_LOOP('',(#17825,#17826,#17827,#17828));
#4328=EDGE_LOOP('',(#17829,#17830,#17831,#17832));
#4329=EDGE_LOOP('',(#17833,#17834,#17835,#17836));
#4330=EDGE_LOOP('',(#17837,#17838,#17839,#17840));
#4331=EDGE_LOOP('',(#17841,#17842,#17843,#17844));
#4332=EDGE_LOOP('',(#17845,#17846,#17847,#17848));
#4333=EDGE_LOOP('',(#17849,#17850,#17851,#17852));
#4334=EDGE_LOOP('',(#17853,#17854,#17855,#17856));
#4335=EDGE_LOOP('',(#17857,#17858,#17859,#17860));
#4336=EDGE_LOOP('',(#17861,#17862,#17863,#17864));
#4337=EDGE_LOOP('',(#17865,#17866,#17867,#17868));
#4338=EDGE_LOOP('',(#17869,#17870,#17871,#17872));
#4339=EDGE_LOOP('',(#17873,#17874,#17875,#17876));
#4340=EDGE_LOOP('',(#17877,#17878,#17879,#17880));
#4341=EDGE_LOOP('',(#17881,#17882,#17883,#17884));
#4342=EDGE_LOOP('',(#17885,#17886,#17887,#17888));
#4343=EDGE_LOOP('',(#17889,#17890,#17891,#17892));
#4344=EDGE_LOOP('',(#17893,#17894,#17895,#17896));
#4345=EDGE_LOOP('',(#17897,#17898,#17899,#17900));
#4346=EDGE_LOOP('',(#17901,#17902,#17903,#17904));
#4347=EDGE_LOOP('',(#17905,#17906,#17907,#17908));
#4348=EDGE_LOOP('',(#17909,#17910,#17911,#17912));
#4349=EDGE_LOOP('',(#17913,#17914,#17915,#17916,#17917));
#4350=EDGE_LOOP('',(#17918,#17919,#17920,#17921,#17922,#17923,#17924,#17925,
#17926,#17927,#17928,#17929,#17930,#17931,#17932,#17933,#17934,#17935,#17936,
#17937,#17938,#17939,#17940,#17941,#17942,#17943,#17944,#17945,#17946,#17947,
#17948,#17949,#17950));
#4351=EDGE_LOOP('',(#17951,#17952,#17953,#17954,#17955,#17956));
#4352=EDGE_LOOP('',(#17957,#17958,#17959));
#4353=EDGE_LOOP('',(#17960,#17961,#17962,#17963,#17964,#17965,#17966,#17967,
#17968,#17969,#17970,#17971,#17972,#17973,#17974,#17975,#17976,#17977,#17978,
#17979,#17980,#17981,#17982,#17983,#17984,#17985,#17986,#17987,#17988,#17989,
#17990,#17991));
#4354=EDGE_LOOP('',(#17992,#17993,#17994,#17995));
#4355=EDGE_LOOP('',(#17996,#17997,#17998));
#4356=EDGE_LOOP('',(#17999,#18000,#18001,#18002));
#4357=EDGE_LOOP('',(#18003,#18004,#18005));
#4358=EDGE_LOOP('',(#18006,#18007,#18008,#18009));
#4359=EDGE_LOOP('',(#18010,#18011,#18012));
#4360=EDGE_LOOP('',(#18013,#18014,#18015,#18016));
#4361=EDGE_LOOP('',(#18017,#18018,#18019));
#4362=EDGE_LOOP('',(#18020,#18021,#18022,#18023));
#4363=EDGE_LOOP('',(#18024,#18025,#18026));
#4364=EDGE_LOOP('',(#18027,#18028,#18029,#18030));
#4365=EDGE_LOOP('',(#18031,#18032,#18033));
#4366=EDGE_LOOP('',(#18034,#18035,#18036,#18037));
#4367=EDGE_LOOP('',(#18038,#18039,#18040));
#4368=EDGE_LOOP('',(#18041,#18042,#18043,#18044));
#4369=EDGE_LOOP('',(#18045,#18046,#18047));
#4370=EDGE_LOOP('',(#18048,#18049,#18050,#18051));
#4371=EDGE_LOOP('',(#18052,#18053,#18054));
#4372=EDGE_LOOP('',(#18055,#18056,#18057,#18058));
#4373=EDGE_LOOP('',(#18059,#18060,#18061));
#4374=EDGE_LOOP('',(#18062,#18063,#18064,#18065));
#4375=EDGE_LOOP('',(#18066,#18067,#18068));
#4376=EDGE_LOOP('',(#18069,#18070,#18071,#18072));
#4377=EDGE_LOOP('',(#18073,#18074,#18075));
#4378=EDGE_LOOP('',(#18076,#18077,#18078,#18079));
#4379=EDGE_LOOP('',(#18080,#18081,#18082));
#4380=EDGE_LOOP('',(#18083,#18084,#18085,#18086));
#4381=EDGE_LOOP('',(#18087,#18088,#18089));
#4382=EDGE_LOOP('',(#18090,#18091,#18092,#18093));
#4383=EDGE_LOOP('',(#18094,#18095,#18096));
#4384=EDGE_LOOP('',(#18097,#18098,#18099,#18100));
#4385=EDGE_LOOP('',(#18101,#18102,#18103));
#4386=EDGE_LOOP('',(#18104,#18105,#18106,#18107));
#4387=EDGE_LOOP('',(#18108,#18109,#18110));
#4388=EDGE_LOOP('',(#18111,#18112,#18113,#18114));
#4389=EDGE_LOOP('',(#18115,#18116,#18117));
#4390=EDGE_LOOP('',(#18118,#18119,#18120,#18121));
#4391=EDGE_LOOP('',(#18122,#18123,#18124));
#4392=EDGE_LOOP('',(#18125,#18126,#18127,#18128));
#4393=EDGE_LOOP('',(#18129,#18130,#18131));
#4394=EDGE_LOOP('',(#18132,#18133,#18134,#18135));
#4395=EDGE_LOOP('',(#18136,#18137,#18138));
#4396=EDGE_LOOP('',(#18139,#18140,#18141,#18142));
#4397=EDGE_LOOP('',(#18143,#18144,#18145));
#4398=EDGE_LOOP('',(#18146,#18147,#18148,#18149));
#4399=EDGE_LOOP('',(#18150,#18151,#18152));
#4400=EDGE_LOOP('',(#18153,#18154,#18155,#18156));
#4401=EDGE_LOOP('',(#18157,#18158,#18159,#18160));
#4402=EDGE_LOOP('',(#18161,#18162,#18163,#18164));
#4403=EDGE_LOOP('',(#18165,#18166,#18167,#18168));
#4404=EDGE_LOOP('',(#18169,#18170,#18171,#18172));
#4405=EDGE_LOOP('',(#18173,#18174,#18175));
#4406=EDGE_LOOP('',(#18176,#18177,#18178,#18179));
#4407=EDGE_LOOP('',(#18180,#18181,#18182));
#4408=EDGE_LOOP('',(#18183,#18184,#18185,#18186));
#4409=EDGE_LOOP('',(#18187,#18188,#18189));
#4410=EDGE_LOOP('',(#18190,#18191,#18192,#18193));
#4411=EDGE_LOOP('',(#18194,#18195,#18196));
#4412=EDGE_LOOP('',(#18197,#18198,#18199,#18200));
#4413=EDGE_LOOP('',(#18201,#18202,#18203));
#4414=EDGE_LOOP('',(#18204,#18205,#18206,#18207));
#4415=EDGE_LOOP('',(#18208,#18209,#18210));
#4416=EDGE_LOOP('',(#18211,#18212,#18213,#18214));
#4417=EDGE_LOOP('',(#18215,#18216,#18217));
#4418=EDGE_LOOP('',(#18218,#18219,#18220,#18221));
#4419=EDGE_LOOP('',(#18222,#18223,#18224));
#4420=EDGE_LOOP('',(#18225,#18226,#18227,#18228));
#4421=EDGE_LOOP('',(#18229,#18230,#18231));
#4422=EDGE_LOOP('',(#18232,#18233,#18234,#18235));
#4423=EDGE_LOOP('',(#18236,#18237,#18238));
#4424=EDGE_LOOP('',(#18239,#18240,#18241,#18242));
#4425=EDGE_LOOP('',(#18243,#18244,#18245));
#4426=EDGE_LOOP('',(#18246,#18247,#18248,#18249));
#4427=EDGE_LOOP('',(#18250,#18251,#18252));
#4428=EDGE_LOOP('',(#18253,#18254,#18255,#18256));
#4429=EDGE_LOOP('',(#18257,#18258,#18259));
#4430=EDGE_LOOP('',(#18260,#18261,#18262,#18263));
#4431=EDGE_LOOP('',(#18264,#18265,#18266));
#4432=EDGE_LOOP('',(#18267,#18268,#18269,#18270));
#4433=EDGE_LOOP('',(#18271,#18272,#18273));
#4434=EDGE_LOOP('',(#18274,#18275,#18276,#18277));
#4435=EDGE_LOOP('',(#18278,#18279,#18280));
#4436=EDGE_LOOP('',(#18281,#18282,#18283,#18284));
#4437=EDGE_LOOP('',(#18285,#18286,#18287));
#4438=EDGE_LOOP('',(#18288,#18289,#18290,#18291));
#4439=EDGE_LOOP('',(#18292,#18293,#18294));
#4440=EDGE_LOOP('',(#18295,#18296,#18297,#18298));
#4441=EDGE_LOOP('',(#18299,#18300,#18301));
#4442=EDGE_LOOP('',(#18302,#18303,#18304,#18305));
#4443=EDGE_LOOP('',(#18306,#18307,#18308));
#4444=EDGE_LOOP('',(#18309,#18310,#18311,#18312));
#4445=EDGE_LOOP('',(#18313,#18314,#18315));
#4446=EDGE_LOOP('',(#18316,#18317,#18318,#18319));
#4447=EDGE_LOOP('',(#18320,#18321,#18322));
#4448=EDGE_LOOP('',(#18323,#18324,#18325,#18326));
#4449=EDGE_LOOP('',(#18327,#18328,#18329));
#4450=EDGE_LOOP('',(#18330,#18331,#18332,#18333));
#4451=EDGE_LOOP('',(#18334,#18335,#18336));
#4452=EDGE_LOOP('',(#18337));
#4453=EDGE_LOOP('',(#18338,#18339,#18340,#18341));
#4454=EDGE_LOOP('',(#18342));
#4455=EDGE_LOOP('',(#18343,#18344,#18345,#18346));
#4456=EDGE_LOOP('',(#18347,#18348,#18349,#18350));
#4457=EDGE_LOOP('',(#18351,#18352,#18353,#18354,#18355,#18356,#18357,#18358,
#18359,#18360,#18361,#18362));
#4458=EDGE_LOOP('',(#18363,#18364,#18365,#18366));
#4459=EDGE_LOOP('',(#18367,#18368,#18369,#18370));
#4460=EDGE_LOOP('',(#18371,#18372,#18373,#18374));
#4461=EDGE_LOOP('',(#18375,#18376,#18377,#18378));
#4462=EDGE_LOOP('',(#18379,#18380,#18381,#18382));
#4463=EDGE_LOOP('',(#18383,#18384,#18385,#18386));
#4464=EDGE_LOOP('',(#18387,#18388,#18389,#18390));
#4465=EDGE_LOOP('',(#18391,#18392,#18393,#18394));
#4466=EDGE_LOOP('',(#18395,#18396,#18397,#18398));
#4467=EDGE_LOOP('',(#18399,#18400,#18401,#18402));
#4468=EDGE_LOOP('',(#18403,#18404,#18405,#18406));
#4469=EDGE_LOOP('',(#18407,#18408,#18409,#18410));
#4470=EDGE_LOOP('',(#18411,#18412,#18413,#18414));
#4471=EDGE_LOOP('',(#18415,#18416,#18417,#18418));
#4472=EDGE_LOOP('',(#18419,#18420,#18421,#18422));
#4473=EDGE_LOOP('',(#18423,#18424,#18425,#18426));
#4474=EDGE_LOOP('',(#18427,#18428,#18429,#18430));
#4475=EDGE_LOOP('',(#18431,#18432,#18433,#18434));
#4476=EDGE_LOOP('',(#18435,#18436,#18437,#18438));
#4477=EDGE_LOOP('',(#18439,#18440,#18441,#18442));
#4478=EDGE_LOOP('',(#18443,#18444,#18445,#18446));
#4479=EDGE_LOOP('',(#18447,#18448,#18449,#18450));
#4480=EDGE_LOOP('',(#18451,#18452,#18453,#18454));
#4481=EDGE_LOOP('',(#18455,#18456,#18457,#18458));
#4482=EDGE_LOOP('',(#18459));
#4483=EDGE_LOOP('',(#18460));
#4484=EDGE_LOOP('',(#18461,#18462,#18463,#18464,#18465,#18466,#18467,#18468));
#4485=EDGE_LOOP('',(#18469,#18470,#18471,#18472));
#4486=EDGE_LOOP('',(#18473,#18474,#18475,#18476));
#4487=EDGE_LOOP('',(#18477,#18478,#18479,#18480));
#4488=EDGE_LOOP('',(#18481,#18482,#18483,#18484));
#4489=EDGE_LOOP('',(#18485,#18486,#18487,#18488));
#4490=EDGE_LOOP('',(#18489,#18490,#18491,#18492));
#4491=EDGE_LOOP('',(#18493,#18494,#18495,#18496));
#4492=EDGE_LOOP('',(#18497,#18498,#18499,#18500));
#4493=EDGE_LOOP('',(#18501,#18502,#18503,#18504));
#4494=EDGE_LOOP('',(#18505,#18506,#18507,#18508));
#4495=EDGE_LOOP('',(#18509,#18510,#18511,#18512));
#4496=EDGE_LOOP('',(#18513,#18514,#18515,#18516));
#4497=EDGE_LOOP('',(#18517,#18518,#18519,#18520));
#4498=EDGE_LOOP('',(#18521,#18522,#18523,#18524));
#4499=EDGE_LOOP('',(#18525,#18526,#18527,#18528));
#4500=EDGE_LOOP('',(#18529,#18530,#18531,#18532));
#4501=EDGE_LOOP('',(#18533,#18534,#18535,#18536));
#4502=EDGE_LOOP('',(#18537,#18538,#18539,#18540));
#4503=EDGE_LOOP('',(#18541,#18542,#18543,#18544));
#4504=EDGE_LOOP('',(#18545,#18546,#18547,#18548));
#4505=EDGE_LOOP('',(#18549,#18550,#18551,#18552));
#4506=EDGE_LOOP('',(#18553,#18554,#18555,#18556));
#4507=EDGE_LOOP('',(#18557,#18558,#18559,#18560));
#4508=EDGE_LOOP('',(#18561,#18562,#18563,#18564));
#4509=EDGE_LOOP('',(#18565,#18566,#18567,#18568));
#4510=EDGE_LOOP('',(#18569,#18570,#18571,#18572));
#4511=EDGE_LOOP('',(#18573,#18574,#18575,#18576));
#4512=EDGE_LOOP('',(#18577,#18578,#18579,#18580));
#4513=EDGE_LOOP('',(#18581,#18582,#18583,#18584,#18585));
#4514=EDGE_LOOP('',(#18586,#18587,#18588,#18589,#18590,#18591,#18592,#18593,
#18594,#18595,#18596,#18597,#18598,#18599,#18600,#18601,#18602,#18603,#18604,
#18605,#18606,#18607,#18608,#18609,#18610,#18611,#18612,#18613,#18614,#18615,
#18616,#18617,#18618));
#4515=EDGE_LOOP('',(#18619,#18620,#18621,#18622,#18623));
#4516=EDGE_LOOP('',(#18624,#18625,#18626,#18627));
#4517=EDGE_LOOP('',(#18628,#18629,#18630,#18631,#18632,#18633,#18634,#18635,
#18636,#18637,#18638,#18639,#18640,#18641,#18642,#18643,#18644,#18645,#18646,
#18647,#18648,#18649,#18650,#18651,#18652,#18653,#18654,#18655,#18656,#18657,
#18658,#18659,#18660));
#4518=EDGE_LOOP('',(#18661,#18662,#18663));
#4519=EDGE_LOOP('',(#18664,#18665,#18666,#18667));
#4520=EDGE_LOOP('',(#18668,#18669,#18670,#18671));
#4521=EDGE_LOOP('',(#18672,#18673,#18674));
#4522=EDGE_LOOP('',(#18675,#18676,#18677,#18678));
#4523=EDGE_LOOP('',(#18679,#18680,#18681,#18682));
#4524=EDGE_LOOP('',(#18683,#18684,#18685));
#4525=EDGE_LOOP('',(#18686,#18687,#18688,#18689));
#4526=EDGE_LOOP('',(#18690,#18691,#18692,#18693));
#4527=EDGE_LOOP('',(#18694,#18695,#18696));
#4528=EDGE_LOOP('',(#18697,#18698,#18699,#18700));
#4529=EDGE_LOOP('',(#18701,#18702,#18703,#18704));
#4530=EDGE_LOOP('',(#18705,#18706,#18707));
#4531=EDGE_LOOP('',(#18708,#18709,#18710,#18711));
#4532=EDGE_LOOP('',(#18712,#18713,#18714,#18715));
#4533=EDGE_LOOP('',(#18716,#18717,#18718));
#4534=EDGE_LOOP('',(#18719,#18720,#18721,#18722));
#4535=EDGE_LOOP('',(#18723,#18724,#18725,#18726));
#4536=EDGE_LOOP('',(#18727,#18728,#18729));
#4537=EDGE_LOOP('',(#18730,#18731,#18732,#18733));
#4538=EDGE_LOOP('',(#18734,#18735,#18736,#18737));
#4539=EDGE_LOOP('',(#18738,#18739,#18740));
#4540=EDGE_LOOP('',(#18741,#18742,#18743,#18744));
#4541=EDGE_LOOP('',(#18745,#18746,#18747,#18748));
#4542=EDGE_LOOP('',(#18749,#18750,#18751));
#4543=EDGE_LOOP('',(#18752,#18753,#18754,#18755));
#4544=EDGE_LOOP('',(#18756,#18757,#18758,#18759));
#4545=EDGE_LOOP('',(#18760,#18761,#18762));
#4546=EDGE_LOOP('',(#18763,#18764,#18765,#18766));
#4547=EDGE_LOOP('',(#18767,#18768,#18769,#18770));
#4548=EDGE_LOOP('',(#18771,#18772,#18773));
#4549=EDGE_LOOP('',(#18774,#18775,#18776,#18777));
#4550=EDGE_LOOP('',(#18778,#18779,#18780,#18781));
#4551=EDGE_LOOP('',(#18782,#18783,#18784));
#4552=EDGE_LOOP('',(#18785,#18786,#18787,#18788));
#4553=EDGE_LOOP('',(#18789,#18790,#18791,#18792));
#4554=EDGE_LOOP('',(#18793,#18794,#18795));
#4555=EDGE_LOOP('',(#18796,#18797,#18798,#18799));
#4556=EDGE_LOOP('',(#18800,#18801,#18802,#18803));
#4557=EDGE_LOOP('',(#18804,#18805,#18806));
#4558=EDGE_LOOP('',(#18807,#18808,#18809,#18810));
#4559=EDGE_LOOP('',(#18811,#18812,#18813,#18814));
#4560=EDGE_LOOP('',(#18815,#18816,#18817));
#4561=EDGE_LOOP('',(#18818,#18819,#18820,#18821));
#4562=EDGE_LOOP('',(#18822,#18823,#18824,#18825));
#4563=EDGE_LOOP('',(#18826,#18827,#18828));
#4564=EDGE_LOOP('',(#18829,#18830,#18831,#18832));
#4565=EDGE_LOOP('',(#18833,#18834,#18835,#18836));
#4566=EDGE_LOOP('',(#18837,#18838,#18839));
#4567=EDGE_LOOP('',(#18840,#18841,#18842,#18843));
#4568=EDGE_LOOP('',(#18844,#18845,#18846,#18847));
#4569=EDGE_LOOP('',(#18848,#18849,#18850,#18851));
#4570=EDGE_LOOP('',(#18852,#18853,#18854,#18855));
#4571=EDGE_LOOP('',(#18856,#18857,#18858,#18859));
#4572=EDGE_LOOP('',(#18860,#18861,#18862));
#4573=EDGE_LOOP('',(#18863,#18864,#18865,#18866));
#4574=EDGE_LOOP('',(#18867,#18868,#18869,#18870));
#4575=EDGE_LOOP('',(#18871,#18872,#18873));
#4576=EDGE_LOOP('',(#18874,#18875,#18876,#18877));
#4577=EDGE_LOOP('',(#18878,#18879,#18880,#18881));
#4578=EDGE_LOOP('',(#18882,#18883,#18884));
#4579=EDGE_LOOP('',(#18885,#18886,#18887,#18888));
#4580=EDGE_LOOP('',(#18889,#18890,#18891,#18892));
#4581=EDGE_LOOP('',(#18893,#18894,#18895));
#4582=EDGE_LOOP('',(#18896,#18897,#18898,#18899));
#4583=EDGE_LOOP('',(#18900,#18901,#18902,#18903));
#4584=EDGE_LOOP('',(#18904,#18905,#18906));
#4585=EDGE_LOOP('',(#18907,#18908,#18909,#18910));
#4586=EDGE_LOOP('',(#18911,#18912,#18913,#18914));
#4587=EDGE_LOOP('',(#18915,#18916,#18917));
#4588=EDGE_LOOP('',(#18918,#18919,#18920,#18921));
#4589=EDGE_LOOP('',(#18922,#18923,#18924,#18925));
#4590=EDGE_LOOP('',(#18926,#18927,#18928));
#4591=EDGE_LOOP('',(#18929,#18930,#18931,#18932));
#4592=EDGE_LOOP('',(#18933,#18934,#18935,#18936));
#4593=EDGE_LOOP('',(#18937,#18938,#18939));
#4594=EDGE_LOOP('',(#18940,#18941,#18942,#18943));
#4595=EDGE_LOOP('',(#18944,#18945,#18946,#18947));
#4596=EDGE_LOOP('',(#18948,#18949,#18950));
#4597=EDGE_LOOP('',(#18951,#18952,#18953,#18954));
#4598=EDGE_LOOP('',(#18955,#18956,#18957,#18958));
#4599=EDGE_LOOP('',(#18959,#18960,#18961));
#4600=EDGE_LOOP('',(#18962,#18963,#18964,#18965));
#4601=EDGE_LOOP('',(#18966,#18967,#18968,#18969));
#4602=EDGE_LOOP('',(#18970,#18971,#18972));
#4603=EDGE_LOOP('',(#18973,#18974,#18975,#18976));
#4604=EDGE_LOOP('',(#18977,#18978,#18979,#18980));
#4605=EDGE_LOOP('',(#18981,#18982,#18983));
#4606=EDGE_LOOP('',(#18984,#18985,#18986,#18987));
#4607=EDGE_LOOP('',(#18988,#18989,#18990,#18991));
#4608=EDGE_LOOP('',(#18992,#18993,#18994));
#4609=EDGE_LOOP('',(#18995,#18996,#18997,#18998));
#4610=EDGE_LOOP('',(#18999,#19000,#19001,#19002));
#4611=EDGE_LOOP('',(#19003,#19004,#19005));
#4612=EDGE_LOOP('',(#19006,#19007,#19008,#19009));
#4613=EDGE_LOOP('',(#19010,#19011,#19012,#19013));
#4614=EDGE_LOOP('',(#19014,#19015,#19016));
#4615=EDGE_LOOP('',(#19017,#19018,#19019,#19020));
#4616=EDGE_LOOP('',(#19021,#19022,#19023,#19024));
#4617=EDGE_LOOP('',(#19025,#19026,#19027));
#4618=EDGE_LOOP('',(#19028,#19029,#19030,#19031));
#4619=EDGE_LOOP('',(#19032,#19033,#19034,#19035));
#4620=EDGE_LOOP('',(#19036,#19037,#19038));
#4621=EDGE_LOOP('',(#19039,#19040,#19041,#19042));
#4622=EDGE_LOOP('',(#19043,#19044,#19045,#19046));
#4623=EDGE_LOOP('',(#19047,#19048,#19049,#19050,#19051,#19052,#19053,#19054,
#19055,#19056,#19057,#19058,#19059,#19060,#19061,#19062,#19063,#19064,#19065,
#19066,#19067,#19068,#19069,#19070,#19071,#19072,#19073,#19074,#19075,#19076,
#19077,#19078,#19079,#19080,#19081,#19082,#19083,#19084,#19085,#19086,#19087,
#19088,#19089,#19090,#19091,#19092,#19093,#19094,#19095,#19096,#19097,#19098,
#19099,#19100,#19101,#19102,#19103,#19104,#19105,#19106,#19107,#19108,#19109,
#19110,#19111,#19112,#19113,#19114,#19115,#19116,#19117,#19118,#19119,#19120,
#19121,#19122,#19123,#19124,#19125,#19126,#19127,#19128,#19129,#19130,#19131,
#19132,#19133,#19134,#19135,#19136,#19137,#19138,#19139,#19140,#19141,#19142,
#19143,#19144,#19145,#19146,#19147,#19148,#19149,#19150,#19151,#19152,#19153,
#19154,#19155,#19156,#19157,#19158,#19159,#19160,#19161,#19162,#19163,#19164,
#19165,#19166,#19167,#19168,#19169,#19170,#19171,#19172,#19173,#19174,#19175,
#19176,#19177,#19178,#19179,#19180,#19181,#19182,#19183,#19184,#19185,#19186,
#19187,#19188,#19189,#19190,#19191,#19192,#19193,#19194));
#4624=EDGE_LOOP('',(#19195,#19196,#19197,#19198));
#4625=EDGE_LOOP('',(#19199,#19200,#19201,#19202));
#4626=EDGE_LOOP('',(#19203,#19204,#19205));
#4627=EDGE_LOOP('',(#19206,#19207,#19208,#19209,#19210,#19211,#19212,#19213,
#19214,#19215,#19216,#19217,#19218,#19219,#19220,#19221,#19222,#19223,#19224,
#19225,#19226,#19227,#19228,#19229,#19230,#19231,#19232,#19233,#19234,#19235,
#19236,#19237,#19238,#19239,#19240,#19241,#19242,#19243,#19244,#19245,#19246,
#19247,#19248,#19249,#19250,#19251,#19252,#19253,#19254,#19255,#19256,#19257,
#19258,#19259,#19260,#19261,#19262,#19263,#19264,#19265,#19266,#19267,#19268,
#19269,#19270,#19271,#19272,#19273,#19274,#19275,#19276,#19277,#19278,#19279,
#19280,#19281,#19282,#19283,#19284,#19285,#19286,#19287,#19288,#19289,#19290,
#19291,#19292,#19293,#19294,#19295,#19296,#19297,#19298,#19299,#19300,#19301,
#19302,#19303,#19304,#19305,#19306,#19307,#19308,#19309,#19310,#19311,#19312,
#19313,#19314,#19315,#19316));
#4628=EDGE_LOOP('',(#19317,#19318,#19319));
#4629=EDGE_LOOP('',(#19320,#19321,#19322,#19323));
#4630=EDGE_LOOP('',(#19324,#19325,#19326,#19327));
#4631=EDGE_LOOP('',(#19328,#19329,#19330,#19331));
#4632=EDGE_LOOP('',(#19332,#19333,#19334,#19335));
#4633=EDGE_LOOP('',(#19336,#19337,#19338,#19339));
#4634=EDGE_LOOP('',(#19340,#19341,#19342,#19343));
#4635=EDGE_LOOP('',(#19344,#19345,#19346,#19347,#19348,#19349));
#4636=EDGE_LOOP('',(#19350));
#4637=EDGE_LOOP('',(#19351));
#4638=EDGE_LOOP('',(#19352,#19353,#19354,#19355));
#4639=EDGE_LOOP('',(#19356,#19357,#19358,#19359));
#4640=EDGE_LOOP('',(#19360,#19361,#19362,#19363,#19364,#19365));
#4641=EDGE_LOOP('',(#19366));
#4642=EDGE_LOOP('',(#19367));
#4643=EDGE_LOOP('',(#19368));
#4644=EDGE_LOOP('',(#19369,#19370,#19371,#19372,#19373,#19374));
#4645=EDGE_LOOP('',(#19375,#19376,#19377,#19378,#19379,#19380,#19381,#19382));
#4646=EDGE_LOOP('',(#19383,#19384,#19385,#19386));
#4647=EDGE_LOOP('',(#19387,#19388,#19389,#19390));
#4648=EDGE_LOOP('',(#19391,#19392,#19393,#19394));
#4649=EDGE_LOOP('',(#19395,#19396,#19397,#19398));
#4650=EDGE_LOOP('',(#19399,#19400,#19401,#19402));
#4651=EDGE_LOOP('',(#19403,#19404,#19405,#19406));
#4652=EDGE_LOOP('',(#19407,#19408,#19409,#19410));
#4653=EDGE_LOOP('',(#19411,#19412,#19413,#19414));
#4654=EDGE_LOOP('',(#19415,#19416,#19417,#19418));
#4655=EDGE_LOOP('',(#19419,#19420,#19421,#19422));
#4656=EDGE_LOOP('',(#19423,#19424,#19425,#19426));
#4657=EDGE_LOOP('',(#19427,#19428,#19429,#19430));
#4658=EDGE_LOOP('',(#19431,#19432,#19433,#19434));
#4659=EDGE_LOOP('',(#19435,#19436,#19437,#19438));
#4660=EDGE_LOOP('',(#19439,#19440,#19441,#19442));
#4661=EDGE_LOOP('',(#19443,#19444,#19445,#19446));
#4662=EDGE_LOOP('',(#19447,#19448,#19449,#19450));
#4663=EDGE_LOOP('',(#19451,#19452,#19453,#19454));
#4664=EDGE_LOOP('',(#19455,#19456,#19457,#19458));
#4665=EDGE_LOOP('',(#19459,#19460,#19461,#19462));
#4666=EDGE_LOOP('',(#19463,#19464,#19465,#19466));
#4667=EDGE_LOOP('',(#19467,#19468,#19469,#19470));
#4668=EDGE_LOOP('',(#19471,#19472,#19473,#19474));
#4669=EDGE_LOOP('',(#19475,#19476,#19477,#19478));
#4670=EDGE_LOOP('',(#19479,#19480,#19481,#19482));
#4671=EDGE_LOOP('',(#19483,#19484,#19485,#19486));
#4672=EDGE_LOOP('',(#19487,#19488,#19489,#19490));
#4673=EDGE_LOOP('',(#19491,#19492,#19493,#19494));
#4674=EDGE_LOOP('',(#19495,#19496,#19497,#19498));
#4675=EDGE_LOOP('',(#19499,#19500,#19501,#19502));
#4676=EDGE_LOOP('',(#19503,#19504,#19505,#19506));
#4677=EDGE_LOOP('',(#19507,#19508,#19509,#19510));
#4678=EDGE_LOOP('',(#19511,#19512,#19513,#19514));
#4679=EDGE_LOOP('',(#19515,#19516,#19517,#19518));
#4680=EDGE_LOOP('',(#19519,#19520,#19521,#19522));
#4681=EDGE_LOOP('',(#19523,#19524,#19525,#19526));
#4682=EDGE_LOOP('',(#19527,#19528,#19529,#19530));
#4683=EDGE_LOOP('',(#19531,#19532,#19533,#19534));
#4684=EDGE_LOOP('',(#19535,#19536,#19537,#19538));
#4685=EDGE_LOOP('',(#19539,#19540,#19541,#19542));
#4686=EDGE_LOOP('',(#19543,#19544,#19545,#19546));
#4687=EDGE_LOOP('',(#19547,#19548,#19549,#19550));
#4688=EDGE_LOOP('',(#19551,#19552,#19553,#19554));
#4689=EDGE_LOOP('',(#19555,#19556,#19557,#19558));
#4690=EDGE_LOOP('',(#19559,#19560,#19561,#19562));
#4691=EDGE_LOOP('',(#19563,#19564,#19565,#19566));
#4692=EDGE_LOOP('',(#19567,#19568,#19569,#19570));
#4693=EDGE_LOOP('',(#19571,#19572,#19573,#19574));
#4694=EDGE_LOOP('',(#19575,#19576,#19577,#19578));
#4695=EDGE_LOOP('',(#19579,#19580,#19581,#19582));
#4696=EDGE_LOOP('',(#19583,#19584,#19585,#19586));
#4697=EDGE_LOOP('',(#19587,#19588,#19589,#19590));
#4698=EDGE_LOOP('',(#19591,#19592,#19593,#19594));
#4699=EDGE_LOOP('',(#19595,#19596,#19597,#19598));
#4700=EDGE_LOOP('',(#19599,#19600,#19601,#19602));
#4701=EDGE_LOOP('',(#19603,#19604,#19605,#19606));
#4702=EDGE_LOOP('',(#19607,#19608,#19609,#19610));
#4703=EDGE_LOOP('',(#19611,#19612,#19613,#19614));
#4704=EDGE_LOOP('',(#19615,#19616,#19617,#19618));
#4705=EDGE_LOOP('',(#19619,#19620,#19621,#19622));
#4706=EDGE_LOOP('',(#19623,#19624,#19625,#19626));
#4707=EDGE_LOOP('',(#19627,#19628,#19629,#19630));
#4708=EDGE_LOOP('',(#19631,#19632,#19633,#19634));
#4709=EDGE_LOOP('',(#19635,#19636,#19637,#19638));
#4710=EDGE_LOOP('',(#19639,#19640,#19641,#19642));
#4711=EDGE_LOOP('',(#19643,#19644,#19645,#19646));
#4712=EDGE_LOOP('',(#19647,#19648,#19649,#19650));
#4713=EDGE_LOOP('',(#19651,#19652,#19653,#19654));
#4714=EDGE_LOOP('',(#19655,#19656,#19657,#19658));
#4715=EDGE_LOOP('',(#19659,#19660,#19661,#19662));
#4716=EDGE_LOOP('',(#19663,#19664,#19665,#19666));
#4717=EDGE_LOOP('',(#19667,#19668,#19669,#19670));
#4718=EDGE_LOOP('',(#19671,#19672,#19673,#19674));
#4719=EDGE_LOOP('',(#19675,#19676,#19677,#19678));
#4720=EDGE_LOOP('',(#19679,#19680,#19681,#19682));
#4721=EDGE_LOOP('',(#19683,#19684,#19685,#19686));
#4722=EDGE_LOOP('',(#19687,#19688,#19689,#19690));
#4723=EDGE_LOOP('',(#19691,#19692,#19693,#19694));
#4724=EDGE_LOOP('',(#19695,#19696,#19697,#19698));
#4725=EDGE_LOOP('',(#19699,#19700,#19701,#19702));
#4726=EDGE_LOOP('',(#19703,#19704,#19705,#19706));
#4727=EDGE_LOOP('',(#19707,#19708,#19709,#19710));
#4728=EDGE_LOOP('',(#19711,#19712,#19713,#19714));
#4729=EDGE_LOOP('',(#19715,#19716,#19717,#19718));
#4730=EDGE_LOOP('',(#19719,#19720,#19721,#19722));
#4731=EDGE_LOOP('',(#19723,#19724,#19725,#19726));
#4732=EDGE_LOOP('',(#19727,#19728,#19729,#19730));
#4733=EDGE_LOOP('',(#19731,#19732,#19733,#19734));
#4734=EDGE_LOOP('',(#19735,#19736,#19737,#19738));
#4735=EDGE_LOOP('',(#19739,#19740,#19741,#19742));
#4736=EDGE_LOOP('',(#19743,#19744,#19745,#19746));
#4737=EDGE_LOOP('',(#19747,#19748,#19749,#19750));
#4738=EDGE_LOOP('',(#19751,#19752,#19753,#19754));
#4739=EDGE_LOOP('',(#19755,#19756,#19757,#19758));
#4740=EDGE_LOOP('',(#19759,#19760,#19761,#19762));
#4741=EDGE_LOOP('',(#19763,#19764,#19765,#19766));
#4742=EDGE_LOOP('',(#19767,#19768,#19769,#19770));
#4743=EDGE_LOOP('',(#19771,#19772,#19773,#19774));
#4744=EDGE_LOOP('',(#19775,#19776,#19777,#19778));
#4745=EDGE_LOOP('',(#19779,#19780,#19781,#19782));
#4746=EDGE_LOOP('',(#19783,#19784,#19785,#19786));
#4747=EDGE_LOOP('',(#19787,#19788,#19789,#19790));
#4748=EDGE_LOOP('',(#19791,#19792,#19793,#19794));
#4749=EDGE_LOOP('',(#19795,#19796,#19797,#19798));
#4750=EDGE_LOOP('',(#19799,#19800,#19801,#19802));
#4751=EDGE_LOOP('',(#19803,#19804,#19805,#19806));
#4752=EDGE_LOOP('',(#19807,#19808,#19809,#19810));
#4753=EDGE_LOOP('',(#19811,#19812,#19813,#19814));
#4754=EDGE_LOOP('',(#19815,#19816,#19817,#19818));
#4755=EDGE_LOOP('',(#19819,#19820,#19821,#19822));
#4756=EDGE_LOOP('',(#19823,#19824,#19825,#19826));
#4757=EDGE_LOOP('',(#19827,#19828,#19829,#19830));
#4758=EDGE_LOOP('',(#19831,#19832,#19833,#19834));
#4759=EDGE_LOOP('',(#19835,#19836,#19837,#19838));
#4760=EDGE_LOOP('',(#19839,#19840,#19841,#19842));
#4761=EDGE_LOOP('',(#19843,#19844,#19845,#19846));
#4762=EDGE_LOOP('',(#19847,#19848,#19849,#19850,#19851));
#4763=EDGE_LOOP('',(#19852,#19853,#19854,#19855,#19856,#19857,#19858,#19859,
#19860,#19861,#19862,#19863,#19864,#19865,#19866,#19867,#19868,#19869,#19870,
#19871,#19872,#19873,#19874,#19875,#19876,#19877,#19878,#19879,#19880,#19881,
#19882,#19883,#19884,#19885,#19886,#19887,#19888,#19889,#19890,#19891,#19892,
#19893,#19894,#19895,#19896,#19897,#19898,#19899,#19900,#19901,#19902,#19903,
#19904,#19905,#19906,#19907,#19908,#19909,#19910,#19911,#19912,#19913,#19914,
#19915,#19916,#19917,#19918,#19919,#19920,#19921,#19922,#19923,#19924,#19925,
#19926,#19927,#19928,#19929,#19930,#19931,#19932,#19933,#19934,#19935,#19936,
#19937,#19938,#19939,#19940,#19941,#19942,#19943,#19944,#19945,#19946,#19947,
#19948,#19949,#19950,#19951,#19952,#19953,#19954,#19955,#19956,#19957,#19958,
#19959,#19960,#19961,#19962,#19963,#19964,#19965,#19966,#19967,#19968,#19969,
#19970,#19971,#19972));
#4764=EDGE_LOOP('',(#19973,#19974,#19975,#19976,#19977));
#4765=EDGE_LOOP('',(#19978,#19979,#19980,#19981));
#4766=EDGE_LOOP('',(#19982,#19983,#19984,#19985,#19986,#19987,#19988,#19989,
#19990,#19991,#19992,#19993,#19994,#19995,#19996,#19997,#19998,#19999,#20000,
#20001,#20002,#20003,#20004,#20005,#20006,#20007,#20008,#20009,#20010,#20011,
#20012,#20013,#20014,#20015,#20016,#20017,#20018,#20019,#20020,#20021,#20022,
#20023,#20024,#20025,#20026,#20027,#20028,#20029,#20030,#20031,#20032,#20033,
#20034,#20035,#20036,#20037,#20038,#20039,#20040,#20041,#20042,#20043,#20044,
#20045,#20046,#20047,#20048,#20049,#20050,#20051,#20052,#20053,#20054,#20055,
#20056,#20057,#20058,#20059,#20060,#20061,#20062,#20063,#20064,#20065,#20066,
#20067,#20068,#20069,#20070,#20071,#20072,#20073,#20074,#20075,#20076,#20077,
#20078,#20079,#20080,#20081,#20082,#20083,#20084,#20085,#20086,#20087,#20088,
#20089,#20090,#20091,#20092,#20093,#20094,#20095,#20096,#20097,#20098,#20099,
#20100,#20101,#20102));
#4767=EDGE_LOOP('',(#20103,#20104,#20105));
#4768=EDGE_LOOP('',(#20106,#20107,#20108,#20109));
#4769=EDGE_LOOP('',(#20110,#20111,#20112,#20113));
#4770=EDGE_LOOP('',(#20114,#20115,#20116));
#4771=EDGE_LOOP('',(#20117,#20118,#20119,#20120));
#4772=EDGE_LOOP('',(#20121,#20122,#20123,#20124));
#4773=EDGE_LOOP('',(#20125,#20126,#20127));
#4774=EDGE_LOOP('',(#20128,#20129,#20130,#20131));
#4775=EDGE_LOOP('',(#20132,#20133,#20134,#20135));
#4776=EDGE_LOOP('',(#20136,#20137,#20138));
#4777=EDGE_LOOP('',(#20139,#20140,#20141,#20142));
#4778=EDGE_LOOP('',(#20143,#20144,#20145,#20146));
#4779=EDGE_LOOP('',(#20147,#20148,#20149));
#4780=EDGE_LOOP('',(#20150,#20151,#20152,#20153));
#4781=EDGE_LOOP('',(#20154,#20155,#20156,#20157));
#4782=EDGE_LOOP('',(#20158,#20159,#20160));
#4783=EDGE_LOOP('',(#20161,#20162,#20163,#20164));
#4784=EDGE_LOOP('',(#20165,#20166,#20167,#20168));
#4785=EDGE_LOOP('',(#20169,#20170,#20171));
#4786=EDGE_LOOP('',(#20172,#20173,#20174,#20175));
#4787=EDGE_LOOP('',(#20176,#20177,#20178,#20179));
#4788=EDGE_LOOP('',(#20180,#20181,#20182));
#4789=EDGE_LOOP('',(#20183,#20184,#20185,#20186));
#4790=EDGE_LOOP('',(#20187,#20188,#20189,#20190));
#4791=EDGE_LOOP('',(#20191,#20192,#20193));
#4792=EDGE_LOOP('',(#20194,#20195,#20196,#20197));
#4793=EDGE_LOOP('',(#20198,#20199,#20200,#20201));
#4794=EDGE_LOOP('',(#20202,#20203,#20204));
#4795=EDGE_LOOP('',(#20205,#20206,#20207,#20208));
#4796=EDGE_LOOP('',(#20209,#20210,#20211,#20212));
#4797=EDGE_LOOP('',(#20213,#20214,#20215));
#4798=EDGE_LOOP('',(#20216,#20217,#20218,#20219));
#4799=EDGE_LOOP('',(#20220,#20221,#20222,#20223));
#4800=EDGE_LOOP('',(#20224,#20225,#20226));
#4801=EDGE_LOOP('',(#20227,#20228,#20229,#20230));
#4802=EDGE_LOOP('',(#20231,#20232,#20233,#20234));
#4803=EDGE_LOOP('',(#20235,#20236,#20237));
#4804=EDGE_LOOP('',(#20238,#20239,#20240,#20241));
#4805=EDGE_LOOP('',(#20242,#20243,#20244,#20245));
#4806=EDGE_LOOP('',(#20246,#20247,#20248));
#4807=EDGE_LOOP('',(#20249,#20250,#20251,#20252));
#4808=EDGE_LOOP('',(#20253,#20254,#20255,#20256));
#4809=EDGE_LOOP('',(#20257,#20258,#20259));
#4810=EDGE_LOOP('',(#20260,#20261,#20262,#20263));
#4811=EDGE_LOOP('',(#20264,#20265,#20266,#20267));
#4812=EDGE_LOOP('',(#20268,#20269,#20270));
#4813=EDGE_LOOP('',(#20271,#20272,#20273,#20274));
#4814=EDGE_LOOP('',(#20275,#20276,#20277,#20278));
#4815=EDGE_LOOP('',(#20279,#20280,#20281));
#4816=EDGE_LOOP('',(#20282,#20283,#20284,#20285));
#4817=EDGE_LOOP('',(#20286,#20287,#20288,#20289));
#4818=EDGE_LOOP('',(#20290,#20291,#20292,#20293));
#4819=EDGE_LOOP('',(#20294,#20295,#20296,#20297));
#4820=EDGE_LOOP('',(#20298,#20299,#20300,#20301));
#4821=EDGE_LOOP('',(#20302,#20303,#20304));
#4822=EDGE_LOOP('',(#20305,#20306,#20307,#20308));
#4823=EDGE_LOOP('',(#20309,#20310,#20311,#20312));
#4824=EDGE_LOOP('',(#20313,#20314,#20315));
#4825=EDGE_LOOP('',(#20316,#20317,#20318,#20319));
#4826=EDGE_LOOP('',(#20320,#20321,#20322,#20323));
#4827=EDGE_LOOP('',(#20324,#20325,#20326));
#4828=EDGE_LOOP('',(#20327,#20328,#20329,#20330));
#4829=EDGE_LOOP('',(#20331,#20332,#20333,#20334));
#4830=EDGE_LOOP('',(#20335,#20336,#20337));
#4831=EDGE_LOOP('',(#20338,#20339,#20340,#20341));
#4832=EDGE_LOOP('',(#20342,#20343,#20344,#20345));
#4833=EDGE_LOOP('',(#20346,#20347,#20348));
#4834=EDGE_LOOP('',(#20349,#20350,#20351,#20352));
#4835=EDGE_LOOP('',(#20353,#20354,#20355,#20356));
#4836=EDGE_LOOP('',(#20357,#20358,#20359));
#4837=EDGE_LOOP('',(#20360,#20361,#20362,#20363));
#4838=EDGE_LOOP('',(#20364,#20365,#20366,#20367));
#4839=EDGE_LOOP('',(#20368,#20369,#20370));
#4840=EDGE_LOOP('',(#20371,#20372,#20373,#20374));
#4841=EDGE_LOOP('',(#20375,#20376,#20377,#20378));
#4842=EDGE_LOOP('',(#20379,#20380,#20381));
#4843=EDGE_LOOP('',(#20382,#20383,#20384,#20385));
#4844=EDGE_LOOP('',(#20386,#20387,#20388,#20389));
#4845=EDGE_LOOP('',(#20390,#20391,#20392));
#4846=EDGE_LOOP('',(#20393,#20394,#20395,#20396));
#4847=EDGE_LOOP('',(#20397,#20398,#20399,#20400));
#4848=EDGE_LOOP('',(#20401,#20402,#20403));
#4849=EDGE_LOOP('',(#20404,#20405,#20406,#20407));
#4850=EDGE_LOOP('',(#20408,#20409,#20410,#20411));
#4851=EDGE_LOOP('',(#20412,#20413,#20414));
#4852=EDGE_LOOP('',(#20415,#20416,#20417,#20418));
#4853=EDGE_LOOP('',(#20419,#20420,#20421,#20422));
#4854=EDGE_LOOP('',(#20423,#20424,#20425));
#4855=EDGE_LOOP('',(#20426,#20427,#20428,#20429));
#4856=EDGE_LOOP('',(#20430,#20431,#20432,#20433));
#4857=EDGE_LOOP('',(#20434,#20435,#20436));
#4858=EDGE_LOOP('',(#20437,#20438,#20439,#20440));
#4859=EDGE_LOOP('',(#20441,#20442,#20443,#20444));
#4860=EDGE_LOOP('',(#20445,#20446,#20447));
#4861=EDGE_LOOP('',(#20448,#20449,#20450,#20451));
#4862=EDGE_LOOP('',(#20452,#20453,#20454,#20455));
#4863=EDGE_LOOP('',(#20456,#20457,#20458));
#4864=EDGE_LOOP('',(#20459,#20460,#20461,#20462));
#4865=EDGE_LOOP('',(#20463,#20464,#20465,#20466));
#4866=EDGE_LOOP('',(#20467,#20468,#20469));
#4867=EDGE_LOOP('',(#20470,#20471,#20472,#20473));
#4868=EDGE_LOOP('',(#20474,#20475,#20476,#20477));
#4869=EDGE_LOOP('',(#20478,#20479,#20480));
#4870=EDGE_LOOP('',(#20481,#20482,#20483,#20484));
#4871=EDGE_LOOP('',(#20485,#20486,#20487,#20488));
#4872=EDGE_LOOP('',(#20489,#20490,#20491,#20492,#20493,#20494,#20495,#20496,
#20497,#20498,#20499,#20500,#20501,#20502,#20503,#20504,#20505,#20506,#20507,
#20508,#20509,#20510,#20511,#20512,#20513,#20514,#20515,#20516,#20517,#20518,
#20519,#20520,#20521,#20522,#20523,#20524,#20525,#20526,#20527,#20528,#20529,
#20530,#20531,#20532,#20533,#20534,#20535,#20536,#20537,#20538,#20539,#20540,
#20541,#20542,#20543,#20544,#20545,#20546,#20547,#20548,#20549,#20550,#20551,
#20552,#20553,#20554,#20555,#20556,#20557,#20558,#20559,#20560,#20561,#20562,
#20563,#20564,#20565,#20566,#20567,#20568,#20569,#20570,#20571,#20572,#20573,
#20574,#20575,#20576,#20577,#20578,#20579,#20580,#20581,#20582,#20583,#20584,
#20585,#20586,#20587,#20588,#20589,#20590,#20591,#20592,#20593,#20594,#20595,
#20596,#20597,#20598,#20599,#20600,#20601,#20602,#20603,#20604,#20605,#20606,
#20607,#20608,#20609,#20610,#20611,#20612,#20613,#20614,#20615,#20616,#20617,
#20618,#20619,#20620,#20621,#20622,#20623,#20624,#20625,#20626,#20627,#20628,
#20629,#20630,#20631,#20632,#20633,#20634,#20635,#20636));
#4873=EDGE_LOOP('',(#20637,#20638,#20639,#20640));
#4874=EDGE_LOOP('',(#20641,#20642,#20643,#20644));
#4875=EDGE_LOOP('',(#20645,#20646,#20647));
#4876=EDGE_LOOP('',(#20648,#20649,#20650,#20651,#20652,#20653,#20654,#20655,
#20656,#20657,#20658,#20659,#20660,#20661,#20662,#20663,#20664,#20665,#20666,
#20667,#20668,#20669,#20670,#20671,#20672,#20673,#20674,#20675,#20676,#20677,
#20678,#20679,#20680,#20681,#20682,#20683,#20684,#20685,#20686,#20687,#20688,
#20689,#20690,#20691,#20692,#20693,#20694,#20695,#20696,#20697,#20698,#20699,
#20700,#20701,#20702,#20703,#20704,#20705,#20706,#20707,#20708,#20709,#20710,
#20711,#20712,#20713,#20714,#20715,#20716,#20717,#20718,#20719,#20720,#20721,
#20722,#20723,#20724,#20725,#20726,#20727,#20728,#20729,#20730,#20731,#20732,
#20733,#20734,#20735,#20736,#20737,#20738,#20739,#20740,#20741,#20742,#20743,
#20744,#20745,#20746,#20747,#20748,#20749,#20750,#20751,#20752,#20753,#20754,
#20755,#20756,#20757,#20758));
#4877=EDGE_LOOP('',(#20759,#20760,#20761));
#4878=EDGE_LOOP('',(#20762,#20763,#20764,#20765));
#4879=EDGE_LOOP('',(#20766,#20767,#20768,#20769));
#4880=EDGE_LOOP('',(#20770,#20771,#20772,#20773));
#4881=EDGE_LOOP('',(#20774,#20775,#20776,#20777));
#4882=EDGE_LOOP('',(#20778,#20779,#20780,#20781));
#4883=EDGE_LOOP('',(#20782,#20783,#20784,#20785));
#4884=EDGE_LOOP('',(#20786,#20787,#20788,#20789,#20790,#20791));
#4885=EDGE_LOOP('',(#20792));
#4886=EDGE_LOOP('',(#20793));
#4887=EDGE_LOOP('',(#20794,#20795,#20796,#20797));
#4888=EDGE_LOOP('',(#20798,#20799,#20800,#20801));
#4889=EDGE_LOOP('',(#20802,#20803,#20804,#20805,#20806,#20807));
#4890=EDGE_LOOP('',(#20808));
#4891=EDGE_LOOP('',(#20809));
#4892=EDGE_LOOP('',(#20810));
#4893=EDGE_LOOP('',(#20811,#20812,#20813,#20814,#20815,#20816));
#4894=EDGE_LOOP('',(#20817,#20818,#20819,#20820,#20821,#20822,#20823,#20824));
#4895=EDGE_LOOP('',(#20825,#20826,#20827,#20828));
#4896=EDGE_LOOP('',(#20829,#20830,#20831,#20832));
#4897=EDGE_LOOP('',(#20833,#20834,#20835,#20836));
#4898=EDGE_LOOP('',(#20837,#20838,#20839,#20840));
#4899=EDGE_LOOP('',(#20841,#20842,#20843,#20844));
#4900=EDGE_LOOP('',(#20845,#20846,#20847,#20848));
#4901=EDGE_LOOP('',(#20849,#20850,#20851,#20852));
#4902=EDGE_LOOP('',(#20853,#20854,#20855,#20856));
#4903=EDGE_LOOP('',(#20857,#20858,#20859,#20860));
#4904=EDGE_LOOP('',(#20861,#20862,#20863,#20864));
#4905=EDGE_LOOP('',(#20865,#20866,#20867,#20868));
#4906=EDGE_LOOP('',(#20869,#20870,#20871,#20872));
#4907=EDGE_LOOP('',(#20873,#20874,#20875,#20876));
#4908=EDGE_LOOP('',(#20877,#20878,#20879,#20880));
#4909=EDGE_LOOP('',(#20881,#20882,#20883,#20884));
#4910=EDGE_LOOP('',(#20885,#20886,#20887,#20888));
#4911=EDGE_LOOP('',(#20889,#20890,#20891,#20892));
#4912=EDGE_LOOP('',(#20893,#20894,#20895,#20896));
#4913=EDGE_LOOP('',(#20897,#20898,#20899,#20900));
#4914=EDGE_LOOP('',(#20901,#20902,#20903,#20904));
#4915=EDGE_LOOP('',(#20905,#20906,#20907,#20908));
#4916=EDGE_LOOP('',(#20909,#20910,#20911,#20912));
#4917=EDGE_LOOP('',(#20913,#20914,#20915,#20916));
#4918=EDGE_LOOP('',(#20917,#20918,#20919,#20920));
#4919=EDGE_LOOP('',(#20921,#20922,#20923,#20924));
#4920=EDGE_LOOP('',(#20925,#20926,#20927,#20928));
#4921=EDGE_LOOP('',(#20929,#20930,#20931,#20932));
#4922=EDGE_LOOP('',(#20933,#20934,#20935,#20936));
#4923=EDGE_LOOP('',(#20937,#20938,#20939,#20940));
#4924=EDGE_LOOP('',(#20941,#20942,#20943,#20944));
#4925=EDGE_LOOP('',(#20945,#20946,#20947,#20948));
#4926=EDGE_LOOP('',(#20949,#20950,#20951,#20952));
#4927=EDGE_LOOP('',(#20953,#20954,#20955,#20956));
#4928=EDGE_LOOP('',(#20957,#20958,#20959,#20960));
#4929=EDGE_LOOP('',(#20961,#20962,#20963,#20964));
#4930=EDGE_LOOP('',(#20965,#20966,#20967,#20968));
#4931=EDGE_LOOP('',(#20969,#20970,#20971,#20972,#20973));
#4932=EDGE_LOOP('',(#20974,#20975,#20976,#20977,#20978,#20979,#20980,#20981,
#20982,#20983,#20984,#20985,#20986,#20987,#20988,#20989,#20990,#20991,#20992,
#20993,#20994,#20995,#20996,#20997,#20998,#20999,#21000,#21001,#21002,#21003,
#21004,#21005,#21006,#21007,#21008,#21009,#21010,#21011,#21012,#21013,#21014));
#4933=EDGE_LOOP('',(#21015,#21016,#21017,#21018,#21019));
#4934=EDGE_LOOP('',(#21020,#21021,#21022,#21023));
#4935=EDGE_LOOP('',(#21024,#21025,#21026,#21027,#21028,#21029,#21030,#21031,
#21032,#21033,#21034,#21035,#21036,#21037,#21038,#21039,#21040,#21041,#21042,
#21043,#21044,#21045,#21046,#21047,#21048,#21049,#21050,#21051,#21052,#21053,
#21054,#21055,#21056,#21057,#21058,#21059,#21060,#21061,#21062,#21063,#21064));
#4936=EDGE_LOOP('',(#21065,#21066,#21067));
#4937=EDGE_LOOP('',(#21068,#21069,#21070,#21071));
#4938=EDGE_LOOP('',(#21072,#21073,#21074,#21075));
#4939=EDGE_LOOP('',(#21076,#21077,#21078));
#4940=EDGE_LOOP('',(#21079,#21080,#21081,#21082));
#4941=EDGE_LOOP('',(#21083,#21084,#21085,#21086));
#4942=EDGE_LOOP('',(#21087,#21088,#21089));
#4943=EDGE_LOOP('',(#21090,#21091,#21092,#21093));
#4944=EDGE_LOOP('',(#21094,#21095,#21096,#21097));
#4945=EDGE_LOOP('',(#21098,#21099,#21100));
#4946=EDGE_LOOP('',(#21101,#21102,#21103,#21104));
#4947=EDGE_LOOP('',(#21105,#21106,#21107,#21108));
#4948=EDGE_LOOP('',(#21109,#21110,#21111));
#4949=EDGE_LOOP('',(#21112,#21113,#21114,#21115));
#4950=EDGE_LOOP('',(#21116,#21117,#21118,#21119));
#4951=EDGE_LOOP('',(#21120,#21121,#21122));
#4952=EDGE_LOOP('',(#21123,#21124,#21125,#21126));
#4953=EDGE_LOOP('',(#21127,#21128,#21129,#21130));
#4954=EDGE_LOOP('',(#21131,#21132,#21133));
#4955=EDGE_LOOP('',(#21134,#21135,#21136,#21137));
#4956=EDGE_LOOP('',(#21138,#21139,#21140,#21141));
#4957=EDGE_LOOP('',(#21142,#21143,#21144));
#4958=EDGE_LOOP('',(#21145,#21146,#21147,#21148));
#4959=EDGE_LOOP('',(#21149,#21150,#21151,#21152));
#4960=EDGE_LOOP('',(#21153,#21154,#21155));
#4961=EDGE_LOOP('',(#21156,#21157,#21158,#21159));
#4962=EDGE_LOOP('',(#21160,#21161,#21162,#21163));
#4963=EDGE_LOOP('',(#21164,#21165,#21166));
#4964=EDGE_LOOP('',(#21167,#21168,#21169,#21170));
#4965=EDGE_LOOP('',(#21171,#21172,#21173,#21174));
#4966=EDGE_LOOP('',(#21175,#21176,#21177));
#4967=EDGE_LOOP('',(#21178,#21179,#21180,#21181));
#4968=EDGE_LOOP('',(#21182,#21183,#21184,#21185));
#4969=EDGE_LOOP('',(#21186,#21187,#21188));
#4970=EDGE_LOOP('',(#21189,#21190,#21191,#21192));
#4971=EDGE_LOOP('',(#21193,#21194,#21195,#21196));
#4972=EDGE_LOOP('',(#21197,#21198,#21199));
#4973=EDGE_LOOP('',(#21200,#21201,#21202,#21203));
#4974=EDGE_LOOP('',(#21204,#21205,#21206,#21207));
#4975=EDGE_LOOP('',(#21208,#21209,#21210));
#4976=EDGE_LOOP('',(#21211,#21212,#21213,#21214));
#4977=EDGE_LOOP('',(#21215,#21216,#21217,#21218));
#4978=EDGE_LOOP('',(#21219,#21220,#21221));
#4979=EDGE_LOOP('',(#21222,#21223,#21224,#21225));
#4980=EDGE_LOOP('',(#21226,#21227,#21228,#21229));
#4981=EDGE_LOOP('',(#21230,#21231,#21232));
#4982=EDGE_LOOP('',(#21233,#21234,#21235,#21236));
#4983=EDGE_LOOP('',(#21237,#21238,#21239,#21240));
#4984=EDGE_LOOP('',(#21241,#21242,#21243));
#4985=EDGE_LOOP('',(#21244,#21245,#21246,#21247));
#4986=EDGE_LOOP('',(#21248,#21249,#21250,#21251));
#4987=EDGE_LOOP('',(#21252,#21253,#21254,#21255));
#4988=EDGE_LOOP('',(#21256,#21257,#21258,#21259));
#4989=EDGE_LOOP('',(#21260,#21261,#21262,#21263));
#4990=EDGE_LOOP('',(#21264,#21265,#21266));
#4991=EDGE_LOOP('',(#21267,#21268,#21269,#21270));
#4992=EDGE_LOOP('',(#21271,#21272,#21273,#21274));
#4993=EDGE_LOOP('',(#21275,#21276,#21277));
#4994=EDGE_LOOP('',(#21278,#21279,#21280,#21281));
#4995=EDGE_LOOP('',(#21282,#21283,#21284,#21285));
#4996=EDGE_LOOP('',(#21286,#21287,#21288));
#4997=EDGE_LOOP('',(#21289,#21290,#21291,#21292));
#4998=EDGE_LOOP('',(#21293,#21294,#21295,#21296));
#4999=EDGE_LOOP('',(#21297,#21298,#21299));
#5000=EDGE_LOOP('',(#21300,#21301,#21302,#21303));
#5001=EDGE_LOOP('',(#21304,#21305,#21306,#21307));
#5002=EDGE_LOOP('',(#21308,#21309,#21310));
#5003=EDGE_LOOP('',(#21311,#21312,#21313,#21314));
#5004=EDGE_LOOP('',(#21315,#21316,#21317,#21318));
#5005=EDGE_LOOP('',(#21319,#21320,#21321));
#5006=EDGE_LOOP('',(#21322,#21323,#21324,#21325));
#5007=EDGE_LOOP('',(#21326,#21327,#21328,#21329));
#5008=EDGE_LOOP('',(#21330,#21331,#21332));
#5009=EDGE_LOOP('',(#21333,#21334,#21335,#21336));
#5010=EDGE_LOOP('',(#21337,#21338,#21339,#21340));
#5011=EDGE_LOOP('',(#21341,#21342,#21343));
#5012=EDGE_LOOP('',(#21344,#21345,#21346,#21347));
#5013=EDGE_LOOP('',(#21348,#21349,#21350,#21351));
#5014=EDGE_LOOP('',(#21352,#21353,#21354));
#5015=EDGE_LOOP('',(#21355,#21356,#21357,#21358));
#5016=EDGE_LOOP('',(#21359,#21360,#21361,#21362));
#5017=EDGE_LOOP('',(#21363,#21364,#21365));
#5018=EDGE_LOOP('',(#21366,#21367,#21368,#21369));
#5019=EDGE_LOOP('',(#21370,#21371,#21372,#21373));
#5020=EDGE_LOOP('',(#21374,#21375,#21376));
#5021=EDGE_LOOP('',(#21377,#21378,#21379,#21380));
#5022=EDGE_LOOP('',(#21381,#21382,#21383,#21384));
#5023=EDGE_LOOP('',(#21385,#21386,#21387));
#5024=EDGE_LOOP('',(#21388,#21389,#21390,#21391));
#5025=EDGE_LOOP('',(#21392,#21393,#21394,#21395));
#5026=EDGE_LOOP('',(#21396,#21397,#21398));
#5027=EDGE_LOOP('',(#21399,#21400,#21401,#21402));
#5028=EDGE_LOOP('',(#21403,#21404,#21405,#21406));
#5029=EDGE_LOOP('',(#21407,#21408,#21409));
#5030=EDGE_LOOP('',(#21410,#21411,#21412,#21413));
#5031=EDGE_LOOP('',(#21414,#21415,#21416,#21417));
#5032=EDGE_LOOP('',(#21418,#21419,#21420));
#5033=EDGE_LOOP('',(#21421,#21422,#21423,#21424));
#5034=EDGE_LOOP('',(#21425,#21426,#21427,#21428));
#5035=EDGE_LOOP('',(#21429,#21430,#21431));
#5036=EDGE_LOOP('',(#21432,#21433,#21434,#21435));
#5037=EDGE_LOOP('',(#21436,#21437,#21438,#21439));
#5038=EDGE_LOOP('',(#21440,#21441,#21442));
#5039=EDGE_LOOP('',(#21443,#21444,#21445,#21446));
#5040=EDGE_LOOP('',(#21447,#21448,#21449,#21450));
#5041=EDGE_LOOP('',(#21451,#21452,#21453,#21454,#21455,#21456,#21457,#21458,
#21459,#21460,#21461,#21462,#21463,#21464,#21465,#21466,#21467,#21468,#21469,
#21470,#21471,#21472,#21473,#21474,#21475,#21476,#21477,#21478,#21479,#21480,
#21481,#21482,#21483,#21484,#21485,#21486,#21487,#21488,#21489,#21490,#21491,
#21492,#21493,#21494,#21495,#21496,#21497,#21498,#21499,#21500,#21501,#21502,
#21503,#21504,#21505,#21506,#21507,#21508,#21509,#21510,#21511,#21512,#21513,
#21514,#21515,#21516,#21517,#21518,#21519,#21520,#21521,#21522,#21523,#21524,
#21525,#21526,#21527,#21528,#21529,#21530,#21531,#21532,#21533,#21534,#21535,
#21536,#21537,#21538,#21539,#21540,#21541,#21542,#21543,#21544,#21545,#21546,
#21547,#21548,#21549,#21550,#21551,#21552,#21553,#21554,#21555,#21556,#21557,
#21558,#21559,#21560,#21561,#21562,#21563,#21564,#21565,#21566,#21567,#21568,
#21569,#21570,#21571,#21572,#21573,#21574,#21575,#21576,#21577,#21578,#21579,
#21580,#21581,#21582,#21583,#21584,#21585,#21586,#21587,#21588,#21589,#21590,
#21591,#21592,#21593,#21594,#21595,#21596,#21597,#21598));
#5042=EDGE_LOOP('',(#21599,#21600,#21601,#21602));
#5043=EDGE_LOOP('',(#21603,#21604,#21605,#21606));
#5044=EDGE_LOOP('',(#21607,#21608,#21609));
#5045=EDGE_LOOP('',(#21610,#21611,#21612,#21613,#21614,#21615,#21616,#21617,
#21618,#21619,#21620,#21621,#21622,#21623,#21624,#21625,#21626,#21627,#21628,
#21629,#21630,#21631,#21632,#21633,#21634,#21635,#21636,#21637,#21638,#21639,
#21640,#21641,#21642,#21643,#21644,#21645,#21646,#21647,#21648,#21649,#21650,
#21651,#21652,#21653,#21654,#21655,#21656,#21657,#21658,#21659,#21660,#21661,
#21662,#21663,#21664,#21665,#21666,#21667,#21668,#21669,#21670,#21671,#21672,
#21673,#21674,#21675,#21676,#21677,#21678,#21679,#21680,#21681,#21682,#21683,
#21684,#21685,#21686,#21687,#21688,#21689,#21690,#21691,#21692,#21693,#21694,
#21695,#21696,#21697,#21698,#21699,#21700,#21701,#21702,#21703,#21704,#21705,
#21706,#21707,#21708,#21709,#21710,#21711,#21712,#21713,#21714,#21715,#21716,
#21717,#21718,#21719,#21720));
#5046=EDGE_LOOP('',(#21721,#21722,#21723));
#5047=EDGE_LOOP('',(#21724,#21725,#21726,#21727));
#5048=EDGE_LOOP('',(#21728,#21729,#21730,#21731));
#5049=EDGE_LOOP('',(#21732,#21733,#21734,#21735));
#5050=EDGE_LOOP('',(#21736,#21737,#21738,#21739));
#5051=EDGE_LOOP('',(#21740,#21741,#21742,#21743));
#5052=EDGE_LOOP('',(#21744,#21745,#21746,#21747));
#5053=EDGE_LOOP('',(#21748,#21749,#21750,#21751,#21752,#21753));
#5054=EDGE_LOOP('',(#21754));
#5055=EDGE_LOOP('',(#21755));
#5056=EDGE_LOOP('',(#21756,#21757,#21758,#21759));
#5057=EDGE_LOOP('',(#21760,#21761,#21762,#21763));
#5058=EDGE_LOOP('',(#21764,#21765,#21766,#21767,#21768,#21769));
#5059=EDGE_LOOP('',(#21770));
#5060=EDGE_LOOP('',(#21771));
#5061=EDGE_LOOP('',(#21772));
#5062=EDGE_LOOP('',(#21773,#21774,#21775,#21776,#21777,#21778));
#5063=CIRCLE('',#23499,0.521213203435596);
#5064=CIRCLE('',#23500,0.47);
#5065=CIRCLE('',#23503,0.521213203435596);
#5066=CIRCLE('',#23504,0.47);
#5067=CIRCLE('',#23507,0.521213203435596);
#5068=CIRCLE('',#23508,0.47);
#5069=CIRCLE('',#23511,0.521213203435596);
#5070=CIRCLE('',#23512,0.47);
#5071=CIRCLE('',#23516,0.578786796564404);
#5072=CIRCLE('',#23519,0.578786796564404);
#5073=CIRCLE('',#23521,0.58);
#5074=CIRCLE('',#23522,0.58);
#5075=CIRCLE('',#23523,0.283333333333333);
#5076=CIRCLE('',#23524,0.283333333333333);
#5077=CIRCLE('',#23525,0.283333333333333);
#5078=CIRCLE('',#23526,0.58);
#5079=CIRCLE('',#23527,0.58);
#5080=CIRCLE('',#23529,0.6);
#5081=CIRCLE('',#23532,0.6);
#5082=CIRCLE('',#23535,0.578786796564404);
#5083=CIRCLE('',#23536,0.6);
#5084=CIRCLE('',#23539,0.578786796564404);
#5085=CIRCLE('',#23540,0.6);
#5086=CIRCLE('',#23544,0.6);
#5087=CIRCLE('',#23547,0.6);
#5088=CIRCLE('',#23553,0.571213203435596);
#5089=CIRCLE('',#23554,0.52);
#5090=CIRCLE('',#23557,0.571213203435596);
#5091=CIRCLE('',#23558,0.52);
#5092=CIRCLE('',#23561,0.571213203435596);
#5093=CIRCLE('',#23562,0.52);
#5094=CIRCLE('',#23565,0.571213203435596);
#5095=CIRCLE('',#23566,0.52);
#5096=CIRCLE('',#23568,0.578786796564404);
#5097=CIRCLE('',#23571,0.578786796564404);
#5098=CIRCLE('',#23574,0.53);
#5099=CIRCLE('',#23575,0.53);
#5100=CIRCLE('',#23576,0.338333333333333);
#5101=CIRCLE('',#23577,0.338333333333333);
#5102=CIRCLE('',#23578,0.338333333333333);
#5103=CIRCLE('',#23579,0.338333333333333);
#5104=CIRCLE('',#23580,0.53);
#5105=CIRCLE('',#23587,0.578786796564404);
#5106=CIRCLE('',#23588,0.6);
#5107=CIRCLE('',#23591,0.578786796564404);
#5108=CIRCLE('',#23592,0.6);
#5109=CIRCLE('',#23597,0.55);
#5110=CIRCLE('',#23598,0.55);
#5111=CIRCLE('',#23600,0.55);
#5112=CIRCLE('',#23602,0.55);
#5113=CIRCLE('',#23603,0.55);
#5114=CIRCLE('',#23605,0.55);
#5115=CIRCLE('',#23607,0.55);
#5116=CIRCLE('',#23608,0.55);
#5117=CIRCLE('',#23610,0.55);
#5118=CIRCLE('',#23612,0.55);
#5119=CIRCLE('',#23613,0.55);
#5120=CIRCLE('',#23615,0.55);
#5121=CIRCLE('',#23617,0.5);
#5122=CIRCLE('',#23618,0.5);
#5123=CIRCLE('',#23620,0.5);
#5124=CIRCLE('',#23622,0.5);
#5125=CIRCLE('',#23623,0.5);
#5126=CIRCLE('',#23625,0.5);
#5127=CIRCLE('',#23627,0.5);
#5128=CIRCLE('',#23628,0.5);
#5129=CIRCLE('',#23630,0.5);
#5130=CIRCLE('',#23632,0.275);
#5131=CIRCLE('',#23634,0.275);
#5132=CIRCLE('',#23636,0.3);
#5133=CIRCLE('',#23639,0.275);
#5134=CIRCLE('',#23641,0.275);
#5135=CIRCLE('',#23643,0.3);
#5136=CIRCLE('',#23646,0.275);
#5137=CIRCLE('',#23648,0.275);
#5138=CIRCLE('',#23650,0.3);
#5139=CIRCLE('',#23653,0.33);
#5140=CIRCLE('',#23655,0.33);
#5141=CIRCLE('',#23657,0.355);
#5142=CIRCLE('',#23660,0.33);
#5143=CIRCLE('',#23662,0.33);
#5144=CIRCLE('',#23664,0.355);
#5145=CIRCLE('',#23667,0.33);
#5146=CIRCLE('',#23669,0.33);
#5147=CIRCLE('',#23671,0.355);
#5148=CIRCLE('',#23674,0.33);
#5149=CIRCLE('',#23676,0.33);
#5150=CIRCLE('',#23678,0.355);
#5151=CIRCLE('',#23690,0.541213203435597);
#5152=CIRCLE('',#23691,0.49);
#5153=CIRCLE('',#23694,0.541213203435596);
#5154=CIRCLE('',#23695,0.489999999999998);
#5155=CIRCLE('',#23698,0.578786796564402);
#5156=CIRCLE('',#23702,3.33);
#5157=CIRCLE('',#23703,0.2);
#5158=CIRCLE('',#23704,0.435);
#5159=CIRCLE('',#23705,0.435);
#5160=CIRCLE('',#23706,0.435);
#5161=CIRCLE('',#23707,0.2);
#5162=CIRCLE('',#23708,0.2);
#5163=CIRCLE('',#23711,0.305);
#5164=CIRCLE('',#23712,0.305);
#5165=CIRCLE('',#23713,0.305);
#5166=CIRCLE('',#23718,0.6);
#5167=CIRCLE('',#23721,0.578786796564403);
#5168=CIRCLE('',#23722,0.6);
#5169=CIRCLE('',#23732,0.578786796564403);
#5170=CIRCLE('',#23733,0.6);
#5171=CIRCLE('',#23736,0.578786796564403);
#5172=CIRCLE('',#23737,0.6);
#5173=CIRCLE('',#23739,0.541213203435596);
#5174=CIRCLE('',#23747,0.489999999999998);
#5175=CIRCLE('',#23750,0.541213203435597);
#5176=CIRCLE('',#23751,0.49);
#5177=CIRCLE('',#23756,3.805);
#5178=CIRCLE('',#23757,0.2);
#5179=CIRCLE('',#23758,0.42375);
#5180=CIRCLE('',#23759,0.423750000000001);
#5181=CIRCLE('',#23760,0.205);
#5182=CIRCLE('',#23761,0.205000000000001);
#5183=CIRCLE('',#23762,0.205);
#5184=CIRCLE('',#23763,0.423749999999999);
#5185=CIRCLE('',#23764,0.2);
#5186=CIRCLE('',#23765,0.2);
#5187=CIRCLE('',#23767,3.3);
#5188=CIRCLE('',#23769,3.3);
#5189=CIRCLE('',#23771,3.775);
#5190=CIRCLE('',#23772,3.775);
#5191=CIRCLE('',#23774,3.775);
#5192=CIRCLE('',#23776,3.33);
#5193=CIRCLE('',#23779,0.17);
#5194=CIRCLE('',#23780,0.17);
#5195=CIRCLE('',#23782,0.17);
#5196=CIRCLE('',#23785,0.17);
#5197=CIRCLE('',#23786,0.17);
#5198=CIRCLE('',#23788,0.17);
#5199=CIRCLE('',#23791,0.17);
#5200=CIRCLE('',#23792,0.17);
#5201=CIRCLE('',#23794,0.17);
#5202=CIRCLE('',#23797,0.405);
#5203=CIRCLE('',#23799,0.405);
#5204=CIRCLE('',#23801,0.404999999999999);
#5205=CIRCLE('',#23803,0.404999999999999);
#5206=CIRCLE('',#23805,0.405);
#5207=CIRCLE('',#23807,0.405);
#5208=CIRCLE('',#23809,0.485000000000001);
#5209=CIRCLE('',#23810,0.433786796564405);
#5210=CIRCLE('',#23812,0.426213203435597);
#5211=CIRCLE('',#23813,0.426213203435597);
#5212=CIRCLE('',#23816,0.405);
#5213=CIRCLE('',#23817,0.405);
#5214=CIRCLE('',#23819,0.405);
#5215=CIRCLE('',#23822,0.255);
#5216=CIRCLE('',#23824,0.255);
#5217=CIRCLE('',#23827,0.255);
#5218=CIRCLE('',#23829,0.255);
#5219=CIRCLE('',#23832,0.255);
#5220=CIRCLE('',#23834,0.255);
#5221=CIRCLE('',#23840,0.155);
#5222=CIRCLE('',#23842,0.155);
#5223=CIRCLE('',#23845,0.155);
#5224=CIRCLE('',#23847,0.155);
#5225=CIRCLE('',#23850,0.155);
#5226=CIRCLE('',#23852,0.155);
#5227=CIRCLE('',#23858,0.541213203435597);
#5228=CIRCLE('',#23859,0.49);
#5229=CIRCLE('',#23862,0.541213203435597);
#5230=CIRCLE('',#23863,0.49);
#5231=CIRCLE('',#23866,0.541213203435597);
#5232=CIRCLE('',#23867,0.49);
#5233=CIRCLE('',#23870,0.541213203435596);
#5234=CIRCLE('',#23871,0.489999999999999);
#5235=CIRCLE('',#23875,0.578786796564404);
#5236=CIRCLE('',#23878,0.578786796564403);
#5237=CIRCLE('',#23880,3.805);
#5238=CIRCLE('',#23881,0.255);
#5239=CIRCLE('',#23882,0.255);
#5240=CIRCLE('',#23883,0.255);
#5241=CIRCLE('',#23886,0.578786796564403);
#5242=CIRCLE('',#23887,0.6);
#5243=CIRCLE('',#23890,0.6);
#5244=CIRCLE('',#23893,0.6);
#5245=CIRCLE('',#23896,0.578786796564403);
#5246=CIRCLE('',#23897,0.6);
#5247=CIRCLE('',#23899,0.6);
#5248=CIRCLE('',#23902,0.6);
#5249=CIRCLE('',#23907,0.578786796564403);
#5250=CIRCLE('',#23910,0.578786796564404);
#5251=CIRCLE('',#23913,0.578786796564404);
#5252=CIRCLE('',#23914,0.6);
#5253=CIRCLE('',#23917,0.578786796564404);
#5254=CIRCLE('',#23918,0.6);
#5255=CIRCLE('',#23922,0.541213203435596);
#5256=CIRCLE('',#23925,0.541213203435597);
#5257=CIRCLE('',#23927,3.775);
#5258=CIRCLE('',#23928,3.775);
#5259=CIRCLE('',#23930,3.775);
#5260=CIRCLE('',#23932,0.49);
#5261=CIRCLE('',#23935,0.489999999999998);
#5262=CIRCLE('',#23938,0.541213203435597);
#5263=CIRCLE('',#23939,0.49);
#5264=CIRCLE('',#23942,0.541213203435597);
#5265=CIRCLE('',#23943,0.49);
#5266=CIRCLE('',#23949,3.38);
#5267=CIRCLE('',#23951,3.3);
#5268=CIRCLE('',#23952,3.33);
#5269=CIRCLE('',#23954,3.3);
#5270=CIRCLE('',#23957,3.3287867965644);
#5271=CIRCLE('',#23959,3.3212132034356);
#5272=CIRCLE('',#23962,0.205);
#5273=CIRCLE('',#23964,0.205);
#5274=CIRCLE('',#23967,0.205);
#5275=CIRCLE('',#23969,0.205);
#5276=CIRCLE('',#23972,0.205);
#5277=CIRCLE('',#23974,0.205);
#5278=CIRCLE('',#23985,4.0212132034356);
#5279=CIRCLE('',#23986,4.);
#5280=CIRCLE('',#23987,4.);
#5281=CIRCLE('',#23989,4.);
#5282=CIRCLE('',#23990,4.);
#5283=CIRCLE('',#23992,4.0287867965644);
#5284=CIRCLE('',#23994,4.0212132034356);
#5285=CIRCLE('',#23996,4.0287867965644);
#5286=CIRCLE('',#23998,4.08);
#5287=CIRCLE('',#24000,4.72);
#5288=CIRCLE('',#24001,0.205);
#5289=CIRCLE('',#24002,0.204999999999999);
#5290=CIRCLE('',#24003,0.205);
#5291=CIRCLE('',#24005,4.7712132034356);
#5292=CIRCLE('',#24007,4.7787867965644);
#5293=CIRCLE('',#24009,4.08);
#5294=CIRCLE('',#24011,4.72);
#5295=CIRCLE('',#24013,4.8);
#5296=CIRCLE('',#24014,4.8);
#5297=CIRCLE('',#24016,4.8);
#5298=CIRCLE('',#24017,4.8);
#5299=CIRCLE('',#24019,4.7712132034356);
#5300=CIRCLE('',#24021,4.7787867965644);
#5301=CIRCLE('',#24024,0.155);
#5302=CIRCLE('',#24026,0.155);
#5303=CIRCLE('',#24029,0.154999999999999);
#5304=CIRCLE('',#24031,0.154999999999999);
#5305=CIRCLE('',#24034,0.155);
#5306=CIRCLE('',#24036,0.155);
#5307=CIRCLE('',#24040,0.2);
#5308=CIRCLE('',#24041,0.17);
#5309=CIRCLE('',#24042,0.17);
#5310=CIRCLE('',#24044,0.17);
#5311=CIRCLE('',#24046,4.66);
#5312=CIRCLE('',#24047,0.2);
#5313=CIRCLE('',#24048,0.200000000000001);
#5314=CIRCLE('',#24049,0.2);
#5315=CIRCLE('',#24050,3.34);
#5316=CIRCLE('',#24051,0.2);
#5317=CIRCLE('',#24052,0.2);
#5318=CIRCLE('',#24054,0.2);
#5319=CIRCLE('',#24056,4.66);
#5320=CIRCLE('',#24057,0.2);
#5321=CIRCLE('',#24058,0.200000000000001);
#5322=CIRCLE('',#24059,0.2);
#5323=CIRCLE('',#24060,3.34);
#5324=CIRCLE('',#24061,0.2);
#5325=CIRCLE('',#24062,0.2);
#5326=CIRCLE('',#24064,0.17);
#5327=CIRCLE('',#24065,0.17);
#5328=CIRCLE('',#24067,0.17);
#5329=CIRCLE('',#24070,0.17);
#5330=CIRCLE('',#24071,0.17);
#5331=CIRCLE('',#24073,0.17);
#5332=CIRCLE('',#24076,0.170000000000001);
#5333=CIRCLE('',#24077,0.170000000000001);
#5334=CIRCLE('',#24079,0.170000000000001);
#5335=CIRCLE('',#24082,0.17);
#5336=CIRCLE('',#24083,0.17);
#5337=CIRCLE('',#24085,0.17);
#5338=CIRCLE('',#24088,0.17);
#5339=CIRCLE('',#24089,0.17);
#5340=CIRCLE('',#24091,0.17);
#5341=CIRCLE('',#24094,4.7);
#5342=CIRCLE('',#24095,4.7);
#5343=CIRCLE('',#24097,4.7);
#5344=CIRCLE('',#24098,4.7);
#5345=CIRCLE('',#24101,3.3);
#5346=CIRCLE('',#24102,3.3);
#5347=CIRCLE('',#24104,3.3);
#5348=CIRCLE('',#24105,3.3);
#5349=CIRCLE('',#24109,0.3954);
#5350=CIRCLE('',#24110,0.3954);
#5351=CIRCLE('',#24121,0.352375);
#5352=CIRCLE('',#24133,0.352375);
#5353=CIRCLE('',#24136,0.08);
#5354=CIRCLE('',#24137,0.08);
#5355=CIRCLE('',#24139,0.08);
#5356=CIRCLE('',#24140,0.08);
#5357=CIRCLE('',#24142,0.08);
#5358=CIRCLE('',#24143,0.08);
#5359=CIRCLE('',#24145,0.08);
#5360=CIRCLE('',#24146,0.08);
#5361=CIRCLE('',#24149,0.5);
#5362=CIRCLE('',#24152,0.5);
#5363=CIRCLE('',#24155,0.5);
#5364=CIRCLE('',#24158,0.5);
#5365=CIRCLE('',#24161,0.5);
#5366=CIRCLE('',#24164,0.5);
#5367=CIRCLE('',#24167,0.5);
#5368=CIRCLE('',#24170,0.5);
#5369=CIRCLE('',#24173,0.5);
#5370=CIRCLE('',#24176,0.5);
#5371=CIRCLE('',#24179,0.5);
#5372=CIRCLE('',#24182,0.5);
#5373=CIRCLE('',#24185,0.5);
#5374=CIRCLE('',#24188,0.5);
#5375=CIRCLE('',#24191,0.5);
#5376=CIRCLE('',#24194,0.5);
#5377=CIRCLE('',#24197,0.5);
#5378=CIRCLE('',#24200,0.5);
#5379=CIRCLE('',#24203,0.5);
#5380=CIRCLE('',#24206,0.5);
#5381=CIRCLE('',#24209,0.5);
#5382=CIRCLE('',#24212,0.5);
#5383=CIRCLE('',#24215,0.5);
#5384=CIRCLE('',#24216,0.5);
#5385=CIRCLE('',#24219,0.5);
#5386=CIRCLE('',#24220,0.5);
#5387=CIRCLE('',#24223,0.5);
#5388=CIRCLE('',#24226,0.5);
#5389=CIRCLE('',#24229,0.5);
#5390=CIRCLE('',#24232,0.5);
#5391=CIRCLE('',#24235,0.5);
#5392=CIRCLE('',#24238,0.5);
#5393=CIRCLE('',#24241,0.5);
#5394=CIRCLE('',#24244,0.5);
#5395=CIRCLE('',#24247,0.5);
#5396=CIRCLE('',#24250,0.5);
#5397=CIRCLE('',#24253,0.5);
#5398=CIRCLE('',#24256,0.5);
#5399=CIRCLE('',#24259,0.5);
#5400=CIRCLE('',#24262,0.5);
#5401=CIRCLE('',#24265,0.5);
#5402=CIRCLE('',#24268,0.5);
#5403=CIRCLE('',#24271,0.5);
#5404=CIRCLE('',#24274,0.5);
#5405=CIRCLE('',#24277,0.5);
#5406=CIRCLE('',#24280,0.5);
#5407=CIRCLE('',#24283,0.5);
#5408=CIRCLE('',#24286,0.5);
#5409=CIRCLE('',#24289,0.5);
#5410=CIRCLE('',#24292,0.5);
#5411=CIRCLE('',#24294,0.06);
#5412=CIRCLE('',#24295,0.06);
#5413=CIRCLE('',#24297,0.03);
#5414=CIRCLE('',#24300,0.25);
#5415=CIRCLE('',#24302,0.25);
#5416=CIRCLE('',#24304,0.5);
#5417=CIRCLE('',#24305,0.5);
#5418=CIRCLE('',#24307,0.52);
#5419=CIRCLE('',#24309,0.52);
#5420=CIRCLE('',#24311,0.48);
#5421=CIRCLE('',#24321,0.3954);
#5422=CIRCLE('',#24328,0.36);
#5423=CIRCLE('',#24333,3.7);
#5424=CIRCLE('',#24334,3.75);
#5425=CIRCLE('',#24335,3.75);
#5426=CIRCLE('',#24337,3.75);
#5427=CIRCLE('',#24338,3.75);
#5428=CIRCLE('',#24341,3.7);
#5429=CIRCLE('',#24345,0.385);
#5430=CIRCLE('',#24346,0.385);
#5431=CIRCLE('',#24348,0.4);
#5432=CIRCLE('',#24350,0.4);
#5433=CIRCLE('',#24352,0.4);
#5434=CIRCLE('',#24353,0.4);
#5435=CIRCLE('',#24355,0.385);
#5436=CIRCLE('',#24356,0.385);
#5437=CIRCLE('',#24358,0.4);
#5438=CIRCLE('',#24360,0.4);
#5439=CIRCLE('',#24363,0.38);
#5440=CIRCLE('',#24365,0.4);
#5441=CIRCLE('',#24366,0.4);
#5442=CIRCLE('',#24368,0.25);
#5443=CIRCLE('',#24370,0.38);
#5444=CIRCLE('',#24372,0.25);
#5445=CIRCLE('',#24376,0.578786796564404);
#5446=CIRCLE('',#24377,0.578786796564404);
#5447=CIRCLE('',#24378,0.6);
#5448=CIRCLE('',#24379,0.6);
#5449=CIRCLE('',#24381,0.6);
#5450=CIRCLE('',#24382,0.6);
#5451=CIRCLE('',#24384,0.56);
#5452=CIRCLE('',#24386,0.57);
#5453=CIRCLE('',#24388,0.4);
#5454=CIRCLE('',#24391,0.3);
#5455=CIRCLE('',#24394,0.3);
#5456=CIRCLE('',#24397,0.3);
#5457=CIRCLE('',#24400,0.3);
#5458=CIRCLE('',#24403,0.3);
#5459=CIRCLE('',#24406,0.3);
#5460=CIRCLE('',#24409,0.3);
#5461=CIRCLE('',#24412,0.3);
#5462=CIRCLE('',#24415,0.3);
#5463=CIRCLE('',#24418,0.3);
#5464=CIRCLE('',#24421,0.3);
#5465=CIRCLE('',#24424,0.3);
#5466=CIRCLE('',#24427,0.3);
#5467=CIRCLE('',#24430,0.3);
#5468=CIRCLE('',#24433,0.3);
#5469=CIRCLE('',#24436,0.3);
#5470=CIRCLE('',#24439,0.3);
#5471=CIRCLE('',#24440,0.3);
#5472=CIRCLE('',#24443,0.3);
#5473=CIRCLE('',#24444,0.3);
#5474=CIRCLE('',#24447,0.3);
#5475=CIRCLE('',#24450,0.3);
#5476=CIRCLE('',#24453,0.3);
#5477=CIRCLE('',#24456,0.3);
#5478=CIRCLE('',#24459,0.3);
#5479=CIRCLE('',#24462,0.3);
#5480=CIRCLE('',#24465,0.3);
#5481=CIRCLE('',#24468,0.3);
#5482=CIRCLE('',#24471,0.3);
#5483=CIRCLE('',#24474,0.3);
#5484=CIRCLE('',#24477,0.3);
#5485=CIRCLE('',#24480,0.3);
#5486=CIRCLE('',#24483,0.3);
#5487=CIRCLE('',#24486,0.3);
#5488=CIRCLE('',#24489,0.3);
#5489=CIRCLE('',#24492,0.3);
#5490=CIRCLE('',#24495,0.3);
#5491=CIRCLE('',#24498,0.3);
#5492=CIRCLE('',#24500,0.24);
#5493=CIRCLE('',#24501,0.24);
#5494=CIRCLE('',#24503,0.28);
#5495=CIRCLE('',#24504,0.28);
#5496=CIRCLE('',#24507,0.38);
#5497=CIRCLE('',#24510,0.4);
#5498=CIRCLE('',#24513,0.3);
#5499=CIRCLE('',#24515,0.3);
#5500=CIRCLE('',#24517,0.18);
#5501=CIRCLE('',#24519,0.18);
#5502=CIRCLE('',#24523,3.35);
#5503=CIRCLE('',#24524,3.35);
#5504=CIRCLE('',#24526,3.75);
#5505=CIRCLE('',#24528,3.75);
#5506=CIRCLE('',#24532,0.255000000000001);
#5507=CIRCLE('',#24533,0.225000000000001);
#5508=CIRCLE('',#24535,0.225000000000001);
#5509=CIRCLE('',#24536,0.225000000000001);
#5510=CIRCLE('',#24538,0.32);
#5511=CIRCLE('',#24539,0.32);
#5512=CIRCLE('',#24541,0.255000000000001);
#5513=CIRCLE('',#24543,0.17);
#5514=CIRCLE('',#24544,0.17);
#5515=CIRCLE('',#24545,0.32);
#5516=CIRCLE('',#24546,0.32);
#5517=CIRCLE('',#24549,0.35);
#5518=CIRCLE('',#24552,0.35);
#5519=CIRCLE('',#24557,0.2);
#5520=CIRCLE('',#24558,0.17);
#5521=CIRCLE('',#24561,0.2);
#5522=CIRCLE('',#24562,0.17);
#5523=CIRCLE('',#24565,0.2);
#5524=CIRCLE('',#24570,0.2);
#5525=CIRCLE('',#24573,0.35);
#5526=CIRCLE('',#24576,0.35);
#5527=CIRCLE('',#24588,0.21);
#5528=CIRCLE('',#24589,0.21);
#5529=CIRCLE('',#24591,0.4);
#5530=CIRCLE('',#24593,0.4);
#5531=CIRCLE('',#24597,0.1954);
#5532=CIRCLE('',#24598,0.1954);
#5533=CIRCLE('',#24599,0.1954);
#5534=CIRCLE('',#24614,0.15555);
#5535=CIRCLE('',#24629,0.15555);
#5536=CIRCLE('',#24631,0.15555);
#5537=CIRCLE('',#24634,0.1954);
#5538=CIRCLE('',#24636,0.2);
#5539=CIRCLE('',#24639,0.6);
#5540=CIRCLE('',#24642,0.6);
#5541=CIRCLE('',#24645,0.6);
#5542=CIRCLE('',#24648,0.6);
#5543=CIRCLE('',#24651,0.6);
#5544=CIRCLE('',#24654,0.6);
#5545=CIRCLE('',#24657,0.6);
#5546=CIRCLE('',#24660,0.6);
#5547=CIRCLE('',#24663,0.6);
#5548=CIRCLE('',#24666,0.6);
#5549=CIRCLE('',#24669,0.6);
#5550=CIRCLE('',#24672,0.6);
#5551=CIRCLE('',#24675,0.6);
#5552=CIRCLE('',#24678,0.6);
#5553=CIRCLE('',#24681,0.6);
#5554=CIRCLE('',#24684,0.6);
#5555=CIRCLE('',#24687,0.6);
#5556=CIRCLE('',#24690,0.6);
#5557=CIRCLE('',#24693,0.6);
#5558=CIRCLE('',#24696,0.6);
#5559=CIRCLE('',#24699,0.6);
#5560=CIRCLE('',#24702,0.6);
#5561=CIRCLE('',#24705,0.6);
#5562=CIRCLE('',#24706,0.6);
#5563=CIRCLE('',#24709,0.6);
#5564=CIRCLE('',#24710,0.6);
#5565=CIRCLE('',#24713,0.6);
#5566=CIRCLE('',#24716,0.6);
#5567=CIRCLE('',#24719,0.6);
#5568=CIRCLE('',#24722,0.6);
#5569=CIRCLE('',#24725,0.6);
#5570=CIRCLE('',#24728,0.6);
#5571=CIRCLE('',#24731,0.6);
#5572=CIRCLE('',#24734,0.6);
#5573=CIRCLE('',#24737,0.6);
#5574=CIRCLE('',#24740,0.6);
#5575=CIRCLE('',#24743,0.6);
#5576=CIRCLE('',#24746,0.6);
#5577=CIRCLE('',#24749,0.6);
#5578=CIRCLE('',#24752,0.6);
#5579=CIRCLE('',#24755,0.6);
#5580=CIRCLE('',#24758,0.6);
#5581=CIRCLE('',#24761,0.6);
#5582=CIRCLE('',#24764,0.6);
#5583=CIRCLE('',#24767,0.6);
#5584=CIRCLE('',#24770,0.6);
#5585=CIRCLE('',#24773,0.6);
#5586=CIRCLE('',#24776,0.6);
#5587=CIRCLE('',#24779,0.6);
#5588=CIRCLE('',#24782,0.6);
#5589=CIRCLE('',#24784,0.16);
#5590=CIRCLE('',#24787,0.55);
#5591=CIRCLE('',#24789,0.6);
#5592=CIRCLE('',#24791,0.6);
#5593=CIRCLE('',#24793,0.5);
#5594=CIRCLE('',#24797,0.14635);
#5595=CIRCLE('',#24798,0.14635);
#5596=CIRCLE('',#24799,0.14635);
#5597=CIRCLE('',#24814,0.117775);
#5598=CIRCLE('',#24830,0.14635);
#5599=CIRCLE('',#24831,0.14635);
#5600=CIRCLE('',#24833,0.117775);
#5601=CIRCLE('',#24836,0.275);
#5602=CIRCLE('',#24840,0.275);
#5603=CIRCLE('',#24844,0.275);
#5604=CIRCLE('',#24848,0.275);
#5605=CIRCLE('',#24852,0.275);
#5606=CIRCLE('',#24856,0.275);
#5607=CIRCLE('',#24860,0.275);
#5608=CIRCLE('',#24864,0.275);
#5609=CIRCLE('',#24868,0.275);
#5610=CIRCLE('',#24872,0.275);
#5611=CIRCLE('',#24876,0.275);
#5612=CIRCLE('',#24880,0.275);
#5613=CIRCLE('',#24884,0.275);
#5614=CIRCLE('',#24888,0.275);
#5615=CIRCLE('',#24892,0.275);
#5616=CIRCLE('',#24896,0.275);
#5617=CIRCLE('',#24900,0.275);
#5618=CIRCLE('',#24904,0.275);
#5619=CIRCLE('',#24905,0.275);
#5620=CIRCLE('',#24909,0.275);
#5621=CIRCLE('',#24913,0.275);
#5622=CIRCLE('',#24917,0.275);
#5623=CIRCLE('',#24921,0.275);
#5624=CIRCLE('',#24925,0.275);
#5625=CIRCLE('',#24929,0.275);
#5626=CIRCLE('',#24933,0.275);
#5627=CIRCLE('',#24937,0.275);
#5628=CIRCLE('',#24941,0.275);
#5629=CIRCLE('',#24945,0.275);
#5630=CIRCLE('',#24949,0.275);
#5631=CIRCLE('',#24953,0.275);
#5632=CIRCLE('',#24957,0.275);
#5633=CIRCLE('',#24961,0.275);
#5634=CIRCLE('',#24965,0.275);
#5635=CIRCLE('',#24969,0.275);
#5636=CIRCLE('',#24973,0.275);
#5637=CIRCLE('',#24977,0.275);
#5638=CIRCLE('',#24978,0.275);
#5639=CIRCLE('',#24979,0.275);
#5640=CIRCLE('',#24980,0.275);
#5641=CIRCLE('',#24981,0.275);
#5642=CIRCLE('',#24982,0.275);
#5643=CIRCLE('',#24983,0.275);
#5644=CIRCLE('',#24984,0.275);
#5645=CIRCLE('',#24985,0.275);
#5646=CIRCLE('',#24986,0.275);
#5647=CIRCLE('',#24987,0.275);
#5648=CIRCLE('',#24988,0.275);
#5649=CIRCLE('',#24989,0.275);
#5650=CIRCLE('',#24990,0.275);
#5651=CIRCLE('',#24991,0.275);
#5652=CIRCLE('',#24992,0.275);
#5653=CIRCLE('',#24993,0.275);
#5654=CIRCLE('',#24994,0.275);
#5655=CIRCLE('',#24995,0.275);
#5656=CIRCLE('',#24996,0.275);
#5657=CIRCLE('',#24997,0.275);
#5658=CIRCLE('',#24998,0.275);
#5659=CIRCLE('',#24999,0.275);
#5660=CIRCLE('',#25000,0.275);
#5661=CIRCLE('',#25001,0.275);
#5662=CIRCLE('',#25002,0.275);
#5663=CIRCLE('',#25003,0.275);
#5664=CIRCLE('',#25004,0.275);
#5665=CIRCLE('',#25005,0.275);
#5666=CIRCLE('',#25006,0.275);
#5667=CIRCLE('',#25007,0.275);
#5668=CIRCLE('',#25008,0.275);
#5669=CIRCLE('',#25009,0.275);
#5670=CIRCLE('',#25010,0.275);
#5671=CIRCLE('',#25011,0.275);
#5672=CIRCLE('',#25012,0.275);
#5673=CIRCLE('',#25013,0.275);
#5674=CIRCLE('',#25014,0.275);
#5675=CIRCLE('',#25019,0.26);
#5676=CIRCLE('',#25021,0.113891921086774);
#5677=CIRCLE('',#25030,0.114);
#5678=CIRCLE('',#25033,0.14635);
#5679=CIRCLE('',#25035,0.16);
#5680=CIRCLE('',#25040,0.14635);
#5681=CIRCLE('',#25041,0.14635);
#5682=CIRCLE('',#25042,0.14635);
#5683=CIRCLE('',#25101,0.117775);
#5684=CIRCLE('',#25161,0.14635);
#5685=CIRCLE('',#25162,0.14635);
#5686=CIRCLE('',#25164,0.117775);
#5687=CIRCLE('',#25167,0.275);
#5688=CIRCLE('',#25171,0.275);
#5689=CIRCLE('',#25175,0.275);
#5690=CIRCLE('',#25179,0.275);
#5691=CIRCLE('',#25183,0.275);
#5692=CIRCLE('',#25187,0.275);
#5693=CIRCLE('',#25191,0.275);
#5694=CIRCLE('',#25195,0.275);
#5695=CIRCLE('',#25199,0.275);
#5696=CIRCLE('',#25203,0.275);
#5697=CIRCLE('',#25207,0.275);
#5698=CIRCLE('',#25211,0.275);
#5699=CIRCLE('',#25215,0.275);
#5700=CIRCLE('',#25219,0.275);
#5701=CIRCLE('',#25223,0.275);
#5702=CIRCLE('',#25227,0.275);
#5703=CIRCLE('',#25231,0.275);
#5704=CIRCLE('',#25235,0.275);
#5705=CIRCLE('',#25236,0.275);
#5706=CIRCLE('',#25240,0.275);
#5707=CIRCLE('',#25244,0.275);
#5708=CIRCLE('',#25248,0.275);
#5709=CIRCLE('',#25252,0.275);
#5710=CIRCLE('',#25256,0.275);
#5711=CIRCLE('',#25260,0.275);
#5712=CIRCLE('',#25264,0.275);
#5713=CIRCLE('',#25268,0.275);
#5714=CIRCLE('',#25272,0.275);
#5715=CIRCLE('',#25276,0.275);
#5716=CIRCLE('',#25280,0.275);
#5717=CIRCLE('',#25284,0.275);
#5718=CIRCLE('',#25288,0.275);
#5719=CIRCLE('',#25292,0.275);
#5720=CIRCLE('',#25296,0.275);
#5721=CIRCLE('',#25300,0.275);
#5722=CIRCLE('',#25304,0.275);
#5723=CIRCLE('',#25308,0.275);
#5724=CIRCLE('',#25309,0.275);
#5725=CIRCLE('',#25310,0.275);
#5726=CIRCLE('',#25311,0.275);
#5727=CIRCLE('',#25312,0.275);
#5728=CIRCLE('',#25313,0.275);
#5729=CIRCLE('',#25314,0.275);
#5730=CIRCLE('',#25315,0.275);
#5731=CIRCLE('',#25316,0.275);
#5732=CIRCLE('',#25317,0.275);
#5733=CIRCLE('',#25318,0.275);
#5734=CIRCLE('',#25319,0.275);
#5735=CIRCLE('',#25320,0.275);
#5736=CIRCLE('',#25321,0.275);
#5737=CIRCLE('',#25322,0.275);
#5738=CIRCLE('',#25323,0.275);
#5739=CIRCLE('',#25324,0.275);
#5740=CIRCLE('',#25325,0.275);
#5741=CIRCLE('',#25326,0.275);
#5742=CIRCLE('',#25327,0.275);
#5743=CIRCLE('',#25328,0.275);
#5744=CIRCLE('',#25329,0.275);
#5745=CIRCLE('',#25330,0.275);
#5746=CIRCLE('',#25331,0.275);
#5747=CIRCLE('',#25332,0.275);
#5748=CIRCLE('',#25333,0.275);
#5749=CIRCLE('',#25334,0.275);
#5750=CIRCLE('',#25335,0.275);
#5751=CIRCLE('',#25336,0.275);
#5752=CIRCLE('',#25337,0.275);
#5753=CIRCLE('',#25338,0.275);
#5754=CIRCLE('',#25339,0.275);
#5755=CIRCLE('',#25340,0.275);
#5756=CIRCLE('',#25341,0.275);
#5757=CIRCLE('',#25342,0.275);
#5758=CIRCLE('',#25343,0.275);
#5759=CIRCLE('',#25344,0.275);
#5760=CIRCLE('',#25345,0.275);
#5761=CIRCLE('',#25350,0.26);
#5762=CIRCLE('',#25352,0.113891921086774);
#5763=CIRCLE('',#25361,0.114);
#5764=CIRCLE('',#25364,0.14635);
#5765=CIRCLE('',#25366,0.16);
#5766=CIRCLE('',#25371,0.24505);
#5767=CIRCLE('',#25372,0.24505);
#5768=CIRCLE('',#25373,0.24505);
#5769=CIRCLE('',#25392,0.199475);
#5770=CIRCLE('',#25412,0.24505);
#5771=CIRCLE('',#25413,0.24505);
#5772=CIRCLE('',#25415,0.199475);
#5773=CIRCLE('',#25418,0.425);
#5774=CIRCLE('',#25422,0.425);
#5775=CIRCLE('',#25426,0.425);
#5776=CIRCLE('',#25430,0.425);
#5777=CIRCLE('',#25434,0.425);
#5778=CIRCLE('',#25438,0.425);
#5779=CIRCLE('',#25442,0.425);
#5780=CIRCLE('',#25446,0.425);
#5781=CIRCLE('',#25450,0.425);
#5782=CIRCLE('',#25454,0.425);
#5783=CIRCLE('',#25458,0.425);
#5784=CIRCLE('',#25462,0.425);
#5785=CIRCLE('',#25466,0.425);
#5786=CIRCLE('',#25470,0.425);
#5787=CIRCLE('',#25474,0.425);
#5788=CIRCLE('',#25478,0.425);
#5789=CIRCLE('',#25482,0.425);
#5790=CIRCLE('',#25486,0.425);
#5791=CIRCLE('',#25487,0.425);
#5792=CIRCLE('',#25491,0.425);
#5793=CIRCLE('',#25495,0.425);
#5794=CIRCLE('',#25499,0.425);
#5795=CIRCLE('',#25503,0.425);
#5796=CIRCLE('',#25507,0.425);
#5797=CIRCLE('',#25511,0.425);
#5798=CIRCLE('',#25515,0.425);
#5799=CIRCLE('',#25519,0.425);
#5800=CIRCLE('',#25523,0.425);
#5801=CIRCLE('',#25527,0.425);
#5802=CIRCLE('',#25531,0.425);
#5803=CIRCLE('',#25535,0.425);
#5804=CIRCLE('',#25539,0.425);
#5805=CIRCLE('',#25543,0.425);
#5806=CIRCLE('',#25547,0.425);
#5807=CIRCLE('',#25551,0.425);
#5808=CIRCLE('',#25555,0.425);
#5809=CIRCLE('',#25559,0.425);
#5810=CIRCLE('',#25560,0.425);
#5811=CIRCLE('',#25561,0.425);
#5812=CIRCLE('',#25562,0.425);
#5813=CIRCLE('',#25563,0.425);
#5814=CIRCLE('',#25564,0.425);
#5815=CIRCLE('',#25565,0.425);
#5816=CIRCLE('',#25566,0.425);
#5817=CIRCLE('',#25567,0.425);
#5818=CIRCLE('',#25568,0.425);
#5819=CIRCLE('',#25569,0.425);
#5820=CIRCLE('',#25570,0.425);
#5821=CIRCLE('',#25571,0.425);
#5822=CIRCLE('',#25572,0.425);
#5823=CIRCLE('',#25573,0.425);
#5824=CIRCLE('',#25574,0.425);
#5825=CIRCLE('',#25575,0.425);
#5826=CIRCLE('',#25576,0.425);
#5827=CIRCLE('',#25577,0.425);
#5828=CIRCLE('',#25578,0.425);
#5829=CIRCLE('',#25579,0.425);
#5830=CIRCLE('',#25580,0.425);
#5831=CIRCLE('',#25581,0.425);
#5832=CIRCLE('',#25582,0.425);
#5833=CIRCLE('',#25583,0.425);
#5834=CIRCLE('',#25584,0.425);
#5835=CIRCLE('',#25585,0.425);
#5836=CIRCLE('',#25586,0.425);
#5837=CIRCLE('',#25587,0.425);
#5838=CIRCLE('',#25588,0.425);
#5839=CIRCLE('',#25589,0.425);
#5840=CIRCLE('',#25590,0.425);
#5841=CIRCLE('',#25591,0.425);
#5842=CIRCLE('',#25592,0.425);
#5843=CIRCLE('',#25593,0.425);
#5844=CIRCLE('',#25594,0.425);
#5845=CIRCLE('',#25595,0.425);
#5846=CIRCLE('',#25596,0.425);
#5847=CIRCLE('',#25601,0.41);
#5848=CIRCLE('',#25603,0.183165823577449);
#5849=CIRCLE('',#25612,0.19);
#5850=CIRCLE('',#25615,0.24505);
#5851=CIRCLE('',#25617,0.26);
#5852=LINE('',#31820,#7697);
#5853=LINE('',#31824,#7698);
#5854=LINE('',#31829,#7699);
#5855=LINE('',#31830,#7700);
#5856=LINE('',#31831,#7701);
#5857=LINE('',#31835,#7702);
#5858=LINE('',#31841,#7703);
#5859=LINE('',#31842,#7704);
#5860=LINE('',#31843,#7705);
#5861=LINE('',#31847,#7706);
#5862=LINE('',#31853,#7707);
#5863=LINE('',#31854,#7708);
#5864=LINE('',#31855,#7709);
#5865=LINE('',#31859,#7710);
#5866=LINE('',#31863,#7711);
#5867=LINE('',#31864,#7712);
#5868=LINE('',#31867,#7713);
#5869=LINE('',#31869,#7714);
#5870=LINE('',#31870,#7715);
#5871=LINE('',#31873,#7716);
#5872=LINE('',#31877,#7717);
#5873=LINE('',#31878,#7718);
#5874=LINE('',#31881,#7719);
#5875=LINE('',#31900,#7720);
#5876=LINE('',#31902,#7721);
#5877=LINE('',#31906,#7722);
#5878=LINE('',#31907,#7723);
#5879=LINE('',#31910,#7724);
#5880=LINE('',#31914,#7725);
#5881=LINE('',#31915,#7726);
#5882=LINE('',#31919,#7727);
#5883=LINE('',#31925,#7728);
#5884=LINE('',#31926,#7729);
#5885=LINE('',#31927,#7730);
#5886=LINE('',#31931,#7731);
#5887=LINE('',#31935,#7732);
#5888=LINE('',#31936,#7733);
#5889=LINE('',#31939,#7734);
#5890=LINE('',#31941,#7735);
#5891=LINE('',#31942,#7736);
#5892=LINE('',#31945,#7737);
#5893=LINE('',#31949,#7738);
#5894=LINE('',#31950,#7739);
#5895=LINE('',#31953,#7740);
#5896=LINE('',#31956,#7741);
#5897=LINE('',#31957,#7742);
#5898=LINE('',#31959,#7743);
#5899=LINE('',#31964,#7744);
#5900=LINE('',#31966,#7745);
#5901=LINE('',#31968,#7746);
#5902=LINE('',#31969,#7747);
#5903=LINE('',#31973,#7748);
#5904=LINE('',#31979,#7749);
#5905=LINE('',#31980,#7750);
#5906=LINE('',#31981,#7751);
#5907=LINE('',#31985,#7752);
#5908=LINE('',#31991,#7753);
#5909=LINE('',#31992,#7754);
#5910=LINE('',#31993,#7755);
#5911=LINE('',#31997,#7756);
#5912=LINE('',#32003,#7757);
#5913=LINE('',#32004,#7758);
#5914=LINE('',#32005,#7759);
#5915=LINE('',#32011,#7760);
#5916=LINE('',#32014,#7761);
#5917=LINE('',#32017,#7762);
#5918=LINE('',#32018,#7763);
#5919=LINE('',#32021,#7764);
#5920=LINE('',#32025,#7765);
#5921=LINE('',#32026,#7766);
#5922=LINE('',#32043,#7767);
#5923=LINE('',#32044,#7768);
#5924=LINE('',#32046,#7769);
#5925=LINE('',#32048,#7770);
#5926=LINE('',#32050,#7771);
#5927=LINE('',#32054,#7772);
#5928=LINE('',#32055,#7773);
#5929=LINE('',#32056,#7774);
#5930=LINE('',#32060,#7775);
#5931=LINE('',#32066,#7776);
#5932=LINE('',#32067,#7777);
#5933=LINE('',#32068,#7778);
#5934=LINE('',#32073,#7779);
#5935=LINE('',#32074,#7780);
#5936=LINE('',#32076,#7781);
#5937=LINE('',#32080,#7782);
#5938=LINE('',#32087,#7783);
#5939=LINE('',#32090,#7784);
#5940=LINE('',#32097,#7785);
#5941=LINE('',#32100,#7786);
#5942=LINE('',#32107,#7787);
#5943=LINE('',#32110,#7788);
#5944=LINE('',#32117,#7789);
#5945=LINE('',#32120,#7790);
#5946=LINE('',#32127,#7791);
#5947=LINE('',#32130,#7792);
#5948=LINE('',#32137,#7793);
#5949=LINE('',#32140,#7794);
#5950=LINE('',#32147,#7795);
#5951=LINE('',#32150,#7796);
#5952=LINE('',#32154,#7797);
#5953=LINE('',#32158,#7798);
#5954=LINE('',#32163,#7799);
#5955=LINE('',#32167,#7800);
#5956=LINE('',#32171,#7801);
#5957=LINE('',#32176,#7802);
#5958=LINE('',#32180,#7803);
#5959=LINE('',#32184,#7804);
#5960=LINE('',#32189,#7805);
#5961=LINE('',#32193,#7806);
#5962=LINE('',#32197,#7807);
#5963=LINE('',#32202,#7808);
#5964=LINE('',#32206,#7809);
#5965=LINE('',#32210,#7810);
#5966=LINE('',#32215,#7811);
#5967=LINE('',#32219,#7812);
#5968=LINE('',#32223,#7813);
#5969=LINE('',#32228,#7814);
#5970=LINE('',#32232,#7815);
#5971=LINE('',#32236,#7816);
#5972=LINE('',#32242,#7817);
#5973=LINE('',#32244,#7818);
#5974=LINE('',#32246,#7819);
#5975=LINE('',#32252,#7820);
#5976=LINE('',#32254,#7821);
#5977=LINE('',#32256,#7822);
#5978=LINE('',#32257,#7823);
#5979=LINE('',#32260,#7824);
#5980=LINE('',#32262,#7825);
#5981=LINE('',#32263,#7826);
#5982=LINE('',#32267,#7827);
#5983=LINE('',#32273,#7828);
#5984=LINE('',#32274,#7829);
#5985=LINE('',#32275,#7830);
#5986=LINE('',#32279,#7831);
#5987=LINE('',#32283,#7832);
#5988=LINE('',#32284,#7833);
#5989=LINE('',#32287,#7834);
#5990=LINE('',#32290,#7835);
#5991=LINE('',#32293,#7836);
#5992=LINE('',#32294,#7837);
#5993=LINE('',#32297,#7838);
#5994=LINE('',#32298,#7839);
#5995=LINE('',#32316,#7840);
#5996=LINE('',#32318,#7841);
#5997=LINE('',#32320,#7842);
#5998=LINE('',#32322,#7843);
#5999=LINE('',#32323,#7844);
#6000=LINE('',#32326,#7845);
#6001=LINE('',#32328,#7846);
#6002=LINE('',#32329,#7847);
#6003=LINE('',#32338,#7848);
#6004=LINE('',#32340,#7849);
#6005=LINE('',#32342,#7850);
#6006=LINE('',#32343,#7851);
#6007=LINE('',#32346,#7852);
#6008=LINE('',#32348,#7853);
#6009=LINE('',#32349,#7854);
#6010=LINE('',#32352,#7855);
#6011=LINE('',#32354,#7856);
#6012=LINE('',#32355,#7857);
#6013=LINE('',#32358,#7858);
#6014=LINE('',#32363,#7859);
#6015=LINE('',#32364,#7860);
#6016=LINE('',#32365,#7861);
#6017=LINE('',#32370,#7862);
#6018=LINE('',#32372,#7863);
#6019=LINE('',#32376,#7864);
#6020=LINE('',#32378,#7865);
#6021=LINE('',#32380,#7866);
#6022=LINE('',#32381,#7867);
#6023=LINE('',#32384,#7868);
#6024=LINE('',#32385,#7869);
#6025=LINE('',#32388,#7870);
#6026=LINE('',#32389,#7871);
#6027=LINE('',#32392,#7872);
#6028=LINE('',#32393,#7873);
#6029=LINE('',#32396,#7874);
#6030=LINE('',#32398,#7875);
#6031=LINE('',#32399,#7876);
#6032=LINE('',#32403,#7877);
#6033=LINE('',#32409,#7878);
#6034=LINE('',#32410,#7879);
#6035=LINE('',#32411,#7880);
#6036=LINE('',#32417,#7881);
#6037=LINE('',#32420,#7882);
#6038=LINE('',#32423,#7883);
#6039=LINE('',#32424,#7884);
#6040=LINE('',#32427,#7885);
#6041=LINE('',#32428,#7886);
#6042=LINE('',#32430,#7887);
#6043=LINE('',#32431,#7888);
#6044=LINE('',#32436,#7889);
#6045=LINE('',#32437,#7890);
#6046=LINE('',#32438,#7891);
#6047=LINE('',#32441,#7892);
#6048=LINE('',#32442,#7893);
#6049=LINE('',#32445,#7894);
#6050=LINE('',#32450,#7895);
#6051=LINE('',#32451,#7896);
#6052=LINE('',#32452,#7897);
#6053=LINE('',#32456,#7898);
#6054=LINE('',#32460,#7899);
#6055=LINE('',#32461,#7900);
#6056=LINE('',#32463,#7901);
#6057=LINE('',#32464,#7902);
#6058=LINE('',#32489,#7903);
#6059=LINE('',#32493,#7904);
#6060=LINE('',#32497,#7905);
#6061=LINE('',#32504,#7906);
#6062=LINE('',#32507,#7907);
#6063=LINE('',#32512,#7908);
#6064=LINE('',#32519,#7909);
#6065=LINE('',#32521,#7910);
#6066=LINE('',#32524,#7911);
#6067=LINE('',#32531,#7912);
#6068=LINE('',#32533,#7913);
#6069=LINE('',#32536,#7914);
#6070=LINE('',#32543,#7915);
#6071=LINE('',#32545,#7916);
#6072=LINE('',#32548,#7917);
#6073=LINE('',#32552,#7918);
#6074=LINE('',#32556,#7919);
#6075=LINE('',#32560,#7920);
#6076=LINE('',#32564,#7921);
#6077=LINE('',#32568,#7922);
#6078=LINE('',#32574,#7923);
#6079=LINE('',#32581,#7924);
#6080=LINE('',#32583,#7925);
#6081=LINE('',#32589,#7926);
#6082=LINE('',#32593,#7927);
#6083=LINE('',#32596,#7928);
#6084=LINE('',#32600,#7929);
#6085=LINE('',#32604,#7930);
#6086=LINE('',#32607,#7931);
#6087=LINE('',#32611,#7932);
#6088=LINE('',#32615,#7933);
#6089=LINE('',#32618,#7934);
#6090=LINE('',#32622,#7935);
#6091=LINE('',#32626,#7936);
#6092=LINE('',#32629,#7937);
#6093=LINE('',#32631,#7938);
#6094=LINE('',#32633,#7939);
#6095=LINE('',#32635,#7940);
#6096=LINE('',#32639,#7941);
#6097=LINE('',#32643,#7942);
#6098=LINE('',#32646,#7943);
#6099=LINE('',#32650,#7944);
#6100=LINE('',#32654,#7945);
#6101=LINE('',#32657,#7946);
#6102=LINE('',#32661,#7947);
#6103=LINE('',#32665,#7948);
#6104=LINE('',#32668,#7949);
#6105=LINE('',#32675,#7950);
#6106=LINE('',#32679,#7951);
#6107=LINE('',#32684,#7952);
#6108=LINE('',#32685,#7953);
#6109=LINE('',#32686,#7954);
#6110=LINE('',#32690,#7955);
#6111=LINE('',#32696,#7956);
#6112=LINE('',#32697,#7957);
#6113=LINE('',#32698,#7958);
#6114=LINE('',#32702,#7959);
#6115=LINE('',#32708,#7960);
#6116=LINE('',#32709,#7961);
#6117=LINE('',#32710,#7962);
#6118=LINE('',#32714,#7963);
#6119=LINE('',#32718,#7964);
#6120=LINE('',#32719,#7965);
#6121=LINE('',#32722,#7966);
#6122=LINE('',#32724,#7967);
#6123=LINE('',#32725,#7968);
#6124=LINE('',#32728,#7969);
#6125=LINE('',#32732,#7970);
#6126=LINE('',#32733,#7971);
#6127=LINE('',#32736,#7972);
#6128=LINE('',#32750,#7973);
#6129=LINE('',#32752,#7974);
#6130=LINE('',#32754,#7975);
#6131=LINE('',#32755,#7976);
#6132=LINE('',#32759,#7977);
#6133=LINE('',#32764,#7978);
#6134=LINE('',#32765,#7979);
#6135=LINE('',#32766,#7980);
#6136=LINE('',#32769,#7981);
#6137=LINE('',#32773,#7982);
#6138=LINE('',#32774,#7983);
#6139=LINE('',#32777,#7984);
#6140=LINE('',#32781,#7985);
#6141=LINE('',#32782,#7986);
#6142=LINE('',#32788,#7987);
#6143=LINE('',#32791,#7988);
#6144=LINE('',#32794,#7989);
#6145=LINE('',#32795,#7990);
#6146=LINE('',#32798,#7991);
#6147=LINE('',#32802,#7992);
#6148=LINE('',#32803,#7993);
#6149=LINE('',#32805,#7994);
#6150=LINE('',#32807,#7995);
#6151=LINE('',#32810,#7996);
#6152=LINE('',#32813,#7997);
#6153=LINE('',#32816,#7998);
#6154=LINE('',#32817,#7999);
#6155=LINE('',#32820,#8000);
#6156=LINE('',#32824,#8001);
#6157=LINE('',#32825,#8002);
#6158=LINE('',#32829,#8003);
#6159=LINE('',#32835,#8004);
#6160=LINE('',#32836,#8005);
#6161=LINE('',#32837,#8006);
#6162=LINE('',#32841,#8007);
#6163=LINE('',#32845,#8008);
#6164=LINE('',#32846,#8009);
#6165=LINE('',#32849,#8010);
#6166=LINE('',#32851,#8011);
#6167=LINE('',#32852,#8012);
#6168=LINE('',#32855,#8013);
#6169=LINE('',#32859,#8014);
#6170=LINE('',#32860,#8015);
#6171=LINE('',#32863,#8016);
#6172=LINE('',#32867,#8017);
#6173=LINE('',#32874,#8018);
#6174=LINE('',#32877,#8019);
#6175=LINE('',#32879,#8020);
#6176=LINE('',#32883,#8021);
#6177=LINE('',#32884,#8022);
#6178=LINE('',#32887,#8023);
#6179=LINE('',#32891,#8024);
#6180=LINE('',#32892,#8025);
#6181=LINE('',#32896,#8026);
#6182=LINE('',#32902,#8027);
#6183=LINE('',#32903,#8028);
#6184=LINE('',#32904,#8029);
#6185=LINE('',#32908,#8030);
#6186=LINE('',#32912,#8031);
#6187=LINE('',#32913,#8032);
#6188=LINE('',#32915,#8033);
#6189=LINE('',#32916,#8034);
#6190=LINE('',#32918,#8035);
#6191=LINE('',#32927,#8036);
#6192=LINE('',#32932,#8037);
#6193=LINE('',#32937,#8038);
#6194=LINE('',#32940,#8039);
#6195=LINE('',#32943,#8040);
#6196=LINE('',#32947,#8041);
#6197=LINE('',#32951,#8042);
#6198=LINE('',#32954,#8043);
#6199=LINE('',#32958,#8044);
#6200=LINE('',#32962,#8045);
#6201=LINE('',#32965,#8046);
#6202=LINE('',#32969,#8047);
#6203=LINE('',#32973,#8048);
#6204=LINE('',#32976,#8049);
#6205=LINE('',#32979,#8050);
#6206=LINE('',#32982,#8051);
#6207=LINE('',#32983,#8052);
#6208=LINE('',#32985,#8053);
#6209=LINE('',#32993,#8054);
#6210=LINE('',#32999,#8055);
#6211=LINE('',#33005,#8056);
#6212=LINE('',#33010,#8057);
#6213=LINE('',#33014,#8058);
#6214=LINE('',#33017,#8059);
#6215=LINE('',#33031,#8060);
#6216=LINE('',#33035,#8061);
#6217=LINE('',#33038,#8062);
#6218=LINE('',#33045,#8063);
#6219=LINE('',#33054,#8064);
#6220=LINE('',#33058,#8065);
#6221=LINE('',#33061,#8066);
#6222=LINE('',#33064,#8067);
#6223=LINE('',#33068,#8068);
#6224=LINE('',#33072,#8069);
#6225=LINE('',#33075,#8070);
#6226=LINE('',#33079,#8071);
#6227=LINE('',#33083,#8072);
#6228=LINE('',#33086,#8073);
#6229=LINE('',#33090,#8074);
#6230=LINE('',#33094,#8075);
#6231=LINE('',#33097,#8076);
#6232=LINE('',#33103,#8077);
#6233=LINE('',#33110,#8078);
#6234=LINE('',#33129,#8079);
#6235=LINE('',#33147,#8080);
#6236=LINE('',#33154,#8081);
#6237=LINE('',#33156,#8082);
#6238=LINE('',#33159,#8083);
#6239=LINE('',#33166,#8084);
#6240=LINE('',#33168,#8085);
#6241=LINE('',#33171,#8086);
#6242=LINE('',#33178,#8087);
#6243=LINE('',#33180,#8088);
#6244=LINE('',#33183,#8089);
#6245=LINE('',#33190,#8090);
#6246=LINE('',#33192,#8091);
#6247=LINE('',#33195,#8092);
#6248=LINE('',#33202,#8093);
#6249=LINE('',#33204,#8094);
#6250=LINE('',#33207,#8095);
#6251=LINE('',#33213,#8096);
#6252=LINE('',#33218,#8097);
#6253=LINE('',#33221,#8098);
#6254=LINE('',#33230,#8099);
#6255=LINE('',#33232,#8100);
#6256=LINE('',#33237,#8101);
#6257=LINE('',#33265,#8102);
#6258=LINE('',#33299,#8103);
#6259=LINE('',#33347,#8104);
#6260=LINE('',#33395,#8105);
#6261=LINE('',#33443,#8106);
#6262=LINE('',#33491,#8107);
#6263=LINE('',#33545,#8108);
#6264=LINE('',#33593,#8109);
#6265=LINE('',#33641,#8110);
#6266=LINE('',#33695,#8111);
#6267=LINE('',#33743,#8112);
#6268=LINE('',#33759,#8113);
#6269=LINE('',#33783,#8114);
#6270=LINE('',#33808,#8115);
#6271=LINE('',#33833,#8116);
#6272=LINE('',#33857,#8117);
#6273=LINE('',#33882,#8118);
#6274=LINE('',#33907,#8119);
#6275=LINE('',#33931,#8120);
#6276=LINE('',#33957,#8121);
#6277=LINE('',#33981,#8122);
#6278=LINE('',#34891,#8123);
#6279=LINE('',#34897,#8124);
#6280=LINE('',#34903,#8125);
#6281=LINE('',#34909,#8126);
#6282=LINE('',#34914,#8127);
#6283=LINE('',#34916,#8128);
#6284=LINE('',#34918,#8129);
#6285=LINE('',#34919,#8130);
#6286=LINE('',#34923,#8131);
#6287=LINE('',#34926,#8132);
#6288=LINE('',#34927,#8133);
#6289=LINE('',#34933,#8134);
#6290=LINE('',#34935,#8135);
#6291=LINE('',#34937,#8136);
#6292=LINE('',#34938,#8137);
#6293=LINE('',#34942,#8138);
#6294=LINE('',#34945,#8139);
#6295=LINE('',#34946,#8140);
#6296=LINE('',#34952,#8141);
#6297=LINE('',#34954,#8142);
#6298=LINE('',#34956,#8143);
#6299=LINE('',#34957,#8144);
#6300=LINE('',#34961,#8145);
#6301=LINE('',#34964,#8146);
#6302=LINE('',#34965,#8147);
#6303=LINE('',#34971,#8148);
#6304=LINE('',#34973,#8149);
#6305=LINE('',#34975,#8150);
#6306=LINE('',#34976,#8151);
#6307=LINE('',#34980,#8152);
#6308=LINE('',#34983,#8153);
#6309=LINE('',#34984,#8154);
#6310=LINE('',#34990,#8155);
#6311=LINE('',#34992,#8156);
#6312=LINE('',#34994,#8157);
#6313=LINE('',#34995,#8158);
#6314=LINE('',#34999,#8159);
#6315=LINE('',#35002,#8160);
#6316=LINE('',#35003,#8161);
#6317=LINE('',#35009,#8162);
#6318=LINE('',#35011,#8163);
#6319=LINE('',#35013,#8164);
#6320=LINE('',#35014,#8165);
#6321=LINE('',#35018,#8166);
#6322=LINE('',#35021,#8167);
#6323=LINE('',#35022,#8168);
#6324=LINE('',#35028,#8169);
#6325=LINE('',#35030,#8170);
#6326=LINE('',#35032,#8171);
#6327=LINE('',#35033,#8172);
#6328=LINE('',#35037,#8173);
#6329=LINE('',#35040,#8174);
#6330=LINE('',#35041,#8175);
#6331=LINE('',#35047,#8176);
#6332=LINE('',#35049,#8177);
#6333=LINE('',#35051,#8178);
#6334=LINE('',#35052,#8179);
#6335=LINE('',#35056,#8180);
#6336=LINE('',#35059,#8181);
#6337=LINE('',#35060,#8182);
#6338=LINE('',#35066,#8183);
#6339=LINE('',#35068,#8184);
#6340=LINE('',#35070,#8185);
#6341=LINE('',#35071,#8186);
#6342=LINE('',#35075,#8187);
#6343=LINE('',#35078,#8188);
#6344=LINE('',#35079,#8189);
#6345=LINE('',#35085,#8190);
#6346=LINE('',#35087,#8191);
#6347=LINE('',#35089,#8192);
#6348=LINE('',#35090,#8193);
#6349=LINE('',#35094,#8194);
#6350=LINE('',#35097,#8195);
#6351=LINE('',#35098,#8196);
#6352=LINE('',#35104,#8197);
#6353=LINE('',#35106,#8198);
#6354=LINE('',#35108,#8199);
#6355=LINE('',#35109,#8200);
#6356=LINE('',#35113,#8201);
#6357=LINE('',#35116,#8202);
#6358=LINE('',#35117,#8203);
#6359=LINE('',#35123,#8204);
#6360=LINE('',#35125,#8205);
#6361=LINE('',#35127,#8206);
#6362=LINE('',#35128,#8207);
#6363=LINE('',#35133,#8208);
#6364=LINE('',#35137,#8209);
#6365=LINE('',#35138,#8210);
#6366=LINE('',#35146,#8211);
#6367=LINE('',#35148,#8212);
#6368=LINE('',#35150,#8213);
#6369=LINE('',#35151,#8214);
#6370=LINE('',#35155,#8215);
#6371=LINE('',#35158,#8216);
#6372=LINE('',#35159,#8217);
#6373=LINE('',#35165,#8218);
#6374=LINE('',#35167,#8219);
#6375=LINE('',#35169,#8220);
#6376=LINE('',#35170,#8221);
#6377=LINE('',#35174,#8222);
#6378=LINE('',#35177,#8223);
#6379=LINE('',#35178,#8224);
#6380=LINE('',#35184,#8225);
#6381=LINE('',#35186,#8226);
#6382=LINE('',#35188,#8227);
#6383=LINE('',#35189,#8228);
#6384=LINE('',#35193,#8229);
#6385=LINE('',#35196,#8230);
#6386=LINE('',#35197,#8231);
#6387=LINE('',#35203,#8232);
#6388=LINE('',#35205,#8233);
#6389=LINE('',#35207,#8234);
#6390=LINE('',#35208,#8235);
#6391=LINE('',#35212,#8236);
#6392=LINE('',#35215,#8237);
#6393=LINE('',#35216,#8238);
#6394=LINE('',#35222,#8239);
#6395=LINE('',#35224,#8240);
#6396=LINE('',#35226,#8241);
#6397=LINE('',#35227,#8242);
#6398=LINE('',#35231,#8243);
#6399=LINE('',#35234,#8244);
#6400=LINE('',#35235,#8245);
#6401=LINE('',#35241,#8246);
#6402=LINE('',#35243,#8247);
#6403=LINE('',#35245,#8248);
#6404=LINE('',#35246,#8249);
#6405=LINE('',#35250,#8250);
#6406=LINE('',#35253,#8251);
#6407=LINE('',#35254,#8252);
#6408=LINE('',#35260,#8253);
#6409=LINE('',#35262,#8254);
#6410=LINE('',#35264,#8255);
#6411=LINE('',#35265,#8256);
#6412=LINE('',#35269,#8257);
#6413=LINE('',#35272,#8258);
#6414=LINE('',#35273,#8259);
#6415=LINE('',#35279,#8260);
#6416=LINE('',#35281,#8261);
#6417=LINE('',#35283,#8262);
#6418=LINE('',#35284,#8263);
#6419=LINE('',#35288,#8264);
#6420=LINE('',#35291,#8265);
#6421=LINE('',#35292,#8266);
#6422=LINE('',#35298,#8267);
#6423=LINE('',#35300,#8268);
#6424=LINE('',#35302,#8269);
#6425=LINE('',#35303,#8270);
#6426=LINE('',#35307,#8271);
#6427=LINE('',#35310,#8272);
#6428=LINE('',#35311,#8273);
#6429=LINE('',#35317,#8274);
#6430=LINE('',#35319,#8275);
#6431=LINE('',#35321,#8276);
#6432=LINE('',#35322,#8277);
#6433=LINE('',#35326,#8278);
#6434=LINE('',#35329,#8279);
#6435=LINE('',#35330,#8280);
#6436=LINE('',#35336,#8281);
#6437=LINE('',#35338,#8282);
#6438=LINE('',#35340,#8283);
#6439=LINE('',#35341,#8284);
#6440=LINE('',#35345,#8285);
#6441=LINE('',#35348,#8286);
#6442=LINE('',#35349,#8287);
#6443=LINE('',#35355,#8288);
#6444=LINE('',#35357,#8289);
#6445=LINE('',#35359,#8290);
#6446=LINE('',#35360,#8291);
#6447=LINE('',#35364,#8292);
#6448=LINE('',#35367,#8293);
#6449=LINE('',#35368,#8294);
#6450=LINE('',#35375,#8295);
#6451=LINE('',#35380,#8296);
#6452=LINE('',#35387,#8297);
#6453=LINE('',#35392,#8298);
#6454=LINE('',#35394,#8299);
#6455=LINE('',#35402,#8300);
#6456=LINE('',#35406,#8301);
#6457=LINE('',#35411,#8302);
#6458=LINE('',#35413,#8303);
#6459=LINE('',#35415,#8304);
#6460=LINE('',#35416,#8305);
#6461=LINE('',#35419,#8306);
#6462=LINE('',#35421,#8307);
#6463=LINE('',#35422,#8308);
#6464=LINE('',#35425,#8309);
#6465=LINE('',#35427,#8310);
#6466=LINE('',#35428,#8311);
#6467=LINE('',#35431,#8312);
#6468=LINE('',#35433,#8313);
#6469=LINE('',#35434,#8314);
#6470=LINE('',#35437,#8315);
#6471=LINE('',#35439,#8316);
#6472=LINE('',#35440,#8317);
#6473=LINE('',#35442,#8318);
#6474=LINE('',#35443,#8319);
#6475=LINE('',#35448,#8320);
#6476=LINE('',#35450,#8321);
#6477=LINE('',#35452,#8322);
#6478=LINE('',#35453,#8323);
#6479=LINE('',#35457,#8324);
#6480=LINE('',#35459,#8325);
#6481=LINE('',#35460,#8326);
#6482=LINE('',#35463,#8327);
#6483=LINE('',#35464,#8328);
#6484=LINE('',#35467,#8329);
#6485=LINE('',#35468,#8330);
#6486=LINE('',#35470,#8331);
#6487=LINE('',#35476,#8332);
#6488=LINE('',#35483,#8333);
#6489=LINE('',#35489,#8334);
#6490=LINE('',#35496,#8335);
#6491=LINE('',#35504,#8336);
#6492=LINE('',#35517,#8337);
#6493=LINE('',#35522,#8338);
#6494=LINE('',#35531,#8339);
#6495=LINE('',#35535,#8340);
#6496=LINE('',#35538,#8341);
#6497=LINE('',#35547,#8342);
#6498=LINE('',#35553,#8343);
#6499=LINE('',#35561,#8344);
#6500=LINE('',#35567,#8345);
#6501=LINE('',#35574,#8346);
#6502=LINE('',#35577,#8347);
#6503=LINE('',#35585,#8348);
#6504=LINE('',#35587,#8349);
#6505=LINE('',#35589,#8350);
#6506=LINE('',#35590,#8351);
#6507=LINE('',#35594,#8352);
#6508=LINE('',#35597,#8353);
#6509=LINE('',#35598,#8354);
#6510=LINE('',#35604,#8355);
#6511=LINE('',#35606,#8356);
#6512=LINE('',#35608,#8357);
#6513=LINE('',#35609,#8358);
#6514=LINE('',#35613,#8359);
#6515=LINE('',#35616,#8360);
#6516=LINE('',#35617,#8361);
#6517=LINE('',#35623,#8362);
#6518=LINE('',#35625,#8363);
#6519=LINE('',#35627,#8364);
#6520=LINE('',#35628,#8365);
#6521=LINE('',#35632,#8366);
#6522=LINE('',#35635,#8367);
#6523=LINE('',#35636,#8368);
#6524=LINE('',#35642,#8369);
#6525=LINE('',#35644,#8370);
#6526=LINE('',#35646,#8371);
#6527=LINE('',#35647,#8372);
#6528=LINE('',#35651,#8373);
#6529=LINE('',#35654,#8374);
#6530=LINE('',#35655,#8375);
#6531=LINE('',#35661,#8376);
#6532=LINE('',#35663,#8377);
#6533=LINE('',#35665,#8378);
#6534=LINE('',#35666,#8379);
#6535=LINE('',#35670,#8380);
#6536=LINE('',#35673,#8381);
#6537=LINE('',#35674,#8382);
#6538=LINE('',#35680,#8383);
#6539=LINE('',#35682,#8384);
#6540=LINE('',#35684,#8385);
#6541=LINE('',#35685,#8386);
#6542=LINE('',#35689,#8387);
#6543=LINE('',#35692,#8388);
#6544=LINE('',#35693,#8389);
#6545=LINE('',#35699,#8390);
#6546=LINE('',#35701,#8391);
#6547=LINE('',#35703,#8392);
#6548=LINE('',#35704,#8393);
#6549=LINE('',#35708,#8394);
#6550=LINE('',#35711,#8395);
#6551=LINE('',#35712,#8396);
#6552=LINE('',#35718,#8397);
#6553=LINE('',#35720,#8398);
#6554=LINE('',#35722,#8399);
#6555=LINE('',#35723,#8400);
#6556=LINE('',#35727,#8401);
#6557=LINE('',#35730,#8402);
#6558=LINE('',#35731,#8403);
#6559=LINE('',#35737,#8404);
#6560=LINE('',#35739,#8405);
#6561=LINE('',#35741,#8406);
#6562=LINE('',#35742,#8407);
#6563=LINE('',#35747,#8408);
#6564=LINE('',#35751,#8409);
#6565=LINE('',#35752,#8410);
#6566=LINE('',#35760,#8411);
#6567=LINE('',#35762,#8412);
#6568=LINE('',#35764,#8413);
#6569=LINE('',#35765,#8414);
#6570=LINE('',#35769,#8415);
#6571=LINE('',#35772,#8416);
#6572=LINE('',#35773,#8417);
#6573=LINE('',#35779,#8418);
#6574=LINE('',#35781,#8419);
#6575=LINE('',#35783,#8420);
#6576=LINE('',#35784,#8421);
#6577=LINE('',#35788,#8422);
#6578=LINE('',#35791,#8423);
#6579=LINE('',#35792,#8424);
#6580=LINE('',#35798,#8425);
#6581=LINE('',#35800,#8426);
#6582=LINE('',#35802,#8427);
#6583=LINE('',#35803,#8428);
#6584=LINE('',#35807,#8429);
#6585=LINE('',#35810,#8430);
#6586=LINE('',#35811,#8431);
#6587=LINE('',#35817,#8432);
#6588=LINE('',#35819,#8433);
#6589=LINE('',#35821,#8434);
#6590=LINE('',#35822,#8435);
#6591=LINE('',#35826,#8436);
#6592=LINE('',#35829,#8437);
#6593=LINE('',#35830,#8438);
#6594=LINE('',#35836,#8439);
#6595=LINE('',#35838,#8440);
#6596=LINE('',#35840,#8441);
#6597=LINE('',#35841,#8442);
#6598=LINE('',#35845,#8443);
#6599=LINE('',#35848,#8444);
#6600=LINE('',#35849,#8445);
#6601=LINE('',#35855,#8446);
#6602=LINE('',#35857,#8447);
#6603=LINE('',#35859,#8448);
#6604=LINE('',#35860,#8449);
#6605=LINE('',#35864,#8450);
#6606=LINE('',#35867,#8451);
#6607=LINE('',#35868,#8452);
#6608=LINE('',#35874,#8453);
#6609=LINE('',#35876,#8454);
#6610=LINE('',#35878,#8455);
#6611=LINE('',#35879,#8456);
#6612=LINE('',#35883,#8457);
#6613=LINE('',#35886,#8458);
#6614=LINE('',#35887,#8459);
#6615=LINE('',#35893,#8460);
#6616=LINE('',#35895,#8461);
#6617=LINE('',#35897,#8462);
#6618=LINE('',#35898,#8463);
#6619=LINE('',#35902,#8464);
#6620=LINE('',#35905,#8465);
#6621=LINE('',#35906,#8466);
#6622=LINE('',#35912,#8467);
#6623=LINE('',#35914,#8468);
#6624=LINE('',#35916,#8469);
#6625=LINE('',#35917,#8470);
#6626=LINE('',#35921,#8471);
#6627=LINE('',#35924,#8472);
#6628=LINE('',#35925,#8473);
#6629=LINE('',#35932,#8474);
#6630=LINE('',#35938,#8475);
#6631=LINE('',#35948,#8476);
#6632=LINE('',#35950,#8477);
#6633=LINE('',#35957,#8478);
#6634=LINE('',#35958,#8479);
#6635=LINE('',#35965,#8480);
#6636=LINE('',#35972,#8481);
#6637=LINE('',#35980,#8482);
#6638=LINE('',#35987,#8483);
#6639=LINE('',#35991,#8484);
#6640=LINE('',#35998,#8485);
#6641=LINE('',#36002,#8486);
#6642=LINE('',#36006,#8487);
#6643=LINE('',#36007,#8488);
#6644=LINE('',#36011,#8489);
#6645=LINE('',#36017,#8490);
#6646=LINE('',#36021,#8491);
#6647=LINE('',#36025,#8492);
#6648=LINE('',#36028,#8493);
#6649=LINE('',#36031,#8494);
#6650=LINE('',#36033,#8495);
#6651=LINE('',#36034,#8496);
#6652=LINE('',#36037,#8497);
#6653=LINE('',#36041,#8498);
#6654=LINE('',#36042,#8499);
#6655=LINE('',#36045,#8500);
#6656=LINE('',#36049,#8501);
#6657=LINE('',#36050,#8502);
#6658=LINE('',#36054,#8503);
#6659=LINE('',#36056,#8504);
#6660=LINE('',#36058,#8505);
#6661=LINE('',#36059,#8506);
#6662=LINE('',#36062,#8507);
#6663=LINE('',#36064,#8508);
#6664=LINE('',#36065,#8509);
#6665=LINE('',#36069,#8510);
#6666=LINE('',#36075,#8511);
#6667=LINE('',#36076,#8512);
#6668=LINE('',#36077,#8513);
#6669=LINE('',#36081,#8514);
#6670=LINE('',#36085,#8515);
#6671=LINE('',#36086,#8516);
#6672=LINE('',#36089,#8517);
#6673=LINE('',#36092,#8518);
#6674=LINE('',#36095,#8519);
#6675=LINE('',#36096,#8520);
#6676=LINE('',#36097,#8521);
#6677=LINE('',#36099,#8522);
#6678=LINE('',#36103,#8523);
#6679=LINE('',#36106,#8524);
#6680=LINE('',#36109,#8525);
#6681=LINE('',#36110,#8526);
#6682=LINE('',#36113,#8527);
#6683=LINE('',#36117,#8528);
#6684=LINE('',#36118,#8529);
#6685=LINE('',#36120,#8530);
#6686=LINE('',#36123,#8531);
#6687=LINE('',#36125,#8532);
#6688=LINE('',#36127,#8533);
#6689=LINE('',#36129,#8534);
#6690=LINE('',#36131,#8535);
#6691=LINE('',#36133,#8536);
#6692=LINE('',#36135,#8537);
#6693=LINE('',#36137,#8538);
#6694=LINE('',#36144,#8539);
#6695=LINE('',#36148,#8540);
#6696=LINE('',#36153,#8541);
#6697=LINE('',#36155,#8542);
#6698=LINE('',#36160,#8543);
#6699=LINE('',#36178,#8544);
#6700=LINE('',#36195,#8545);
#6701=LINE('',#36243,#8546);
#6702=LINE('',#36297,#8547);
#6703=LINE('',#36345,#8548);
#6704=LINE('',#36393,#8549);
#6705=LINE('',#36441,#8550);
#6706=LINE('',#36495,#8551);
#6707=LINE('',#36543,#8552);
#6708=LINE('',#36591,#8553);
#6709=LINE('',#36645,#8554);
#6710=LINE('',#36693,#8555);
#6711=LINE('',#36741,#8556);
#6712=LINE('',#36795,#8557);
#6713=LINE('',#36843,#8558);
#6714=LINE('',#36861,#8559);
#6715=LINE('',#36885,#8560);
#6716=LINE('',#36910,#8561);
#6717=LINE('',#36935,#8562);
#6718=LINE('',#36959,#8563);
#6719=LINE('',#36984,#8564);
#6720=LINE('',#37009,#8565);
#6721=LINE('',#37033,#8566);
#6722=LINE('',#37058,#8567);
#6723=LINE('',#37083,#8568);
#6724=LINE('',#37107,#8569);
#6725=LINE('',#37131,#8570);
#6726=LINE('',#37156,#8571);
#6727=LINE('',#37181,#8572);
#6728=LINE('',#38221,#8573);
#6729=LINE('',#38226,#8574);
#6730=LINE('',#38228,#8575);
#6731=LINE('',#38230,#8576);
#6732=LINE('',#38231,#8577);
#6733=LINE('',#38235,#8578);
#6734=LINE('',#38238,#8579);
#6735=LINE('',#38239,#8580);
#6736=LINE('',#38245,#8581);
#6737=LINE('',#38247,#8582);
#6738=LINE('',#38249,#8583);
#6739=LINE('',#38250,#8584);
#6740=LINE('',#38254,#8585);
#6741=LINE('',#38257,#8586);
#6742=LINE('',#38258,#8587);
#6743=LINE('',#38264,#8588);
#6744=LINE('',#38266,#8589);
#6745=LINE('',#38268,#8590);
#6746=LINE('',#38269,#8591);
#6747=LINE('',#38273,#8592);
#6748=LINE('',#38276,#8593);
#6749=LINE('',#38277,#8594);
#6750=LINE('',#38283,#8595);
#6751=LINE('',#38285,#8596);
#6752=LINE('',#38287,#8597);
#6753=LINE('',#38288,#8598);
#6754=LINE('',#38292,#8599);
#6755=LINE('',#38295,#8600);
#6756=LINE('',#38296,#8601);
#6757=LINE('',#38302,#8602);
#6758=LINE('',#38304,#8603);
#6759=LINE('',#38306,#8604);
#6760=LINE('',#38307,#8605);
#6761=LINE('',#38311,#8606);
#6762=LINE('',#38314,#8607);
#6763=LINE('',#38315,#8608);
#6764=LINE('',#38321,#8609);
#6765=LINE('',#38323,#8610);
#6766=LINE('',#38325,#8611);
#6767=LINE('',#38326,#8612);
#6768=LINE('',#38330,#8613);
#6769=LINE('',#38333,#8614);
#6770=LINE('',#38334,#8615);
#6771=LINE('',#38340,#8616);
#6772=LINE('',#38342,#8617);
#6773=LINE('',#38344,#8618);
#6774=LINE('',#38345,#8619);
#6775=LINE('',#38349,#8620);
#6776=LINE('',#38352,#8621);
#6777=LINE('',#38353,#8622);
#6778=LINE('',#38359,#8623);
#6779=LINE('',#38361,#8624);
#6780=LINE('',#38363,#8625);
#6781=LINE('',#38364,#8626);
#6782=LINE('',#38368,#8627);
#6783=LINE('',#38371,#8628);
#6784=LINE('',#38372,#8629);
#6785=LINE('',#38378,#8630);
#6786=LINE('',#38380,#8631);
#6787=LINE('',#38382,#8632);
#6788=LINE('',#38383,#8633);
#6789=LINE('',#38387,#8634);
#6790=LINE('',#38390,#8635);
#6791=LINE('',#38391,#8636);
#6792=LINE('',#38397,#8637);
#6793=LINE('',#38399,#8638);
#6794=LINE('',#38401,#8639);
#6795=LINE('',#38402,#8640);
#6796=LINE('',#38406,#8641);
#6797=LINE('',#38409,#8642);
#6798=LINE('',#38410,#8643);
#6799=LINE('',#38416,#8644);
#6800=LINE('',#38418,#8645);
#6801=LINE('',#38420,#8646);
#6802=LINE('',#38421,#8647);
#6803=LINE('',#38425,#8648);
#6804=LINE('',#38428,#8649);
#6805=LINE('',#38429,#8650);
#6806=LINE('',#38435,#8651);
#6807=LINE('',#38437,#8652);
#6808=LINE('',#38439,#8653);
#6809=LINE('',#38440,#8654);
#6810=LINE('',#38445,#8655);
#6811=LINE('',#38449,#8656);
#6812=LINE('',#38450,#8657);
#6813=LINE('',#38458,#8658);
#6814=LINE('',#38460,#8659);
#6815=LINE('',#38462,#8660);
#6816=LINE('',#38463,#8661);
#6817=LINE('',#38467,#8662);
#6818=LINE('',#38470,#8663);
#6819=LINE('',#38471,#8664);
#6820=LINE('',#38477,#8665);
#6821=LINE('',#38479,#8666);
#6822=LINE('',#38481,#8667);
#6823=LINE('',#38482,#8668);
#6824=LINE('',#38486,#8669);
#6825=LINE('',#38489,#8670);
#6826=LINE('',#38490,#8671);
#6827=LINE('',#38496,#8672);
#6828=LINE('',#38498,#8673);
#6829=LINE('',#38500,#8674);
#6830=LINE('',#38501,#8675);
#6831=LINE('',#38505,#8676);
#6832=LINE('',#38508,#8677);
#6833=LINE('',#38509,#8678);
#6834=LINE('',#38515,#8679);
#6835=LINE('',#38517,#8680);
#6836=LINE('',#38519,#8681);
#6837=LINE('',#38520,#8682);
#6838=LINE('',#38524,#8683);
#6839=LINE('',#38527,#8684);
#6840=LINE('',#38528,#8685);
#6841=LINE('',#38534,#8686);
#6842=LINE('',#38536,#8687);
#6843=LINE('',#38538,#8688);
#6844=LINE('',#38539,#8689);
#6845=LINE('',#38543,#8690);
#6846=LINE('',#38546,#8691);
#6847=LINE('',#38547,#8692);
#6848=LINE('',#38553,#8693);
#6849=LINE('',#38555,#8694);
#6850=LINE('',#38557,#8695);
#6851=LINE('',#38558,#8696);
#6852=LINE('',#38562,#8697);
#6853=LINE('',#38565,#8698);
#6854=LINE('',#38566,#8699);
#6855=LINE('',#38572,#8700);
#6856=LINE('',#38574,#8701);
#6857=LINE('',#38576,#8702);
#6858=LINE('',#38577,#8703);
#6859=LINE('',#38581,#8704);
#6860=LINE('',#38584,#8705);
#6861=LINE('',#38585,#8706);
#6862=LINE('',#38591,#8707);
#6863=LINE('',#38593,#8708);
#6864=LINE('',#38595,#8709);
#6865=LINE('',#38596,#8710);
#6866=LINE('',#38600,#8711);
#6867=LINE('',#38603,#8712);
#6868=LINE('',#38604,#8713);
#6869=LINE('',#38610,#8714);
#6870=LINE('',#38612,#8715);
#6871=LINE('',#38614,#8716);
#6872=LINE('',#38615,#8717);
#6873=LINE('',#38619,#8718);
#6874=LINE('',#38622,#8719);
#6875=LINE('',#38623,#8720);
#6876=LINE('',#38629,#8721);
#6877=LINE('',#38631,#8722);
#6878=LINE('',#38633,#8723);
#6879=LINE('',#38634,#8724);
#6880=LINE('',#38638,#8725);
#6881=LINE('',#38641,#8726);
#6882=LINE('',#38642,#8727);
#6883=LINE('',#38648,#8728);
#6884=LINE('',#38650,#8729);
#6885=LINE('',#38652,#8730);
#6886=LINE('',#38653,#8731);
#6887=LINE('',#38657,#8732);
#6888=LINE('',#38660,#8733);
#6889=LINE('',#38661,#8734);
#6890=LINE('',#38667,#8735);
#6891=LINE('',#38669,#8736);
#6892=LINE('',#38671,#8737);
#6893=LINE('',#38672,#8738);
#6894=LINE('',#38676,#8739);
#6895=LINE('',#38679,#8740);
#6896=LINE('',#38680,#8741);
#6897=LINE('',#38687,#8742);
#6898=LINE('',#38694,#8743);
#6899=LINE('',#38698,#8744);
#6900=LINE('',#38699,#8745);
#6901=LINE('',#38703,#8746);
#6902=LINE('',#38709,#8747);
#6903=LINE('',#38730,#8748);
#6904=LINE('',#38750,#8749);
#6905=LINE('',#38804,#8750);
#6906=LINE('',#38852,#8751);
#6907=LINE('',#38900,#8752);
#6908=LINE('',#38954,#8753);
#6909=LINE('',#39002,#8754);
#6910=LINE('',#39050,#8755);
#6911=LINE('',#39104,#8756);
#6912=LINE('',#39152,#8757);
#6913=LINE('',#39200,#8758);
#6914=LINE('',#39254,#8759);
#6915=LINE('',#39302,#8760);
#6916=LINE('',#39350,#8761);
#6917=LINE('',#39404,#8762);
#6918=LINE('',#39422,#8763);
#6919=LINE('',#39447,#8764);
#6920=LINE('',#39472,#8765);
#6921=LINE('',#39496,#8766);
#6922=LINE('',#39521,#8767);
#6923=LINE('',#39546,#8768);
#6924=LINE('',#39570,#8769);
#6925=LINE('',#39595,#8770);
#6926=LINE('',#39620,#8771);
#6927=LINE('',#39644,#8772);
#6928=LINE('',#39669,#8773);
#6929=LINE('',#39694,#8774);
#6930=LINE('',#39718,#8775);
#6931=LINE('',#39743,#8776);
#6932=LINE('',#40809,#8777);
#6933=LINE('',#40810,#8778);
#6934=LINE('',#40813,#8779);
#6935=LINE('',#40815,#8780);
#6936=LINE('',#40821,#8781);
#6937=LINE('',#40830,#8782);
#6938=LINE('',#40831,#8783);
#6939=LINE('',#40834,#8784);
#6940=LINE('',#40836,#8785);
#6941=LINE('',#40842,#8786);
#6942=LINE('',#40851,#8787);
#6943=LINE('',#40852,#8788);
#6944=LINE('',#40855,#8789);
#6945=LINE('',#40857,#8790);
#6946=LINE('',#40863,#8791);
#6947=LINE('',#40872,#8792);
#6948=LINE('',#40873,#8793);
#6949=LINE('',#40876,#8794);
#6950=LINE('',#40878,#8795);
#6951=LINE('',#40884,#8796);
#6952=LINE('',#40893,#8797);
#6953=LINE('',#40894,#8798);
#6954=LINE('',#40897,#8799);
#6955=LINE('',#40899,#8800);
#6956=LINE('',#40905,#8801);
#6957=LINE('',#40914,#8802);
#6958=LINE('',#40915,#8803);
#6959=LINE('',#40918,#8804);
#6960=LINE('',#40920,#8805);
#6961=LINE('',#40926,#8806);
#6962=LINE('',#40935,#8807);
#6963=LINE('',#40936,#8808);
#6964=LINE('',#40939,#8809);
#6965=LINE('',#40941,#8810);
#6966=LINE('',#40947,#8811);
#6967=LINE('',#40956,#8812);
#6968=LINE('',#40957,#8813);
#6969=LINE('',#40960,#8814);
#6970=LINE('',#40962,#8815);
#6971=LINE('',#40968,#8816);
#6972=LINE('',#40977,#8817);
#6973=LINE('',#40978,#8818);
#6974=LINE('',#40981,#8819);
#6975=LINE('',#40983,#8820);
#6976=LINE('',#40989,#8821);
#6977=LINE('',#40998,#8822);
#6978=LINE('',#40999,#8823);
#6979=LINE('',#41002,#8824);
#6980=LINE('',#41004,#8825);
#6981=LINE('',#41010,#8826);
#6982=LINE('',#41019,#8827);
#6983=LINE('',#41020,#8828);
#6984=LINE('',#41023,#8829);
#6985=LINE('',#41025,#8830);
#6986=LINE('',#41031,#8831);
#6987=LINE('',#41040,#8832);
#6988=LINE('',#41041,#8833);
#6989=LINE('',#41044,#8834);
#6990=LINE('',#41046,#8835);
#6991=LINE('',#41052,#8836);
#6992=LINE('',#41061,#8837);
#6993=LINE('',#41062,#8838);
#6994=LINE('',#41065,#8839);
#6995=LINE('',#41067,#8840);
#6996=LINE('',#41073,#8841);
#6997=LINE('',#41082,#8842);
#6998=LINE('',#41083,#8843);
#6999=LINE('',#41086,#8844);
#7000=LINE('',#41088,#8845);
#7001=LINE('',#41094,#8846);
#7002=LINE('',#41103,#8847);
#7003=LINE('',#41104,#8848);
#7004=LINE('',#41107,#8849);
#7005=LINE('',#41109,#8850);
#7006=LINE('',#41115,#8851);
#7007=LINE('',#41124,#8852);
#7008=LINE('',#41125,#8853);
#7009=LINE('',#41128,#8854);
#7010=LINE('',#41130,#8855);
#7011=LINE('',#41136,#8856);
#7012=LINE('',#41145,#8857);
#7013=LINE('',#41146,#8858);
#7014=LINE('',#41149,#8859);
#7015=LINE('',#41151,#8860);
#7016=LINE('',#41157,#8861);
#7017=LINE('',#41166,#8862);
#7018=LINE('',#41168,#8863);
#7019=LINE('',#41172,#8864);
#7020=LINE('',#41174,#8865);
#7021=LINE('',#41180,#8866);
#7022=LINE('',#41189,#8867);
#7023=LINE('',#41190,#8868);
#7024=LINE('',#41193,#8869);
#7025=LINE('',#41195,#8870);
#7026=LINE('',#41201,#8871);
#7027=LINE('',#41210,#8872);
#7028=LINE('',#41211,#8873);
#7029=LINE('',#41214,#8874);
#7030=LINE('',#41216,#8875);
#7031=LINE('',#41222,#8876);
#7032=LINE('',#41231,#8877);
#7033=LINE('',#41232,#8878);
#7034=LINE('',#41235,#8879);
#7035=LINE('',#41237,#8880);
#7036=LINE('',#41243,#8881);
#7037=LINE('',#41252,#8882);
#7038=LINE('',#41253,#8883);
#7039=LINE('',#41256,#8884);
#7040=LINE('',#41258,#8885);
#7041=LINE('',#41264,#8886);
#7042=LINE('',#41273,#8887);
#7043=LINE('',#41274,#8888);
#7044=LINE('',#41277,#8889);
#7045=LINE('',#41279,#8890);
#7046=LINE('',#41285,#8891);
#7047=LINE('',#41294,#8892);
#7048=LINE('',#41295,#8893);
#7049=LINE('',#41298,#8894);
#7050=LINE('',#41300,#8895);
#7051=LINE('',#41306,#8896);
#7052=LINE('',#41315,#8897);
#7053=LINE('',#41316,#8898);
#7054=LINE('',#41319,#8899);
#7055=LINE('',#41321,#8900);
#7056=LINE('',#41327,#8901);
#7057=LINE('',#41336,#8902);
#7058=LINE('',#41337,#8903);
#7059=LINE('',#41340,#8904);
#7060=LINE('',#41342,#8905);
#7061=LINE('',#41348,#8906);
#7062=LINE('',#41357,#8907);
#7063=LINE('',#41358,#8908);
#7064=LINE('',#41361,#8909);
#7065=LINE('',#41363,#8910);
#7066=LINE('',#41369,#8911);
#7067=LINE('',#41378,#8912);
#7068=LINE('',#41379,#8913);
#7069=LINE('',#41382,#8914);
#7070=LINE('',#41384,#8915);
#7071=LINE('',#41390,#8916);
#7072=LINE('',#41399,#8917);
#7073=LINE('',#41400,#8918);
#7074=LINE('',#41403,#8919);
#7075=LINE('',#41405,#8920);
#7076=LINE('',#41411,#8921);
#7077=LINE('',#41420,#8922);
#7078=LINE('',#41421,#8923);
#7079=LINE('',#41424,#8924);
#7080=LINE('',#41426,#8925);
#7081=LINE('',#41432,#8926);
#7082=LINE('',#41441,#8927);
#7083=LINE('',#41442,#8928);
#7084=LINE('',#41445,#8929);
#7085=LINE('',#41447,#8930);
#7086=LINE('',#41453,#8931);
#7087=LINE('',#41462,#8932);
#7088=LINE('',#41463,#8933);
#7089=LINE('',#41466,#8934);
#7090=LINE('',#41468,#8935);
#7091=LINE('',#41474,#8936);
#7092=LINE('',#41483,#8937);
#7093=LINE('',#41484,#8938);
#7094=LINE('',#41487,#8939);
#7095=LINE('',#41489,#8940);
#7096=LINE('',#41495,#8941);
#7097=LINE('',#41504,#8942);
#7098=LINE('',#41505,#8943);
#7099=LINE('',#41508,#8944);
#7100=LINE('',#41510,#8945);
#7101=LINE('',#41516,#8946);
#7102=LINE('',#41525,#8947);
#7103=LINE('',#41526,#8948);
#7104=LINE('',#41529,#8949);
#7105=LINE('',#41531,#8950);
#7106=LINE('',#41537,#8951);
#7107=LINE('',#41560,#8952);
#7108=LINE('',#41582,#8953);
#7109=LINE('',#41586,#8954);
#7110=LINE('',#41590,#8955);
#7111=LINE('',#41592,#8956);
#7112=LINE('',#41600,#8957);
#7113=LINE('',#41605,#8958);
#7114=LINE('',#41609,#8959);
#7115=LINE('',#41614,#8960);
#7116=LINE('',#41616,#8961);
#7117=LINE('',#41618,#8962);
#7118=LINE('',#41619,#8963);
#7119=LINE('',#41622,#8964);
#7120=LINE('',#41624,#8965);
#7121=LINE('',#41625,#8966);
#7122=LINE('',#41628,#8967);
#7123=LINE('',#41630,#8968);
#7124=LINE('',#41631,#8969);
#7125=LINE('',#41634,#8970);
#7126=LINE('',#41636,#8971);
#7127=LINE('',#41637,#8972);
#7128=LINE('',#41640,#8973);
#7129=LINE('',#41642,#8974);
#7130=LINE('',#41643,#8975);
#7131=LINE('',#41645,#8976);
#7132=LINE('',#41646,#8977);
#7133=LINE('',#41652,#8978);
#7134=LINE('',#41658,#8979);
#7135=LINE('',#41665,#8980);
#7136=LINE('',#41686,#8981);
#7137=LINE('',#41706,#8982);
#7138=LINE('',#41754,#8983);
#7139=LINE('',#41808,#8984);
#7140=LINE('',#41856,#8985);
#7141=LINE('',#41904,#8986);
#7142=LINE('',#41958,#8987);
#7143=LINE('',#42006,#8988);
#7144=LINE('',#42054,#8989);
#7145=LINE('',#42102,#8990);
#7146=LINE('',#42156,#8991);
#7147=LINE('',#42204,#8992);
#7148=LINE('',#42252,#8993);
#7149=LINE('',#42306,#8994);
#7150=LINE('',#42354,#8995);
#7151=LINE('',#42402,#8996);
#7152=LINE('',#42453,#8997);
#7153=LINE('',#42504,#8998);
#7154=LINE('',#42552,#8999);
#7155=LINE('',#42600,#9000);
#7156=LINE('',#42654,#9001);
#7157=LINE('',#42702,#9002);
#7158=LINE('',#42750,#9003);
#7159=LINE('',#42804,#9004);
#7160=LINE('',#42852,#9005);
#7161=LINE('',#42900,#9006);
#7162=LINE('',#42948,#9007);
#7163=LINE('',#43002,#9008);
#7164=LINE('',#43050,#9009);
#7165=LINE('',#43098,#9010);
#7166=LINE('',#43152,#9011);
#7167=LINE('',#43200,#9012);
#7168=LINE('',#43248,#9013);
#7169=LINE('',#43296,#9014);
#7170=LINE('',#43350,#9015);
#7171=LINE('',#43398,#9016);
#7172=LINE('',#43446,#9017);
#7173=LINE('',#43500,#9018);
#7174=LINE('',#43548,#9019);
#7175=LINE('',#43596,#9020);
#7176=LINE('',#43647,#9021);
#7177=LINE('',#43698,#9022);
#7178=LINE('',#43746,#9023);
#7179=LINE('',#43794,#9024);
#7180=LINE('',#43848,#9025);
#7181=LINE('',#43896,#9026);
#7182=LINE('',#43944,#9027);
#7183=LINE('',#43998,#9028);
#7184=LINE('',#44046,#9029);
#7185=LINE('',#44094,#9030);
#7186=LINE('',#44142,#9031);
#7187=LINE('',#44196,#9032);
#7188=LINE('',#44244,#9033);
#7189=LINE('',#44292,#9034);
#7190=LINE('',#44346,#9035);
#7191=LINE('',#44394,#9036);
#7192=LINE('',#44442,#9037);
#7193=LINE('',#44490,#9038);
#7194=LINE('',#44544,#9039);
#7195=LINE('',#44562,#9040);
#7196=LINE('',#44587,#9041);
#7197=LINE('',#44612,#9042);
#7198=LINE('',#44636,#9043);
#7199=LINE('',#44660,#9044);
#7200=LINE('',#44685,#9045);
#7201=LINE('',#44710,#9046);
#7202=LINE('',#44734,#9047);
#7203=LINE('',#44759,#9048);
#7204=LINE('',#44784,#9049);
#7205=LINE('',#44808,#9050);
#7206=LINE('',#44832,#9051);
#7207=LINE('',#44857,#9052);
#7208=LINE('',#44882,#9053);
#7209=LINE('',#44906,#9054);
#7210=LINE('',#44931,#9055);
#7211=LINE('',#44956,#9056);
#7212=LINE('',#44980,#9057);
#7213=LINE('',#45005,#9058);
#7214=LINE('',#45029,#9059);
#7215=LINE('',#45054,#9060);
#7216=LINE('',#45078,#9061);
#7217=LINE('',#45103,#9062);
#7218=LINE('',#45128,#9063);
#7219=LINE('',#45152,#9064);
#7220=LINE('',#45177,#9065);
#7221=LINE('',#45202,#9066);
#7222=LINE('',#45226,#9067);
#7223=LINE('',#45250,#9068);
#7224=LINE('',#45275,#9069);
#7225=LINE('',#45300,#9070);
#7226=LINE('',#45324,#9071);
#7227=LINE('',#45349,#9072);
#7228=LINE('',#45374,#9073);
#7229=LINE('',#45398,#9074);
#7230=LINE('',#45422,#9075);
#7231=LINE('',#45447,#9076);
#7232=LINE('',#45472,#9077);
#7233=LINE('',#45496,#9078);
#7234=LINE('',#45521,#9079);
#7235=LINE('',#45546,#9080);
#7236=LINE('',#45570,#9081);
#7237=LINE('',#45595,#9082);
#7238=LINE('',#45619,#9083);
#7239=LINE('',#45644,#9084);
#7240=LINE('',#45668,#9085);
#7241=LINE('',#45693,#9086);
#7242=LINE('',#45718,#9087);
#7243=LINE('',#45742,#9088);
#7244=LINE('',#45767,#9089);
#7245=LINE('',#45792,#9090);
#7246=LINE('',#45816,#9091);
#7247=LINE('',#45840,#9092);
#7248=LINE('',#45865,#9093);
#7249=LINE('',#45890,#9094);
#7250=LINE('',#45914,#9095);
#7251=LINE('',#45939,#9096);
#7252=LINE('',#45964,#9097);
#7253=LINE('',#49237,#9098);
#7254=LINE('',#49238,#9099);
#7255=LINE('',#49241,#9100);
#7256=LINE('',#49243,#9101);
#7257=LINE('',#49249,#9102);
#7258=LINE('',#49258,#9103);
#7259=LINE('',#49259,#9104);
#7260=LINE('',#49262,#9105);
#7261=LINE('',#49264,#9106);
#7262=LINE('',#49270,#9107);
#7263=LINE('',#49279,#9108);
#7264=LINE('',#49280,#9109);
#7265=LINE('',#49283,#9110);
#7266=LINE('',#49285,#9111);
#7267=LINE('',#49291,#9112);
#7268=LINE('',#49300,#9113);
#7269=LINE('',#49301,#9114);
#7270=LINE('',#49304,#9115);
#7271=LINE('',#49306,#9116);
#7272=LINE('',#49312,#9117);
#7273=LINE('',#49321,#9118);
#7274=LINE('',#49322,#9119);
#7275=LINE('',#49325,#9120);
#7276=LINE('',#49327,#9121);
#7277=LINE('',#49333,#9122);
#7278=LINE('',#49342,#9123);
#7279=LINE('',#49343,#9124);
#7280=LINE('',#49346,#9125);
#7281=LINE('',#49348,#9126);
#7282=LINE('',#49354,#9127);
#7283=LINE('',#49363,#9128);
#7284=LINE('',#49364,#9129);
#7285=LINE('',#49367,#9130);
#7286=LINE('',#49369,#9131);
#7287=LINE('',#49375,#9132);
#7288=LINE('',#49384,#9133);
#7289=LINE('',#49385,#9134);
#7290=LINE('',#49388,#9135);
#7291=LINE('',#49390,#9136);
#7292=LINE('',#49396,#9137);
#7293=LINE('',#49405,#9138);
#7294=LINE('',#49406,#9139);
#7295=LINE('',#49409,#9140);
#7296=LINE('',#49411,#9141);
#7297=LINE('',#49417,#9142);
#7298=LINE('',#49426,#9143);
#7299=LINE('',#49427,#9144);
#7300=LINE('',#49430,#9145);
#7301=LINE('',#49432,#9146);
#7302=LINE('',#49438,#9147);
#7303=LINE('',#49447,#9148);
#7304=LINE('',#49448,#9149);
#7305=LINE('',#49451,#9150);
#7306=LINE('',#49453,#9151);
#7307=LINE('',#49459,#9152);
#7308=LINE('',#49468,#9153);
#7309=LINE('',#49469,#9154);
#7310=LINE('',#49472,#9155);
#7311=LINE('',#49474,#9156);
#7312=LINE('',#49480,#9157);
#7313=LINE('',#49489,#9158);
#7314=LINE('',#49490,#9159);
#7315=LINE('',#49493,#9160);
#7316=LINE('',#49495,#9161);
#7317=LINE('',#49501,#9162);
#7318=LINE('',#49510,#9163);
#7319=LINE('',#49511,#9164);
#7320=LINE('',#49514,#9165);
#7321=LINE('',#49516,#9166);
#7322=LINE('',#49522,#9167);
#7323=LINE('',#49531,#9168);
#7324=LINE('',#49532,#9169);
#7325=LINE('',#49535,#9170);
#7326=LINE('',#49537,#9171);
#7327=LINE('',#49543,#9172);
#7328=LINE('',#49552,#9173);
#7329=LINE('',#49553,#9174);
#7330=LINE('',#49556,#9175);
#7331=LINE('',#49558,#9176);
#7332=LINE('',#49564,#9177);
#7333=LINE('',#49573,#9178);
#7334=LINE('',#49574,#9179);
#7335=LINE('',#49577,#9180);
#7336=LINE('',#49579,#9181);
#7337=LINE('',#49585,#9182);
#7338=LINE('',#49594,#9183);
#7339=LINE('',#49596,#9184);
#7340=LINE('',#49600,#9185);
#7341=LINE('',#49602,#9186);
#7342=LINE('',#49608,#9187);
#7343=LINE('',#49617,#9188);
#7344=LINE('',#49618,#9189);
#7345=LINE('',#49621,#9190);
#7346=LINE('',#49623,#9191);
#7347=LINE('',#49629,#9192);
#7348=LINE('',#49638,#9193);
#7349=LINE('',#49639,#9194);
#7350=LINE('',#49642,#9195);
#7351=LINE('',#49644,#9196);
#7352=LINE('',#49650,#9197);
#7353=LINE('',#49659,#9198);
#7354=LINE('',#49660,#9199);
#7355=LINE('',#49663,#9200);
#7356=LINE('',#49665,#9201);
#7357=LINE('',#49671,#9202);
#7358=LINE('',#49680,#9203);
#7359=LINE('',#49681,#9204);
#7360=LINE('',#49684,#9205);
#7361=LINE('',#49686,#9206);
#7362=LINE('',#49692,#9207);
#7363=LINE('',#49701,#9208);
#7364=LINE('',#49702,#9209);
#7365=LINE('',#49705,#9210);
#7366=LINE('',#49707,#9211);
#7367=LINE('',#49713,#9212);
#7368=LINE('',#49722,#9213);
#7369=LINE('',#49723,#9214);
#7370=LINE('',#49726,#9215);
#7371=LINE('',#49728,#9216);
#7372=LINE('',#49734,#9217);
#7373=LINE('',#49743,#9218);
#7374=LINE('',#49744,#9219);
#7375=LINE('',#49747,#9220);
#7376=LINE('',#49749,#9221);
#7377=LINE('',#49755,#9222);
#7378=LINE('',#49764,#9223);
#7379=LINE('',#49765,#9224);
#7380=LINE('',#49768,#9225);
#7381=LINE('',#49770,#9226);
#7382=LINE('',#49776,#9227);
#7383=LINE('',#49785,#9228);
#7384=LINE('',#49786,#9229);
#7385=LINE('',#49789,#9230);
#7386=LINE('',#49791,#9231);
#7387=LINE('',#49797,#9232);
#7388=LINE('',#49806,#9233);
#7389=LINE('',#49807,#9234);
#7390=LINE('',#49810,#9235);
#7391=LINE('',#49812,#9236);
#7392=LINE('',#49818,#9237);
#7393=LINE('',#49827,#9238);
#7394=LINE('',#49828,#9239);
#7395=LINE('',#49831,#9240);
#7396=LINE('',#49833,#9241);
#7397=LINE('',#49839,#9242);
#7398=LINE('',#49848,#9243);
#7399=LINE('',#49849,#9244);
#7400=LINE('',#49852,#9245);
#7401=LINE('',#49854,#9246);
#7402=LINE('',#49860,#9247);
#7403=LINE('',#49869,#9248);
#7404=LINE('',#49870,#9249);
#7405=LINE('',#49873,#9250);
#7406=LINE('',#49875,#9251);
#7407=LINE('',#49881,#9252);
#7408=LINE('',#49890,#9253);
#7409=LINE('',#49891,#9254);
#7410=LINE('',#49894,#9255);
#7411=LINE('',#49896,#9256);
#7412=LINE('',#49902,#9257);
#7413=LINE('',#49911,#9258);
#7414=LINE('',#49912,#9259);
#7415=LINE('',#49915,#9260);
#7416=LINE('',#49917,#9261);
#7417=LINE('',#49923,#9262);
#7418=LINE('',#49932,#9263);
#7419=LINE('',#49933,#9264);
#7420=LINE('',#49936,#9265);
#7421=LINE('',#49938,#9266);
#7422=LINE('',#49944,#9267);
#7423=LINE('',#49953,#9268);
#7424=LINE('',#49954,#9269);
#7425=LINE('',#49957,#9270);
#7426=LINE('',#49959,#9271);
#7427=LINE('',#49965,#9272);
#7428=LINE('',#49988,#9273);
#7429=LINE('',#50010,#9274);
#7430=LINE('',#50014,#9275);
#7431=LINE('',#50018,#9276);
#7432=LINE('',#50020,#9277);
#7433=LINE('',#50028,#9278);
#7434=LINE('',#50033,#9279);
#7435=LINE('',#50037,#9280);
#7436=LINE('',#50042,#9281);
#7437=LINE('',#50044,#9282);
#7438=LINE('',#50046,#9283);
#7439=LINE('',#50047,#9284);
#7440=LINE('',#50050,#9285);
#7441=LINE('',#50052,#9286);
#7442=LINE('',#50053,#9287);
#7443=LINE('',#50056,#9288);
#7444=LINE('',#50058,#9289);
#7445=LINE('',#50059,#9290);
#7446=LINE('',#50062,#9291);
#7447=LINE('',#50064,#9292);
#7448=LINE('',#50065,#9293);
#7449=LINE('',#50068,#9294);
#7450=LINE('',#50070,#9295);
#7451=LINE('',#50071,#9296);
#7452=LINE('',#50073,#9297);
#7453=LINE('',#50074,#9298);
#7454=LINE('',#50080,#9299);
#7455=LINE('',#50086,#9300);
#7456=LINE('',#50093,#9301);
#7457=LINE('',#50120,#9302);
#7458=LINE('',#50146,#9303);
#7459=LINE('',#50194,#9304);
#7460=LINE('',#50242,#9305);
#7461=LINE('',#50290,#9306);
#7462=LINE('',#50344,#9307);
#7463=LINE('',#50392,#9308);
#7464=LINE('',#50440,#9309);
#7465=LINE('',#50494,#9310);
#7466=LINE('',#50542,#9311);
#7467=LINE('',#50590,#9312);
#7468=LINE('',#50638,#9313);
#7469=LINE('',#50692,#9314);
#7470=LINE('',#50740,#9315);
#7471=LINE('',#50788,#9316);
#7472=LINE('',#50842,#9317);
#7473=LINE('',#50890,#9318);
#7474=LINE('',#50938,#9319);
#7475=LINE('',#50986,#9320);
#7476=LINE('',#51005,#9321);
#7477=LINE('',#51030,#9322);
#7478=LINE('',#51054,#9323);
#7479=LINE('',#51078,#9324);
#7480=LINE('',#51103,#9325);
#7481=LINE('',#51128,#9326);
#7482=LINE('',#51152,#9327);
#7483=LINE('',#51177,#9328);
#7484=LINE('',#51202,#9329);
#7485=LINE('',#51226,#9330);
#7486=LINE('',#51250,#9331);
#7487=LINE('',#51275,#9332);
#7488=LINE('',#51300,#9333);
#7489=LINE('',#51324,#9334);
#7490=LINE('',#51349,#9335);
#7491=LINE('',#51374,#9336);
#7492=LINE('',#51398,#9337);
#7493=LINE('',#51422,#9338);
#7494=LINE('',#52729,#9339);
#7495=LINE('',#52730,#9340);
#7496=LINE('',#52733,#9341);
#7497=LINE('',#52735,#9342);
#7498=LINE('',#52741,#9343);
#7499=LINE('',#52750,#9344);
#7500=LINE('',#52751,#9345);
#7501=LINE('',#52754,#9346);
#7502=LINE('',#52756,#9347);
#7503=LINE('',#52762,#9348);
#7504=LINE('',#52771,#9349);
#7505=LINE('',#52772,#9350);
#7506=LINE('',#52775,#9351);
#7507=LINE('',#52777,#9352);
#7508=LINE('',#52783,#9353);
#7509=LINE('',#52792,#9354);
#7510=LINE('',#52793,#9355);
#7511=LINE('',#52796,#9356);
#7512=LINE('',#52798,#9357);
#7513=LINE('',#52804,#9358);
#7514=LINE('',#52813,#9359);
#7515=LINE('',#52814,#9360);
#7516=LINE('',#52817,#9361);
#7517=LINE('',#52819,#9362);
#7518=LINE('',#52825,#9363);
#7519=LINE('',#52834,#9364);
#7520=LINE('',#52835,#9365);
#7521=LINE('',#52838,#9366);
#7522=LINE('',#52840,#9367);
#7523=LINE('',#52846,#9368);
#7524=LINE('',#52855,#9369);
#7525=LINE('',#52856,#9370);
#7526=LINE('',#52859,#9371);
#7527=LINE('',#52861,#9372);
#7528=LINE('',#52867,#9373);
#7529=LINE('',#52876,#9374);
#7530=LINE('',#52877,#9375);
#7531=LINE('',#52880,#9376);
#7532=LINE('',#52882,#9377);
#7533=LINE('',#52888,#9378);
#7534=LINE('',#52897,#9379);
#7535=LINE('',#52898,#9380);
#7536=LINE('',#52901,#9381);
#7537=LINE('',#52903,#9382);
#7538=LINE('',#52909,#9383);
#7539=LINE('',#52918,#9384);
#7540=LINE('',#52919,#9385);
#7541=LINE('',#52922,#9386);
#7542=LINE('',#52924,#9387);
#7543=LINE('',#52930,#9388);
#7544=LINE('',#52939,#9389);
#7545=LINE('',#52940,#9390);
#7546=LINE('',#52943,#9391);
#7547=LINE('',#52945,#9392);
#7548=LINE('',#52951,#9393);
#7549=LINE('',#52960,#9394);
#7550=LINE('',#52961,#9395);
#7551=LINE('',#52964,#9396);
#7552=LINE('',#52966,#9397);
#7553=LINE('',#52972,#9398);
#7554=LINE('',#52981,#9399);
#7555=LINE('',#52982,#9400);
#7556=LINE('',#52985,#9401);
#7557=LINE('',#52987,#9402);
#7558=LINE('',#52993,#9403);
#7559=LINE('',#53002,#9404);
#7560=LINE('',#53003,#9405);
#7561=LINE('',#53006,#9406);
#7562=LINE('',#53008,#9407);
#7563=LINE('',#53014,#9408);
#7564=LINE('',#53023,#9409);
#7565=LINE('',#53024,#9410);
#7566=LINE('',#53027,#9411);
#7567=LINE('',#53029,#9412);
#7568=LINE('',#53035,#9413);
#7569=LINE('',#53044,#9414);
#7570=LINE('',#53045,#9415);
#7571=LINE('',#53048,#9416);
#7572=LINE('',#53050,#9417);
#7573=LINE('',#53056,#9418);
#7574=LINE('',#53065,#9419);
#7575=LINE('',#53066,#9420);
#7576=LINE('',#53069,#9421);
#7577=LINE('',#53071,#9422);
#7578=LINE('',#53077,#9423);
#7579=LINE('',#53086,#9424);
#7580=LINE('',#53088,#9425);
#7581=LINE('',#53092,#9426);
#7582=LINE('',#53094,#9427);
#7583=LINE('',#53100,#9428);
#7584=LINE('',#53109,#9429);
#7585=LINE('',#53110,#9430);
#7586=LINE('',#53113,#9431);
#7587=LINE('',#53115,#9432);
#7588=LINE('',#53121,#9433);
#7589=LINE('',#53130,#9434);
#7590=LINE('',#53131,#9435);
#7591=LINE('',#53134,#9436);
#7592=LINE('',#53136,#9437);
#7593=LINE('',#53142,#9438);
#7594=LINE('',#53151,#9439);
#7595=LINE('',#53152,#9440);
#7596=LINE('',#53155,#9441);
#7597=LINE('',#53157,#9442);
#7598=LINE('',#53163,#9443);
#7599=LINE('',#53172,#9444);
#7600=LINE('',#53173,#9445);
#7601=LINE('',#53176,#9446);
#7602=LINE('',#53178,#9447);
#7603=LINE('',#53184,#9448);
#7604=LINE('',#53193,#9449);
#7605=LINE('',#53194,#9450);
#7606=LINE('',#53197,#9451);
#7607=LINE('',#53199,#9452);
#7608=LINE('',#53205,#9453);
#7609=LINE('',#53214,#9454);
#7610=LINE('',#53215,#9455);
#7611=LINE('',#53218,#9456);
#7612=LINE('',#53220,#9457);
#7613=LINE('',#53226,#9458);
#7614=LINE('',#53235,#9459);
#7615=LINE('',#53236,#9460);
#7616=LINE('',#53239,#9461);
#7617=LINE('',#53241,#9462);
#7618=LINE('',#53247,#9463);
#7619=LINE('',#53256,#9464);
#7620=LINE('',#53257,#9465);
#7621=LINE('',#53260,#9466);
#7622=LINE('',#53262,#9467);
#7623=LINE('',#53268,#9468);
#7624=LINE('',#53277,#9469);
#7625=LINE('',#53278,#9470);
#7626=LINE('',#53281,#9471);
#7627=LINE('',#53283,#9472);
#7628=LINE('',#53289,#9473);
#7629=LINE('',#53298,#9474);
#7630=LINE('',#53299,#9475);
#7631=LINE('',#53302,#9476);
#7632=LINE('',#53304,#9477);
#7633=LINE('',#53310,#9478);
#7634=LINE('',#53319,#9479);
#7635=LINE('',#53320,#9480);
#7636=LINE('',#53323,#9481);
#7637=LINE('',#53325,#9482);
#7638=LINE('',#53331,#9483);
#7639=LINE('',#53340,#9484);
#7640=LINE('',#53341,#9485);
#7641=LINE('',#53344,#9486);
#7642=LINE('',#53346,#9487);
#7643=LINE('',#53352,#9488);
#7644=LINE('',#53361,#9489);
#7645=LINE('',#53362,#9490);
#7646=LINE('',#53365,#9491);
#7647=LINE('',#53367,#9492);
#7648=LINE('',#53373,#9493);
#7649=LINE('',#53382,#9494);
#7650=LINE('',#53383,#9495);
#7651=LINE('',#53386,#9496);
#7652=LINE('',#53388,#9497);
#7653=LINE('',#53394,#9498);
#7654=LINE('',#53403,#9499);
#7655=LINE('',#53404,#9500);
#7656=LINE('',#53407,#9501);
#7657=LINE('',#53409,#9502);
#7658=LINE('',#53415,#9503);
#7659=LINE('',#53424,#9504);
#7660=LINE('',#53425,#9505);
#7661=LINE('',#53428,#9506);
#7662=LINE('',#53430,#9507);
#7663=LINE('',#53436,#9508);
#7664=LINE('',#53445,#9509);
#7665=LINE('',#53446,#9510);
#7666=LINE('',#53449,#9511);
#7667=LINE('',#53451,#9512);
#7668=LINE('',#53457,#9513);
#7669=LINE('',#53480,#9514);
#7670=LINE('',#53502,#9515);
#7671=LINE('',#53506,#9516);
#7672=LINE('',#53510,#9517);
#7673=LINE('',#53512,#9518);
#7674=LINE('',#53520,#9519);
#7675=LINE('',#53525,#9520);
#7676=LINE('',#53529,#9521);
#7677=LINE('',#53534,#9522);
#7678=LINE('',#53536,#9523);
#7679=LINE('',#53538,#9524);
#7680=LINE('',#53539,#9525);
#7681=LINE('',#53542,#9526);
#7682=LINE('',#53544,#9527);
#7683=LINE('',#53545,#9528);
#7684=LINE('',#53548,#9529);
#7685=LINE('',#53550,#9530);
#7686=LINE('',#53551,#9531);
#7687=LINE('',#53554,#9532);
#7688=LINE('',#53556,#9533);
#7689=LINE('',#53557,#9534);
#7690=LINE('',#53560,#9535);
#7691=LINE('',#53562,#9536);
#7692=LINE('',#53563,#9537);
#7693=LINE('',#53565,#9538);
#7694=LINE('',#53566,#9539);
#7695=LINE('',#53572,#9540);
#7696=LINE('',#53578,#9541);
#7697=VECTOR('',#25660,1.);
#7698=VECTOR('',#25663,1.);
#7699=VECTOR('',#25668,1.);
#7700=VECTOR('',#25669,1.);
#7701=VECTOR('',#25670,1.);
#7702=VECTOR('',#25673,1.);
#7703=VECTOR('',#25680,1.);
#7704=VECTOR('',#25681,1.);
#7705=VECTOR('',#25682,1.);
#7706=VECTOR('',#25685,1.);
#7707=VECTOR('',#25692,1.);
#7708=VECTOR('',#25693,1.);
#7709=VECTOR('',#25694,1.);
#7710=VECTOR('',#25697,1.);
#7711=VECTOR('',#25704,1.);
#7712=VECTOR('',#25705,1.);
#7713=VECTOR('',#25708,1.);
#7714=VECTOR('',#25709,1.);
#7715=VECTOR('',#25710,1.);
#7716=VECTOR('',#25713,1.);
#7717=VECTOR('',#25718,1.);
#7718=VECTOR('',#25719,1.);
#7719=VECTOR('',#25722,1.);
#7720=VECTOR('',#25743,1.);
#7721=VECTOR('',#25744,1.);
#7722=VECTOR('',#25749,1.);
#7723=VECTOR('',#25750,1.);
#7724=VECTOR('',#25753,1.);
#7725=VECTOR('',#25758,1.);
#7726=VECTOR('',#25759,1.);
#7727=VECTOR('',#25762,1.);
#7728=VECTOR('',#25769,1.);
#7729=VECTOR('',#25770,1.);
#7730=VECTOR('',#25771,1.);
#7731=VECTOR('',#25774,1.);
#7732=VECTOR('',#25781,1.);
#7733=VECTOR('',#25782,1.);
#7734=VECTOR('',#25785,1.);
#7735=VECTOR('',#25786,1.);
#7736=VECTOR('',#25787,1.);
#7737=VECTOR('',#25790,1.);
#7738=VECTOR('',#25795,1.);
#7739=VECTOR('',#25796,1.);
#7740=VECTOR('',#25799,1.);
#7741=VECTOR('',#25804,1.);
#7742=VECTOR('',#25805,1.);
#7743=VECTOR('',#25808,1.);
#7744=VECTOR('',#25813,1.);
#7745=VECTOR('',#25814,1.);
#7746=VECTOR('',#25815,1.);
#7747=VECTOR('',#25816,1.);
#7748=VECTOR('',#25819,1.);
#7749=VECTOR('',#25826,1.);
#7750=VECTOR('',#25827,1.);
#7751=VECTOR('',#25828,1.);
#7752=VECTOR('',#25831,1.);
#7753=VECTOR('',#25838,1.);
#7754=VECTOR('',#25839,1.);
#7755=VECTOR('',#25840,1.);
#7756=VECTOR('',#25843,1.);
#7757=VECTOR('',#25850,1.);
#7758=VECTOR('',#25851,1.);
#7759=VECTOR('',#25852,1.);
#7760=VECTOR('',#25861,1.);
#7761=VECTOR('',#25864,1.);
#7762=VECTOR('',#25867,1.);
#7763=VECTOR('',#25868,1.);
#7764=VECTOR('',#25871,1.);
#7765=VECTOR('',#25876,1.);
#7766=VECTOR('',#25877,1.);
#7767=VECTOR('',#25896,1.);
#7768=VECTOR('',#25897,1.);
#7769=VECTOR('',#25900,1.);
#7770=VECTOR('',#25903,1.);
#7771=VECTOR('',#25906,1.);
#7772=VECTOR('',#25909,1.);
#7773=VECTOR('',#25910,1.);
#7774=VECTOR('',#25911,1.);
#7775=VECTOR('',#25914,1.);
#7776=VECTOR('',#25921,1.);
#7777=VECTOR('',#25922,1.);
#7778=VECTOR('',#25923,1.);
#7779=VECTOR('',#25932,1.);
#7780=VECTOR('',#25933,1.);
#7781=VECTOR('',#25936,1.);
#7782=VECTOR('',#25941,0.565);
#7783=VECTOR('',#25950,0.55);
#7784=VECTOR('',#25953,0.565);
#7785=VECTOR('',#25962,0.55);
#7786=VECTOR('',#25965,0.565);
#7787=VECTOR('',#25974,0.55);
#7788=VECTOR('',#25977,0.565);
#7789=VECTOR('',#25986,0.55);
#7790=VECTOR('',#25989,0.515);
#7791=VECTOR('',#25998,0.5);
#7792=VECTOR('',#26001,0.515);
#7793=VECTOR('',#26010,0.5);
#7794=VECTOR('',#26013,0.515);
#7795=VECTOR('',#26022,0.5);
#7796=VECTOR('',#26025,0.2875);
#7797=VECTOR('',#26030,0.275);
#7798=VECTOR('',#26035,0.2875);
#7799=VECTOR('',#26042,0.2875);
#7800=VECTOR('',#26047,0.275);
#7801=VECTOR('',#26052,0.2875);
#7802=VECTOR('',#26059,0.2875);
#7803=VECTOR('',#26064,0.275);
#7804=VECTOR('',#26069,0.2875);
#7805=VECTOR('',#26076,0.342499999999999);
#7806=VECTOR('',#26081,0.33);
#7807=VECTOR('',#26086,0.342499999999999);
#7808=VECTOR('',#26093,0.342499999999999);
#7809=VECTOR('',#26098,0.33);
#7810=VECTOR('',#26103,0.342499999999999);
#7811=VECTOR('',#26110,0.342499999999999);
#7812=VECTOR('',#26115,0.33);
#7813=VECTOR('',#26120,0.342499999999999);
#7814=VECTOR('',#26127,0.342499999999999);
#7815=VECTOR('',#26132,0.33);
#7816=VECTOR('',#26137,0.342499999999999);
#7817=VECTOR('',#26148,1.);
#7818=VECTOR('',#26151,1.);
#7819=VECTOR('',#26154,1.);
#7820=VECTOR('',#26161,1.);
#7821=VECTOR('',#26162,1.);
#7822=VECTOR('',#26163,1.);
#7823=VECTOR('',#26164,1.);
#7824=VECTOR('',#26167,1.);
#7825=VECTOR('',#26168,1.);
#7826=VECTOR('',#26169,1.);
#7827=VECTOR('',#26172,1.);
#7828=VECTOR('',#26179,1.);
#7829=VECTOR('',#26180,1.);
#7830=VECTOR('',#26181,1.);
#7831=VECTOR('',#26184,1.);
#7832=VECTOR('',#26191,1.);
#7833=VECTOR('',#26192,1.);
#7834=VECTOR('',#26195,1.);
#7835=VECTOR('',#26198,1.);
#7836=VECTOR('',#26201,1.);
#7837=VECTOR('',#26202,1.);
#7838=VECTOR('',#26205,1.);
#7839=VECTOR('',#26206,1.);
#7840=VECTOR('',#26225,1.);
#7841=VECTOR('',#26226,1.);
#7842=VECTOR('',#26227,1.);
#7843=VECTOR('',#26228,1.);
#7844=VECTOR('',#26229,1.);
#7845=VECTOR('',#26232,1.);
#7846=VECTOR('',#26233,1.);
#7847=VECTOR('',#26234,1.);
#7848=VECTOR('',#26243,1.);
#7849=VECTOR('',#26244,1.);
#7850=VECTOR('',#26245,1.);
#7851=VECTOR('',#26246,1.);
#7852=VECTOR('',#26249,1.);
#7853=VECTOR('',#26250,1.);
#7854=VECTOR('',#26251,1.);
#7855=VECTOR('',#26254,1.);
#7856=VECTOR('',#26255,1.);
#7857=VECTOR('',#26256,1.);
#7858=VECTOR('',#26259,1.);
#7859=VECTOR('',#26264,1.);
#7860=VECTOR('',#26265,1.);
#7861=VECTOR('',#26266,1.);
#7862=VECTOR('',#26275,1.);
#7863=VECTOR('',#26278,1.);
#7864=VECTOR('',#26283,1.);
#7865=VECTOR('',#26284,1.);
#7866=VECTOR('',#26285,1.);
#7867=VECTOR('',#26286,1.);
#7868=VECTOR('',#26289,1.);
#7869=VECTOR('',#26290,1.);
#7870=VECTOR('',#26293,1.);
#7871=VECTOR('',#26294,1.);
#7872=VECTOR('',#26297,1.);
#7873=VECTOR('',#26298,1.);
#7874=VECTOR('',#26301,1.);
#7875=VECTOR('',#26302,1.);
#7876=VECTOR('',#26303,1.);
#7877=VECTOR('',#26306,1.);
#7878=VECTOR('',#26313,1.);
#7879=VECTOR('',#26314,1.);
#7880=VECTOR('',#26315,1.);
#7881=VECTOR('',#26324,1.);
#7882=VECTOR('',#26327,1.);
#7883=VECTOR('',#26330,1.);
#7884=VECTOR('',#26331,1.);
#7885=VECTOR('',#26334,1.);
#7886=VECTOR('',#26335,1.);
#7887=VECTOR('',#26338,1.);
#7888=VECTOR('',#26339,1.);
#7889=VECTOR('',#26344,1.);
#7890=VECTOR('',#26345,1.);
#7891=VECTOR('',#26346,1.);
#7892=VECTOR('',#26349,1.);
#7893=VECTOR('',#26350,1.);
#7894=VECTOR('',#26353,1.);
#7895=VECTOR('',#26358,1.);
#7896=VECTOR('',#26359,1.);
#7897=VECTOR('',#26360,1.);
#7898=VECTOR('',#26363,1.);
#7899=VECTOR('',#26370,1.);
#7900=VECTOR('',#26371,1.);
#7901=VECTOR('',#26374,1.);
#7902=VECTOR('',#26375,1.);
#7903=VECTOR('',#26402,3.315);
#7904=VECTOR('',#26407,3.3);
#7905=VECTOR('',#26412,3.79);
#7906=VECTOR('',#26421,3.775);
#7907=VECTOR('',#26424,3.315);
#7908=VECTOR('',#26431,0.185);
#7909=VECTOR('',#26440,0.17);
#7910=VECTOR('',#26443,0.185);
#7911=VECTOR('',#26446,0.185);
#7912=VECTOR('',#26455,0.17);
#7913=VECTOR('',#26458,0.185);
#7914=VECTOR('',#26461,0.185);
#7915=VECTOR('',#26470,0.17);
#7916=VECTOR('',#26473,0.185);
#7917=VECTOR('',#26476,0.42);
#7918=VECTOR('',#26481,0.405);
#7919=VECTOR('',#26486,0.42);
#7920=VECTOR('',#26491,0.404999999999999);
#7921=VECTOR('',#26496,0.42);
#7922=VECTOR('',#26501,0.405);
#7923=VECTOR('',#26508,0.459393398282203);
#7924=VECTOR('',#26517,0.455);
#7925=VECTOR('',#26520,1.);
#7926=VECTOR('',#26527,0.415606601717798);
#7927=VECTOR('',#26532,0.405);
#7928=VECTOR('',#26535,0.2025);
#7929=VECTOR('',#26538,0.1275);
#7930=VECTOR('',#26543,0.255);
#7931=VECTOR('',#26548,0.305);
#7932=VECTOR('',#26551,0.1275);
#7933=VECTOR('',#26556,0.255);
#7934=VECTOR('',#26561,0.305);
#7935=VECTOR('',#26564,0.1275);
#7936=VECTOR('',#26569,0.255);
#7937=VECTOR('',#26574,0.305);
#7938=VECTOR('',#26577,0.43);
#7939=VECTOR('',#26580,0.429999999999999);
#7940=VECTOR('',#26583,0.430000000000001);
#7941=VECTOR('',#26586,0.0775000000000001);
#7942=VECTOR('',#26591,0.155);
#7943=VECTOR('',#26596,0.205);
#7944=VECTOR('',#26599,0.0775000000000001);
#7945=VECTOR('',#26604,0.155);
#7946=VECTOR('',#26609,0.205000000000001);
#7947=VECTOR('',#26612,0.0775000000000006);
#7948=VECTOR('',#26617,0.155);
#7949=VECTOR('',#26622,0.205);
#7950=VECTOR('',#26631,1.);
#7951=VECTOR('',#26634,1.);
#7952=VECTOR('',#26639,1.);
#7953=VECTOR('',#26640,1.);
#7954=VECTOR('',#26641,1.);
#7955=VECTOR('',#26644,1.);
#7956=VECTOR('',#26651,1.);
#7957=VECTOR('',#26652,1.);
#7958=VECTOR('',#26653,1.);
#7959=VECTOR('',#26656,1.);
#7960=VECTOR('',#26663,1.);
#7961=VECTOR('',#26664,1.);
#7962=VECTOR('',#26665,1.);
#7963=VECTOR('',#26668,1.);
#7964=VECTOR('',#26675,1.);
#7965=VECTOR('',#26676,1.);
#7966=VECTOR('',#26679,1.);
#7967=VECTOR('',#26680,1.);
#7968=VECTOR('',#26681,1.);
#7969=VECTOR('',#26684,1.);
#7970=VECTOR('',#26689,1.);
#7971=VECTOR('',#26690,1.);
#7972=VECTOR('',#26693,1.);
#7973=VECTOR('',#26708,1.);
#7974=VECTOR('',#26709,1.);
#7975=VECTOR('',#26710,1.);
#7976=VECTOR('',#26711,1.);
#7977=VECTOR('',#26714,1.);
#7978=VECTOR('',#26721,1.);
#7979=VECTOR('',#26722,1.);
#7980=VECTOR('',#26723,1.);
#7981=VECTOR('',#26726,1.);
#7982=VECTOR('',#26731,1.);
#7983=VECTOR('',#26732,1.);
#7984=VECTOR('',#26735,1.);
#7985=VECTOR('',#26740,1.);
#7986=VECTOR('',#26741,1.);
#7987=VECTOR('',#26750,1.);
#7988=VECTOR('',#26753,1.);
#7989=VECTOR('',#26756,1.);
#7990=VECTOR('',#26757,1.);
#7991=VECTOR('',#26760,1.);
#7992=VECTOR('',#26765,1.);
#7993=VECTOR('',#26766,1.);
#7994=VECTOR('',#26769,1.);
#7995=VECTOR('',#26772,1.);
#7996=VECTOR('',#26775,1.);
#7997=VECTOR('',#26778,1.);
#7998=VECTOR('',#26781,1.);
#7999=VECTOR('',#26782,1.);
#8000=VECTOR('',#26785,1.);
#8001=VECTOR('',#26790,1.);
#8002=VECTOR('',#26791,1.);
#8003=VECTOR('',#26794,1.);
#8004=VECTOR('',#26801,1.);
#8005=VECTOR('',#26802,1.);
#8006=VECTOR('',#26803,1.);
#8007=VECTOR('',#26806,1.);
#8008=VECTOR('',#26813,1.);
#8009=VECTOR('',#26814,1.);
#8010=VECTOR('',#26817,1.);
#8011=VECTOR('',#26818,1.);
#8012=VECTOR('',#26819,1.);
#8013=VECTOR('',#26822,1.);
#8014=VECTOR('',#26827,1.);
#8015=VECTOR('',#26828,1.);
#8016=VECTOR('',#26831,1.);
#8017=VECTOR('',#26836,3.79);
#8018=VECTOR('',#26845,3.775);
#8019=VECTOR('',#26848,1.);
#8020=VECTOR('',#26849,1.);
#8021=VECTOR('',#26854,1.);
#8022=VECTOR('',#26855,1.);
#8023=VECTOR('',#26858,1.);
#8024=VECTOR('',#26863,1.);
#8025=VECTOR('',#26864,1.);
#8026=VECTOR('',#26867,1.);
#8027=VECTOR('',#26874,1.);
#8028=VECTOR('',#26875,1.);
#8029=VECTOR('',#26876,1.);
#8030=VECTOR('',#26879,1.);
#8031=VECTOR('',#26886,1.);
#8032=VECTOR('',#26887,1.);
#8033=VECTOR('',#26890,1.);
#8034=VECTOR('',#26891,1.);
#8035=VECTOR('',#26894,1.);
#8036=VECTOR('',#26905,3.315);
#8037=VECTOR('',#26912,3.3);
#8038=VECTOR('',#26919,3.3543933982822);
#8039=VECTOR('',#26922,3.325);
#8040=VECTOR('',#26927,3.3106066017178);
#8041=VECTOR('',#26930,0.1025);
#8042=VECTOR('',#26935,0.205);
#8043=VECTOR('',#26940,0.255);
#8044=VECTOR('',#26943,0.1025);
#8045=VECTOR('',#26948,0.205);
#8046=VECTOR('',#26953,0.255);
#8047=VECTOR('',#26956,0.1025);
#8048=VECTOR('',#26961,0.205);
#8049=VECTOR('',#26966,0.255);
#8050=VECTOR('',#26971,1.);
#8051=VECTOR('',#26976,1.);
#8052=VECTOR('',#26977,1.);
#8053=VECTOR('',#26980,1.);
#8054=VECTOR('',#26991,4.0106066017178);
#8055=VECTOR('',#26998,4.);
#8056=VECTOR('',#27005,4.025);
#8057=VECTOR('',#27012,4.0106066017178);
#8058=VECTOR('',#27017,4.025);
#8059=VECTOR('',#27020,4.0543933982822);
#8060=VECTOR('',#27037,4.7456066017178);
#8061=VECTOR('',#27042,4.775);
#8062=VECTOR('',#27045,4.0543933982822);
#8063=VECTOR('',#27054,4.7893933982822);
#8064=VECTOR('',#27065,4.8);
#8065=VECTOR('',#27070,4.7456066017178);
#8066=VECTOR('',#27073,4.775);
#8067=VECTOR('',#27078,4.7893933982822);
#8068=VECTOR('',#27081,0.0774999999999997);
#8069=VECTOR('',#27086,0.155);
#8070=VECTOR('',#27091,0.205);
#8071=VECTOR('',#27094,0.0774999999999997);
#8072=VECTOR('',#27099,0.154999999999999);
#8073=VECTOR('',#27104,0.204999999999999);
#8074=VECTOR('',#27107,0.0774999999999997);
#8075=VECTOR('',#27112,0.155);
#8076=VECTOR('',#27117,0.205);
#8077=VECTOR('',#27124,0.185);
#8078=VECTOR('',#27133,0.17);
#8079=VECTOR('',#27154,0.185);
#8080=VECTOR('',#27173,0.185);
#8081=VECTOR('',#27182,0.17);
#8082=VECTOR('',#27185,0.185);
#8083=VECTOR('',#27188,0.185);
#8084=VECTOR('',#27197,0.17);
#8085=VECTOR('',#27200,0.185);
#8086=VECTOR('',#27203,0.185000000000001);
#8087=VECTOR('',#27212,0.170000000000001);
#8088=VECTOR('',#27215,0.185000000000001);
#8089=VECTOR('',#27218,0.185);
#8090=VECTOR('',#27227,0.17);
#8091=VECTOR('',#27230,0.185);
#8092=VECTOR('',#27233,0.185);
#8093=VECTOR('',#27242,0.17);
#8094=VECTOR('',#27245,0.185);
#8095=VECTOR('',#27248,4.68);
#8096=VECTOR('',#27255,4.7);
#8097=VECTOR('',#27262,4.68);
#8098=VECTOR('',#27265,3.32);
#8099=VECTOR('',#27276,3.3);
#8100=VECTOR('',#27279,3.32);
#8101=VECTOR('',#27284,0.4);
#8102=VECTOR('',#27285,0.4);
#8103=VECTOR('',#27292,0.4);
#8104=VECTOR('',#27295,0.4);
#8105=VECTOR('',#27298,0.4);
#8106=VECTOR('',#27301,0.4);
#8107=VECTOR('',#27304,0.4);
#8108=VECTOR('',#27307,0.4);
#8109=VECTOR('',#27310,0.4);
#8110=VECTOR('',#27313,0.4);
#8111=VECTOR('',#27316,0.4);
#8112=VECTOR('',#27319,0.352375);
#8113=VECTOR('',#27324,0.352375);
#8114=VECTOR('',#27327,0.352375);
#8115=VECTOR('',#27330,0.352375);
#8116=VECTOR('',#27333,0.352375);
#8117=VECTOR('',#27336,0.352375);
#8118=VECTOR('',#27339,0.352375);
#8119=VECTOR('',#27342,0.352375);
#8120=VECTOR('',#27345,0.352375);
#8121=VECTOR('',#27348,0.352375);
#8122=VECTOR('',#27351,0.352375);
#8123=VECTOR('',#27362,0.08);
#8124=VECTOR('',#27369,0.08);
#8125=VECTOR('',#27376,0.08);
#8126=VECTOR('',#27383,0.08);
#8127=VECTOR('',#27388,1.);
#8128=VECTOR('',#27389,1.);
#8129=VECTOR('',#27390,1.);
#8130=VECTOR('',#27391,1.);
#8131=VECTOR('',#27396,1.);
#8132=VECTOR('',#27399,1.);
#8133=VECTOR('',#27400,1.);
#8134=VECTOR('',#27407,1.);
#8135=VECTOR('',#27408,1.);
#8136=VECTOR('',#27409,1.);
#8137=VECTOR('',#27410,1.);
#8138=VECTOR('',#27415,1.);
#8139=VECTOR('',#27418,1.);
#8140=VECTOR('',#27419,1.);
#8141=VECTOR('',#27426,1.);
#8142=VECTOR('',#27427,1.);
#8143=VECTOR('',#27428,1.);
#8144=VECTOR('',#27429,1.);
#8145=VECTOR('',#27434,1.);
#8146=VECTOR('',#27437,1.);
#8147=VECTOR('',#27438,1.);
#8148=VECTOR('',#27445,1.);
#8149=VECTOR('',#27446,1.);
#8150=VECTOR('',#27447,1.);
#8151=VECTOR('',#27448,1.);
#8152=VECTOR('',#27453,1.);
#8153=VECTOR('',#27456,1.);
#8154=VECTOR('',#27457,1.);
#8155=VECTOR('',#27464,1.);
#8156=VECTOR('',#27465,1.);
#8157=VECTOR('',#27466,1.);
#8158=VECTOR('',#27467,1.);
#8159=VECTOR('',#27472,1.);
#8160=VECTOR('',#27475,1.);
#8161=VECTOR('',#27476,1.);
#8162=VECTOR('',#27483,1.);
#8163=VECTOR('',#27484,1.);
#8164=VECTOR('',#27485,1.);
#8165=VECTOR('',#27486,1.);
#8166=VECTOR('',#27491,1.);
#8167=VECTOR('',#27494,1.);
#8168=VECTOR('',#27495,1.);
#8169=VECTOR('',#27502,1.);
#8170=VECTOR('',#27503,1.);
#8171=VECTOR('',#27504,1.);
#8172=VECTOR('',#27505,1.);
#8173=VECTOR('',#27510,1.);
#8174=VECTOR('',#27513,1.);
#8175=VECTOR('',#27514,1.);
#8176=VECTOR('',#27521,1.);
#8177=VECTOR('',#27522,1.);
#8178=VECTOR('',#27523,1.);
#8179=VECTOR('',#27524,1.);
#8180=VECTOR('',#27529,1.);
#8181=VECTOR('',#27532,1.);
#8182=VECTOR('',#27533,1.);
#8183=VECTOR('',#27540,1.);
#8184=VECTOR('',#27541,1.);
#8185=VECTOR('',#27542,1.);
#8186=VECTOR('',#27543,1.);
#8187=VECTOR('',#27548,1.);
#8188=VECTOR('',#27551,1.);
#8189=VECTOR('',#27552,1.);
#8190=VECTOR('',#27559,1.);
#8191=VECTOR('',#27560,1.);
#8192=VECTOR('',#27561,1.);
#8193=VECTOR('',#27562,1.);
#8194=VECTOR('',#27567,1.);
#8195=VECTOR('',#27570,1.);
#8196=VECTOR('',#27571,1.);
#8197=VECTOR('',#27578,1.);
#8198=VECTOR('',#27579,1.);
#8199=VECTOR('',#27580,1.);
#8200=VECTOR('',#27581,1.);
#8201=VECTOR('',#27586,1.);
#8202=VECTOR('',#27589,1.);
#8203=VECTOR('',#27590,1.);
#8204=VECTOR('',#27597,1.);
#8205=VECTOR('',#27598,1.);
#8206=VECTOR('',#27599,1.);
#8207=VECTOR('',#27600,1.);
#8208=VECTOR('',#27605,1.);
#8209=VECTOR('',#27610,1.);
#8210=VECTOR('',#27611,1.);
#8211=VECTOR('',#27620,1.);
#8212=VECTOR('',#27621,1.);
#8213=VECTOR('',#27622,1.);
#8214=VECTOR('',#27623,1.);
#8215=VECTOR('',#27628,1.);
#8216=VECTOR('',#27631,1.);
#8217=VECTOR('',#27632,1.);
#8218=VECTOR('',#27639,1.);
#8219=VECTOR('',#27640,1.);
#8220=VECTOR('',#27641,1.);
#8221=VECTOR('',#27642,1.);
#8222=VECTOR('',#27647,1.);
#8223=VECTOR('',#27650,1.);
#8224=VECTOR('',#27651,1.);
#8225=VECTOR('',#27658,1.);
#8226=VECTOR('',#27659,1.);
#8227=VECTOR('',#27660,1.);
#8228=VECTOR('',#27661,1.);
#8229=VECTOR('',#27666,1.);
#8230=VECTOR('',#27669,1.);
#8231=VECTOR('',#27670,1.);
#8232=VECTOR('',#27677,1.);
#8233=VECTOR('',#27678,1.);
#8234=VECTOR('',#27679,1.);
#8235=VECTOR('',#27680,1.);
#8236=VECTOR('',#27685,1.);
#8237=VECTOR('',#27688,1.);
#8238=VECTOR('',#27689,1.);
#8239=VECTOR('',#27696,1.);
#8240=VECTOR('',#27697,1.);
#8241=VECTOR('',#27698,1.);
#8242=VECTOR('',#27699,1.);
#8243=VECTOR('',#27704,1.);
#8244=VECTOR('',#27707,1.);
#8245=VECTOR('',#27708,1.);
#8246=VECTOR('',#27715,1.);
#8247=VECTOR('',#27716,1.);
#8248=VECTOR('',#27717,1.);
#8249=VECTOR('',#27718,1.);
#8250=VECTOR('',#27723,1.);
#8251=VECTOR('',#27726,1.);
#8252=VECTOR('',#27727,1.);
#8253=VECTOR('',#27734,1.);
#8254=VECTOR('',#27735,1.);
#8255=VECTOR('',#27736,1.);
#8256=VECTOR('',#27737,1.);
#8257=VECTOR('',#27742,1.);
#8258=VECTOR('',#27745,1.);
#8259=VECTOR('',#27746,1.);
#8260=VECTOR('',#27753,1.);
#8261=VECTOR('',#27754,1.);
#8262=VECTOR('',#27755,1.);
#8263=VECTOR('',#27756,1.);
#8264=VECTOR('',#27761,1.);
#8265=VECTOR('',#27764,1.);
#8266=VECTOR('',#27765,1.);
#8267=VECTOR('',#27772,1.);
#8268=VECTOR('',#27773,1.);
#8269=VECTOR('',#27774,1.);
#8270=VECTOR('',#27775,1.);
#8271=VECTOR('',#27780,1.);
#8272=VECTOR('',#27783,1.);
#8273=VECTOR('',#27784,1.);
#8274=VECTOR('',#27791,1.);
#8275=VECTOR('',#27792,1.);
#8276=VECTOR('',#27793,1.);
#8277=VECTOR('',#27794,1.);
#8278=VECTOR('',#27799,1.);
#8279=VECTOR('',#27802,1.);
#8280=VECTOR('',#27803,1.);
#8281=VECTOR('',#27810,1.);
#8282=VECTOR('',#27811,1.);
#8283=VECTOR('',#27812,1.);
#8284=VECTOR('',#27813,1.);
#8285=VECTOR('',#27818,1.);
#8286=VECTOR('',#27821,1.);
#8287=VECTOR('',#27822,1.);
#8288=VECTOR('',#27829,1.);
#8289=VECTOR('',#27830,1.);
#8290=VECTOR('',#27831,1.);
#8291=VECTOR('',#27832,1.);
#8292=VECTOR('',#27837,1.);
#8293=VECTOR('',#27840,1.);
#8294=VECTOR('',#27841,1.);
#8295=VECTOR('',#27850,0.06);
#8296=VECTOR('',#27857,0.045);
#8297=VECTOR('',#27866,0.25);
#8298=VECTOR('',#27873,0.5);
#8299=VECTOR('',#27874,0.5);
#8300=VECTOR('',#27885,0.52);
#8301=VECTOR('',#27890,0.5);
#8302=VECTOR('',#27895,1.);
#8303=VECTOR('',#27896,1.);
#8304=VECTOR('',#27897,1.);
#8305=VECTOR('',#27898,1.);
#8306=VECTOR('',#27901,1.);
#8307=VECTOR('',#27902,1.);
#8308=VECTOR('',#27903,1.);
#8309=VECTOR('',#27906,1.);
#8310=VECTOR('',#27907,1.);
#8311=VECTOR('',#27908,1.);
#8312=VECTOR('',#27911,1.);
#8313=VECTOR('',#27912,1.);
#8314=VECTOR('',#27913,1.);
#8315=VECTOR('',#27916,1.);
#8316=VECTOR('',#27917,1.);
#8317=VECTOR('',#27918,1.);
#8318=VECTOR('',#27921,1.);
#8319=VECTOR('',#27922,1.);
#8320=VECTOR('',#27927,1.);
#8321=VECTOR('',#27928,1.);
#8322=VECTOR('',#27929,1.);
#8323=VECTOR('',#27930,1.);
#8324=VECTOR('',#27935,1.);
#8325=VECTOR('',#27936,1.);
#8326=VECTOR('',#27937,1.);
#8327=VECTOR('',#27940,1.);
#8328=VECTOR('',#27941,1.);
#8329=VECTOR('',#27944,1.);
#8330=VECTOR('',#27945,1.);
#8331=VECTOR('',#27948,1.);
#8332=VECTOR('',#27957,0.38);
#8333=VECTOR('',#27966,3.725);
#8334=VECTOR('',#27973,3.75);
#8335=VECTOR('',#27982,3.725);
#8336=VECTOR('',#27993,0.385);
#8337=VECTOR('',#28010,0.4);
#8338=VECTOR('',#28015,0.385);
#8339=VECTOR('',#28028,0.4);
#8340=VECTOR('',#28033,0.39);
#8341=VECTOR('',#28036,0.4);
#8342=VECTOR('',#28047,0.39);
#8343=VECTOR('',#28056,0.25);
#8344=VECTOR('',#28065,0.589393398282202);
#8345=VECTOR('',#28072,0.6);
#8346=VECTOR('',#28081,0.58);
#8347=VECTOR('',#28084,0.585);
#8348=VECTOR('',#28093,1.);
#8349=VECTOR('',#28094,1.);
#8350=VECTOR('',#28095,1.);
#8351=VECTOR('',#28096,1.);
#8352=VECTOR('',#28101,1.);
#8353=VECTOR('',#28104,1.);
#8354=VECTOR('',#28105,1.);
#8355=VECTOR('',#28112,1.);
#8356=VECTOR('',#28113,1.);
#8357=VECTOR('',#28114,1.);
#8358=VECTOR('',#28115,1.);
#8359=VECTOR('',#28120,1.);
#8360=VECTOR('',#28123,1.);
#8361=VECTOR('',#28124,1.);
#8362=VECTOR('',#28131,1.);
#8363=VECTOR('',#28132,1.);
#8364=VECTOR('',#28133,1.);
#8365=VECTOR('',#28134,1.);
#8366=VECTOR('',#28139,1.);
#8367=VECTOR('',#28142,1.);
#8368=VECTOR('',#28143,1.);
#8369=VECTOR('',#28150,1.);
#8370=VECTOR('',#28151,1.);
#8371=VECTOR('',#28152,1.);
#8372=VECTOR('',#28153,1.);
#8373=VECTOR('',#28158,1.);
#8374=VECTOR('',#28161,1.);
#8375=VECTOR('',#28162,1.);
#8376=VECTOR('',#28169,1.);
#8377=VECTOR('',#28170,1.);
#8378=VECTOR('',#28171,1.);
#8379=VECTOR('',#28172,1.);
#8380=VECTOR('',#28177,1.);
#8381=VECTOR('',#28180,1.);
#8382=VECTOR('',#28181,1.);
#8383=VECTOR('',#28188,1.);
#8384=VECTOR('',#28189,1.);
#8385=VECTOR('',#28190,1.);
#8386=VECTOR('',#28191,1.);
#8387=VECTOR('',#28196,1.);
#8388=VECTOR('',#28199,1.);
#8389=VECTOR('',#28200,1.);
#8390=VECTOR('',#28207,1.);
#8391=VECTOR('',#28208,1.);
#8392=VECTOR('',#28209,1.);
#8393=VECTOR('',#28210,1.);
#8394=VECTOR('',#28215,1.);
#8395=VECTOR('',#28218,1.);
#8396=VECTOR('',#28219,1.);
#8397=VECTOR('',#28226,1.);
#8398=VECTOR('',#28227,1.);
#8399=VECTOR('',#28228,1.);
#8400=VECTOR('',#28229,1.);
#8401=VECTOR('',#28234,1.);
#8402=VECTOR('',#28237,1.);
#8403=VECTOR('',#28238,1.);
#8404=VECTOR('',#28245,1.);
#8405=VECTOR('',#28246,1.);
#8406=VECTOR('',#28247,1.);
#8407=VECTOR('',#28248,1.);
#8408=VECTOR('',#28253,1.);
#8409=VECTOR('',#28258,1.);
#8410=VECTOR('',#28259,1.);
#8411=VECTOR('',#28268,1.);
#8412=VECTOR('',#28269,1.);
#8413=VECTOR('',#28270,1.);
#8414=VECTOR('',#28271,1.);
#8415=VECTOR('',#28276,1.);
#8416=VECTOR('',#28279,1.);
#8417=VECTOR('',#28280,1.);
#8418=VECTOR('',#28287,1.);
#8419=VECTOR('',#28288,1.);
#8420=VECTOR('',#28289,1.);
#8421=VECTOR('',#28290,1.);
#8422=VECTOR('',#28295,1.);
#8423=VECTOR('',#28298,1.);
#8424=VECTOR('',#28299,1.);
#8425=VECTOR('',#28306,1.);
#8426=VECTOR('',#28307,1.);
#8427=VECTOR('',#28308,1.);
#8428=VECTOR('',#28309,1.);
#8429=VECTOR('',#28314,1.);
#8430=VECTOR('',#28317,1.);
#8431=VECTOR('',#28318,1.);
#8432=VECTOR('',#28325,1.);
#8433=VECTOR('',#28326,1.);
#8434=VECTOR('',#28327,1.);
#8435=VECTOR('',#28328,1.);
#8436=VECTOR('',#28333,1.);
#8437=VECTOR('',#28336,1.);
#8438=VECTOR('',#28337,1.);
#8439=VECTOR('',#28344,1.);
#8440=VECTOR('',#28345,1.);
#8441=VECTOR('',#28346,1.);
#8442=VECTOR('',#28347,1.);
#8443=VECTOR('',#28352,1.);
#8444=VECTOR('',#28355,1.);
#8445=VECTOR('',#28356,1.);
#8446=VECTOR('',#28363,1.);
#8447=VECTOR('',#28364,1.);
#8448=VECTOR('',#28365,1.);
#8449=VECTOR('',#28366,1.);
#8450=VECTOR('',#28371,1.);
#8451=VECTOR('',#28374,1.);
#8452=VECTOR('',#28375,1.);
#8453=VECTOR('',#28382,1.);
#8454=VECTOR('',#28383,1.);
#8455=VECTOR('',#28384,1.);
#8456=VECTOR('',#28385,1.);
#8457=VECTOR('',#28390,1.);
#8458=VECTOR('',#28393,1.);
#8459=VECTOR('',#28394,1.);
#8460=VECTOR('',#28401,1.);
#8461=VECTOR('',#28402,1.);
#8462=VECTOR('',#28403,1.);
#8463=VECTOR('',#28404,1.);
#8464=VECTOR('',#28409,1.);
#8465=VECTOR('',#28412,1.);
#8466=VECTOR('',#28413,1.);
#8467=VECTOR('',#28420,1.);
#8468=VECTOR('',#28421,1.);
#8469=VECTOR('',#28422,1.);
#8470=VECTOR('',#28423,1.);
#8471=VECTOR('',#28428,1.);
#8472=VECTOR('',#28431,1.);
#8473=VECTOR('',#28432,1.);
#8474=VECTOR('',#28441,0.24);
#8475=VECTOR('',#28448,0.28);
#8476=VECTOR('',#28463,0.39);
#8477=VECTOR('',#28466,0.4);
#8478=VECTOR('',#28475,0.3);
#8479=VECTOR('',#28476,0.3);
#8480=VECTOR('',#28485,0.18);
#8481=VECTOR('',#28494,3.35);
#8482=VECTOR('',#28505,3.75);
#8483=VECTOR('',#28514,0.240000000000001);
#8484=VECTOR('',#28519,0.225000000000001);
#8485=VECTOR('',#28526,1.);
#8486=VECTOR('',#28529,1.);
#8487=VECTOR('',#28532,1.);
#8488=VECTOR('',#28533,1.);
#8489=VECTOR('',#28538,0.240000000000001);
#8490=VECTOR('',#28543,1.);
#8491=VECTOR('',#28546,1.);
#8492=VECTOR('',#28549,1.);
#8493=VECTOR('',#28552,1.);
#8494=VECTOR('',#28555,1.);
#8495=VECTOR('',#28556,1.);
#8496=VECTOR('',#28557,1.);
#8497=VECTOR('',#28560,1.);
#8498=VECTOR('',#28565,1.);
#8499=VECTOR('',#28566,1.);
#8500=VECTOR('',#28569,1.);
#8501=VECTOR('',#28574,1.);
#8502=VECTOR('',#28575,1.);
#8503=VECTOR('',#28578,1.);
#8504=VECTOR('',#28579,1.);
#8505=VECTOR('',#28580,1.);
#8506=VECTOR('',#28581,1.);
#8507=VECTOR('',#28584,1.);
#8508=VECTOR('',#28585,1.);
#8509=VECTOR('',#28586,1.);
#8510=VECTOR('',#28589,1.);
#8511=VECTOR('',#28596,1.);
#8512=VECTOR('',#28597,1.);
#8513=VECTOR('',#28598,1.);
#8514=VECTOR('',#28601,1.);
#8515=VECTOR('',#28608,1.);
#8516=VECTOR('',#28609,1.);
#8517=VECTOR('',#28612,1.);
#8518=VECTOR('',#28615,1.);
#8519=VECTOR('',#28618,1.);
#8520=VECTOR('',#28619,1.);
#8521=VECTOR('',#28620,1.);
#8522=VECTOR('',#28623,1.);
#8523=VECTOR('',#28628,1.);
#8524=VECTOR('',#28631,1.);
#8525=VECTOR('',#28634,1.);
#8526=VECTOR('',#28635,1.);
#8527=VECTOR('',#28638,1.);
#8528=VECTOR('',#28643,1.);
#8529=VECTOR('',#28644,1.);
#8530=VECTOR('',#28647,1.);
#8531=VECTOR('',#28652,1.);
#8532=VECTOR('',#28655,1.);
#8533=VECTOR('',#28658,1.);
#8534=VECTOR('',#28661,1.);
#8535=VECTOR('',#28664,1.);
#8536=VECTOR('',#28667,1.);
#8537=VECTOR('',#28670,1.);
#8538=VECTOR('',#28673,1.);
#8539=VECTOR('',#28682,0.21);
#8540=VECTOR('',#28687,0.305);
#8541=VECTOR('',#28694,0.4);
#8542=VECTOR('',#28697,0.305);
#8543=VECTOR('',#28702,0.2);
#8544=VECTOR('',#28705,0.2);
#8545=VECTOR('',#28712,0.2);
#8546=VECTOR('',#28715,0.2);
#8547=VECTOR('',#28718,0.2);
#8548=VECTOR('',#28721,0.2);
#8549=VECTOR('',#28724,0.2);
#8550=VECTOR('',#28727,0.2);
#8551=VECTOR('',#28730,0.2);
#8552=VECTOR('',#28733,0.2);
#8553=VECTOR('',#28736,0.2);
#8554=VECTOR('',#28739,0.2);
#8555=VECTOR('',#28742,0.2);
#8556=VECTOR('',#28745,0.2);
#8557=VECTOR('',#28748,0.2);
#8558=VECTOR('',#28751,0.15555);
#8559=VECTOR('',#28756,0.15555);
#8560=VECTOR('',#28759,0.15555);
#8561=VECTOR('',#28762,0.15555);
#8562=VECTOR('',#28765,0.15555);
#8563=VECTOR('',#28768,0.15555);
#8564=VECTOR('',#28771,0.15555);
#8565=VECTOR('',#28774,0.15555);
#8566=VECTOR('',#28777,0.15555);
#8567=VECTOR('',#28780,0.15555);
#8568=VECTOR('',#28783,0.15555);
#8569=VECTOR('',#28786,0.15555);
#8570=VECTOR('',#28789,0.15555);
#8571=VECTOR('',#28792,0.15555);
#8572=VECTOR('',#28795,0.15555);
#8573=VECTOR('',#28810,0.1);
#8574=VECTOR('',#28815,1.);
#8575=VECTOR('',#28816,1.);
#8576=VECTOR('',#28817,1.);
#8577=VECTOR('',#28818,1.);
#8578=VECTOR('',#28823,1.);
#8579=VECTOR('',#28826,1.);
#8580=VECTOR('',#28827,1.);
#8581=VECTOR('',#28834,1.);
#8582=VECTOR('',#28835,1.);
#8583=VECTOR('',#28836,1.);
#8584=VECTOR('',#28837,1.);
#8585=VECTOR('',#28842,1.);
#8586=VECTOR('',#28845,1.);
#8587=VECTOR('',#28846,1.);
#8588=VECTOR('',#28853,1.);
#8589=VECTOR('',#28854,1.);
#8590=VECTOR('',#28855,1.);
#8591=VECTOR('',#28856,1.);
#8592=VECTOR('',#28861,1.);
#8593=VECTOR('',#28864,1.);
#8594=VECTOR('',#28865,1.);
#8595=VECTOR('',#28872,1.);
#8596=VECTOR('',#28873,1.);
#8597=VECTOR('',#28874,1.);
#8598=VECTOR('',#28875,1.);
#8599=VECTOR('',#28880,1.);
#8600=VECTOR('',#28883,1.);
#8601=VECTOR('',#28884,1.);
#8602=VECTOR('',#28891,1.);
#8603=VECTOR('',#28892,1.);
#8604=VECTOR('',#28893,1.);
#8605=VECTOR('',#28894,1.);
#8606=VECTOR('',#28899,1.);
#8607=VECTOR('',#28902,1.);
#8608=VECTOR('',#28903,1.);
#8609=VECTOR('',#28910,1.);
#8610=VECTOR('',#28911,1.);
#8611=VECTOR('',#28912,1.);
#8612=VECTOR('',#28913,1.);
#8613=VECTOR('',#28918,1.);
#8614=VECTOR('',#28921,1.);
#8615=VECTOR('',#28922,1.);
#8616=VECTOR('',#28929,1.);
#8617=VECTOR('',#28930,1.);
#8618=VECTOR('',#28931,1.);
#8619=VECTOR('',#28932,1.);
#8620=VECTOR('',#28937,1.);
#8621=VECTOR('',#28940,1.);
#8622=VECTOR('',#28941,1.);
#8623=VECTOR('',#28948,1.);
#8624=VECTOR('',#28949,1.);
#8625=VECTOR('',#28950,1.);
#8626=VECTOR('',#28951,1.);
#8627=VECTOR('',#28956,1.);
#8628=VECTOR('',#28959,1.);
#8629=VECTOR('',#28960,1.);
#8630=VECTOR('',#28967,1.);
#8631=VECTOR('',#28968,1.);
#8632=VECTOR('',#28969,1.);
#8633=VECTOR('',#28970,1.);
#8634=VECTOR('',#28975,1.);
#8635=VECTOR('',#28978,1.);
#8636=VECTOR('',#28979,1.);
#8637=VECTOR('',#28986,1.);
#8638=VECTOR('',#28987,1.);
#8639=VECTOR('',#28988,1.);
#8640=VECTOR('',#28989,1.);
#8641=VECTOR('',#28994,1.);
#8642=VECTOR('',#28997,1.);
#8643=VECTOR('',#28998,1.);
#8644=VECTOR('',#29005,1.);
#8645=VECTOR('',#29006,1.);
#8646=VECTOR('',#29007,1.);
#8647=VECTOR('',#29008,1.);
#8648=VECTOR('',#29013,1.);
#8649=VECTOR('',#29016,1.);
#8650=VECTOR('',#29017,1.);
#8651=VECTOR('',#29024,1.);
#8652=VECTOR('',#29025,1.);
#8653=VECTOR('',#29026,1.);
#8654=VECTOR('',#29027,1.);
#8655=VECTOR('',#29032,1.);
#8656=VECTOR('',#29037,1.);
#8657=VECTOR('',#29038,1.);
#8658=VECTOR('',#29047,1.);
#8659=VECTOR('',#29048,1.);
#8660=VECTOR('',#29049,1.);
#8661=VECTOR('',#29050,1.);
#8662=VECTOR('',#29055,1.);
#8663=VECTOR('',#29058,1.);
#8664=VECTOR('',#29059,1.);
#8665=VECTOR('',#29066,1.);
#8666=VECTOR('',#29067,1.);
#8667=VECTOR('',#29068,1.);
#8668=VECTOR('',#29069,1.);
#8669=VECTOR('',#29074,1.);
#8670=VECTOR('',#29077,1.);
#8671=VECTOR('',#29078,1.);
#8672=VECTOR('',#29085,1.);
#8673=VECTOR('',#29086,1.);
#8674=VECTOR('',#29087,1.);
#8675=VECTOR('',#29088,1.);
#8676=VECTOR('',#29093,1.);
#8677=VECTOR('',#29096,1.);
#8678=VECTOR('',#29097,1.);
#8679=VECTOR('',#29104,1.);
#8680=VECTOR('',#29105,1.);
#8681=VECTOR('',#29106,1.);
#8682=VECTOR('',#29107,1.);
#8683=VECTOR('',#29112,1.);
#8684=VECTOR('',#29115,1.);
#8685=VECTOR('',#29116,1.);
#8686=VECTOR('',#29123,1.);
#8687=VECTOR('',#29124,1.);
#8688=VECTOR('',#29125,1.);
#8689=VECTOR('',#29126,1.);
#8690=VECTOR('',#29131,1.);
#8691=VECTOR('',#29134,1.);
#8692=VECTOR('',#29135,1.);
#8693=VECTOR('',#29142,1.);
#8694=VECTOR('',#29143,1.);
#8695=VECTOR('',#29144,1.);
#8696=VECTOR('',#29145,1.);
#8697=VECTOR('',#29150,1.);
#8698=VECTOR('',#29153,1.);
#8699=VECTOR('',#29154,1.);
#8700=VECTOR('',#29161,1.);
#8701=VECTOR('',#29162,1.);
#8702=VECTOR('',#29163,1.);
#8703=VECTOR('',#29164,1.);
#8704=VECTOR('',#29169,1.);
#8705=VECTOR('',#29172,1.);
#8706=VECTOR('',#29173,1.);
#8707=VECTOR('',#29180,1.);
#8708=VECTOR('',#29181,1.);
#8709=VECTOR('',#29182,1.);
#8710=VECTOR('',#29183,1.);
#8711=VECTOR('',#29188,1.);
#8712=VECTOR('',#29191,1.);
#8713=VECTOR('',#29192,1.);
#8714=VECTOR('',#29199,1.);
#8715=VECTOR('',#29200,1.);
#8716=VECTOR('',#29201,1.);
#8717=VECTOR('',#29202,1.);
#8718=VECTOR('',#29207,1.);
#8719=VECTOR('',#29210,1.);
#8720=VECTOR('',#29211,1.);
#8721=VECTOR('',#29218,1.);
#8722=VECTOR('',#29219,1.);
#8723=VECTOR('',#29220,1.);
#8724=VECTOR('',#29221,1.);
#8725=VECTOR('',#29226,1.);
#8726=VECTOR('',#29229,1.);
#8727=VECTOR('',#29230,1.);
#8728=VECTOR('',#29237,1.);
#8729=VECTOR('',#29238,1.);
#8730=VECTOR('',#29239,1.);
#8731=VECTOR('',#29240,1.);
#8732=VECTOR('',#29245,1.);
#8733=VECTOR('',#29248,1.);
#8734=VECTOR('',#29249,1.);
#8735=VECTOR('',#29256,1.);
#8736=VECTOR('',#29257,1.);
#8737=VECTOR('',#29258,1.);
#8738=VECTOR('',#29259,1.);
#8739=VECTOR('',#29264,1.);
#8740=VECTOR('',#29267,1.);
#8741=VECTOR('',#29268,1.);
#8742=VECTOR('',#29279,0.18);
#8743=VECTOR('',#29288,0.575);
#8744=VECTOR('',#29293,0.6);
#8745=VECTOR('',#29294,0.6);
#8746=VECTOR('',#29299,0.55);
#8747=VECTOR('',#29306,0.15);
#8748=VECTOR('',#29309,0.15);
#8749=VECTOR('',#29316,0.15);
#8750=VECTOR('',#29319,0.15);
#8751=VECTOR('',#29322,0.15);
#8752=VECTOR('',#29325,0.15);
#8753=VECTOR('',#29328,0.15);
#8754=VECTOR('',#29331,0.15);
#8755=VECTOR('',#29334,0.15);
#8756=VECTOR('',#29337,0.15);
#8757=VECTOR('',#29340,0.15);
#8758=VECTOR('',#29343,0.15);
#8759=VECTOR('',#29346,0.15);
#8760=VECTOR('',#29349,0.15);
#8761=VECTOR('',#29352,0.15);
#8762=VECTOR('',#29355,0.117775);
#8763=VECTOR('',#29360,0.117775);
#8764=VECTOR('',#29363,0.117775);
#8765=VECTOR('',#29366,0.117775);
#8766=VECTOR('',#29369,0.117775);
#8767=VECTOR('',#29372,0.117775);
#8768=VECTOR('',#29375,0.117775);
#8769=VECTOR('',#29378,0.117775);
#8770=VECTOR('',#29381,0.117775);
#8771=VECTOR('',#29384,0.117775);
#8772=VECTOR('',#29387,0.117775);
#8773=VECTOR('',#29390,0.117775);
#8774=VECTOR('',#29393,0.117775);
#8775=VECTOR('',#29396,0.117775);
#8776=VECTOR('',#29399,0.117775);
#8777=VECTOR('',#29416,1.);
#8778=VECTOR('',#29417,1.);
#8779=VECTOR('',#29420,1.);
#8780=VECTOR('',#29421,1.);
#8781=VECTOR('',#29424,1.);
#8782=VECTOR('',#29429,1.);
#8783=VECTOR('',#29430,1.);
#8784=VECTOR('',#29433,1.);
#8785=VECTOR('',#29434,1.);
#8786=VECTOR('',#29437,1.);
#8787=VECTOR('',#29442,1.);
#8788=VECTOR('',#29443,1.);
#8789=VECTOR('',#29446,1.);
#8790=VECTOR('',#29447,1.);
#8791=VECTOR('',#29450,1.);
#8792=VECTOR('',#29455,1.);
#8793=VECTOR('',#29456,1.);
#8794=VECTOR('',#29459,1.);
#8795=VECTOR('',#29460,1.);
#8796=VECTOR('',#29463,1.);
#8797=VECTOR('',#29468,1.);
#8798=VECTOR('',#29469,1.);
#8799=VECTOR('',#29472,1.);
#8800=VECTOR('',#29473,1.);
#8801=VECTOR('',#29476,1.);
#8802=VECTOR('',#29481,1.);
#8803=VECTOR('',#29482,1.);
#8804=VECTOR('',#29485,1.);
#8805=VECTOR('',#29486,1.);
#8806=VECTOR('',#29489,1.);
#8807=VECTOR('',#29494,1.);
#8808=VECTOR('',#29495,1.);
#8809=VECTOR('',#29498,1.);
#8810=VECTOR('',#29499,1.);
#8811=VECTOR('',#29502,1.);
#8812=VECTOR('',#29507,1.);
#8813=VECTOR('',#29508,1.);
#8814=VECTOR('',#29511,1.);
#8815=VECTOR('',#29512,1.);
#8816=VECTOR('',#29515,1.);
#8817=VECTOR('',#29520,1.);
#8818=VECTOR('',#29521,1.);
#8819=VECTOR('',#29524,1.);
#8820=VECTOR('',#29525,1.);
#8821=VECTOR('',#29528,1.);
#8822=VECTOR('',#29533,1.);
#8823=VECTOR('',#29534,1.);
#8824=VECTOR('',#29537,1.);
#8825=VECTOR('',#29538,1.);
#8826=VECTOR('',#29541,1.);
#8827=VECTOR('',#29546,1.);
#8828=VECTOR('',#29547,1.);
#8829=VECTOR('',#29550,1.);
#8830=VECTOR('',#29551,1.);
#8831=VECTOR('',#29554,1.);
#8832=VECTOR('',#29559,1.);
#8833=VECTOR('',#29560,1.);
#8834=VECTOR('',#29563,1.);
#8835=VECTOR('',#29564,1.);
#8836=VECTOR('',#29567,1.);
#8837=VECTOR('',#29572,1.);
#8838=VECTOR('',#29573,1.);
#8839=VECTOR('',#29576,1.);
#8840=VECTOR('',#29577,1.);
#8841=VECTOR('',#29580,1.);
#8842=VECTOR('',#29585,1.);
#8843=VECTOR('',#29586,1.);
#8844=VECTOR('',#29589,1.);
#8845=VECTOR('',#29590,1.);
#8846=VECTOR('',#29593,1.);
#8847=VECTOR('',#29598,1.);
#8848=VECTOR('',#29599,1.);
#8849=VECTOR('',#29602,1.);
#8850=VECTOR('',#29603,1.);
#8851=VECTOR('',#29606,1.);
#8852=VECTOR('',#29611,1.);
#8853=VECTOR('',#29612,1.);
#8854=VECTOR('',#29615,1.);
#8855=VECTOR('',#29616,1.);
#8856=VECTOR('',#29619,1.);
#8857=VECTOR('',#29624,1.);
#8858=VECTOR('',#29625,1.);
#8859=VECTOR('',#29628,1.);
#8860=VECTOR('',#29629,1.);
#8861=VECTOR('',#29632,1.);
#8862=VECTOR('',#29637,1.);
#8863=VECTOR('',#29638,1.);
#8864=VECTOR('',#29643,1.);
#8865=VECTOR('',#29644,1.);
#8866=VECTOR('',#29647,1.);
#8867=VECTOR('',#29652,1.);
#8868=VECTOR('',#29653,1.);
#8869=VECTOR('',#29656,1.);
#8870=VECTOR('',#29657,1.);
#8871=VECTOR('',#29660,1.);
#8872=VECTOR('',#29665,1.);
#8873=VECTOR('',#29666,1.);
#8874=VECTOR('',#29669,1.);
#8875=VECTOR('',#29670,1.);
#8876=VECTOR('',#29673,1.);
#8877=VECTOR('',#29678,1.);
#8878=VECTOR('',#29679,1.);
#8879=VECTOR('',#29682,1.);
#8880=VECTOR('',#29683,1.);
#8881=VECTOR('',#29686,1.);
#8882=VECTOR('',#29691,1.);
#8883=VECTOR('',#29692,1.);
#8884=VECTOR('',#29695,1.);
#8885=VECTOR('',#29696,1.);
#8886=VECTOR('',#29699,1.);
#8887=VECTOR('',#29704,1.);
#8888=VECTOR('',#29705,1.);
#8889=VECTOR('',#29708,1.);
#8890=VECTOR('',#29709,1.);
#8891=VECTOR('',#29712,1.);
#8892=VECTOR('',#29717,1.);
#8893=VECTOR('',#29718,1.);
#8894=VECTOR('',#29721,1.);
#8895=VECTOR('',#29722,1.);
#8896=VECTOR('',#29725,1.);
#8897=VECTOR('',#29730,1.);
#8898=VECTOR('',#29731,1.);
#8899=VECTOR('',#29734,1.);
#8900=VECTOR('',#29735,1.);
#8901=VECTOR('',#29738,1.);
#8902=VECTOR('',#29743,1.);
#8903=VECTOR('',#29744,1.);
#8904=VECTOR('',#29747,1.);
#8905=VECTOR('',#29748,1.);
#8906=VECTOR('',#29751,1.);
#8907=VECTOR('',#29756,1.);
#8908=VECTOR('',#29757,1.);
#8909=VECTOR('',#29760,1.);
#8910=VECTOR('',#29761,1.);
#8911=VECTOR('',#29764,1.);
#8912=VECTOR('',#29769,1.);
#8913=VECTOR('',#29770,1.);
#8914=VECTOR('',#29773,1.);
#8915=VECTOR('',#29774,1.);
#8916=VECTOR('',#29777,1.);
#8917=VECTOR('',#29782,1.);
#8918=VECTOR('',#29783,1.);
#8919=VECTOR('',#29786,1.);
#8920=VECTOR('',#29787,1.);
#8921=VECTOR('',#29790,1.);
#8922=VECTOR('',#29795,1.);
#8923=VECTOR('',#29796,1.);
#8924=VECTOR('',#29799,1.);
#8925=VECTOR('',#29800,1.);
#8926=VECTOR('',#29803,1.);
#8927=VECTOR('',#29808,1.);
#8928=VECTOR('',#29809,1.);
#8929=VECTOR('',#29812,1.);
#8930=VECTOR('',#29813,1.);
#8931=VECTOR('',#29816,1.);
#8932=VECTOR('',#29821,1.);
#8933=VECTOR('',#29822,1.);
#8934=VECTOR('',#29825,1.);
#8935=VECTOR('',#29826,1.);
#8936=VECTOR('',#29829,1.);
#8937=VECTOR('',#29834,1.);
#8938=VECTOR('',#29835,1.);
#8939=VECTOR('',#29838,1.);
#8940=VECTOR('',#29839,1.);
#8941=VECTOR('',#29842,1.);
#8942=VECTOR('',#29847,1.);
#8943=VECTOR('',#29848,1.);
#8944=VECTOR('',#29851,1.);
#8945=VECTOR('',#29852,1.);
#8946=VECTOR('',#29855,1.);
#8947=VECTOR('',#29860,1.);
#8948=VECTOR('',#29861,1.);
#8949=VECTOR('',#29864,1.);
#8950=VECTOR('',#29865,1.);
#8951=VECTOR('',#29868,1.);
#8952=VECTOR('',#29905,0.275);
#8953=VECTOR('',#29944,1.);
#8954=VECTOR('',#29947,1.);
#8955=VECTOR('',#29952,1.);
#8956=VECTOR('',#29953,1.);
#8957=VECTOR('',#29956,1.);
#8958=VECTOR('',#29963,0.2675);
#8959=VECTOR('',#29966,0.0577350269189626);
#8960=VECTOR('',#29971,1.);
#8961=VECTOR('',#29972,1.);
#8962=VECTOR('',#29973,1.);
#8963=VECTOR('',#29974,1.);
#8964=VECTOR('',#29977,1.);
#8965=VECTOR('',#29978,1.);
#8966=VECTOR('',#29979,1.);
#8967=VECTOR('',#29982,1.);
#8968=VECTOR('',#29983,1.);
#8969=VECTOR('',#29984,1.);
#8970=VECTOR('',#29987,1.);
#8971=VECTOR('',#29988,1.);
#8972=VECTOR('',#29989,1.);
#8973=VECTOR('',#29992,1.);
#8974=VECTOR('',#29993,1.);
#8975=VECTOR('',#29994,1.);
#8976=VECTOR('',#29997,1.);
#8977=VECTOR('',#29998,1.);
#8978=VECTOR('',#30007,0.132);
#8979=VECTOR('',#30016,0.155);
#8980=VECTOR('',#30025,0.15);
#8981=VECTOR('',#30028,0.15);
#8982=VECTOR('',#30035,0.15);
#8983=VECTOR('',#30038,0.15);
#8984=VECTOR('',#30041,0.15);
#8985=VECTOR('',#30044,0.15);
#8986=VECTOR('',#30047,0.15);
#8987=VECTOR('',#30050,0.15);
#8988=VECTOR('',#30053,0.15);
#8989=VECTOR('',#30056,0.15);
#8990=VECTOR('',#30059,0.15);
#8991=VECTOR('',#30062,0.15);
#8992=VECTOR('',#30065,0.15);
#8993=VECTOR('',#30068,0.15);
#8994=VECTOR('',#30071,0.15);
#8995=VECTOR('',#30074,0.15);
#8996=VECTOR('',#30077,0.15);
#8997=VECTOR('',#30080,0.15);
#8998=VECTOR('',#30083,0.15);
#8999=VECTOR('',#30086,0.15);
#9000=VECTOR('',#30089,0.15);
#9001=VECTOR('',#30092,0.15);
#9002=VECTOR('',#30095,0.15);
#9003=VECTOR('',#30098,0.15);
#9004=VECTOR('',#30101,0.15);
#9005=VECTOR('',#30104,0.15);
#9006=VECTOR('',#30107,0.15);
#9007=VECTOR('',#30110,0.15);
#9008=VECTOR('',#30113,0.15);
#9009=VECTOR('',#30116,0.15);
#9010=VECTOR('',#30119,0.15);
#9011=VECTOR('',#30122,0.15);
#9012=VECTOR('',#30125,0.15);
#9013=VECTOR('',#30128,0.15);
#9014=VECTOR('',#30131,0.15);
#9015=VECTOR('',#30134,0.15);
#9016=VECTOR('',#30137,0.15);
#9017=VECTOR('',#30140,0.15);
#9018=VECTOR('',#30143,0.15);
#9019=VECTOR('',#30146,0.15);
#9020=VECTOR('',#30149,0.15);
#9021=VECTOR('',#30152,0.15);
#9022=VECTOR('',#30155,0.15);
#9023=VECTOR('',#30158,0.15);
#9024=VECTOR('',#30161,0.15);
#9025=VECTOR('',#30164,0.15);
#9026=VECTOR('',#30167,0.15);
#9027=VECTOR('',#30170,0.15);
#9028=VECTOR('',#30173,0.15);
#9029=VECTOR('',#30176,0.15);
#9030=VECTOR('',#30179,0.15);
#9031=VECTOR('',#30182,0.15);
#9032=VECTOR('',#30185,0.15);
#9033=VECTOR('',#30188,0.15);
#9034=VECTOR('',#30191,0.15);
#9035=VECTOR('',#30194,0.15);
#9036=VECTOR('',#30197,0.15);
#9037=VECTOR('',#30200,0.15);
#9038=VECTOR('',#30203,0.15);
#9039=VECTOR('',#30206,0.117775);
#9040=VECTOR('',#30211,0.117775);
#9041=VECTOR('',#30214,0.117775);
#9042=VECTOR('',#30217,0.117775);
#9043=VECTOR('',#30220,0.117775);
#9044=VECTOR('',#30223,0.117775);
#9045=VECTOR('',#30226,0.117775);
#9046=VECTOR('',#30229,0.117775);
#9047=VECTOR('',#30232,0.117775);
#9048=VECTOR('',#30235,0.117775);
#9049=VECTOR('',#30238,0.117775);
#9050=VECTOR('',#30241,0.117775);
#9051=VECTOR('',#30244,0.117775);
#9052=VECTOR('',#30247,0.117775);
#9053=VECTOR('',#30250,0.117775);
#9054=VECTOR('',#30253,0.117775);
#9055=VECTOR('',#30256,0.117775);
#9056=VECTOR('',#30259,0.117775);
#9057=VECTOR('',#30262,0.117775);
#9058=VECTOR('',#30265,0.117775);
#9059=VECTOR('',#30268,0.117775);
#9060=VECTOR('',#30271,0.117775);
#9061=VECTOR('',#30274,0.117775);
#9062=VECTOR('',#30277,0.117775);
#9063=VECTOR('',#30280,0.117775);
#9064=VECTOR('',#30283,0.117775);
#9065=VECTOR('',#30286,0.117775);
#9066=VECTOR('',#30289,0.117775);
#9067=VECTOR('',#30292,0.117775);
#9068=VECTOR('',#30295,0.117775);
#9069=VECTOR('',#30298,0.117775);
#9070=VECTOR('',#30301,0.117775);
#9071=VECTOR('',#30304,0.117775);
#9072=VECTOR('',#30307,0.117775);
#9073=VECTOR('',#30310,0.117775);
#9074=VECTOR('',#30313,0.117775);
#9075=VECTOR('',#30316,0.117775);
#9076=VECTOR('',#30319,0.117775);
#9077=VECTOR('',#30322,0.117775);
#9078=VECTOR('',#30325,0.117775);
#9079=VECTOR('',#30328,0.117775);
#9080=VECTOR('',#30331,0.117775);
#9081=VECTOR('',#30334,0.117775);
#9082=VECTOR('',#30337,0.117775);
#9083=VECTOR('',#30340,0.117775);
#9084=VECTOR('',#30343,0.117775);
#9085=VECTOR('',#30346,0.117775);
#9086=VECTOR('',#30349,0.117775);
#9087=VECTOR('',#30352,0.117775);
#9088=VECTOR('',#30355,0.117775);
#9089=VECTOR('',#30358,0.117775);
#9090=VECTOR('',#30361,0.117775);
#9091=VECTOR('',#30364,0.117775);
#9092=VECTOR('',#30367,0.117775);
#9093=VECTOR('',#30370,0.117775);
#9094=VECTOR('',#30373,0.117775);
#9095=VECTOR('',#30376,0.117775);
#9096=VECTOR('',#30379,0.117775);
#9097=VECTOR('',#30382,0.117775);
#9098=VECTOR('',#30399,1.);
#9099=VECTOR('',#30400,1.);
#9100=VECTOR('',#30403,1.);
#9101=VECTOR('',#30404,1.);
#9102=VECTOR('',#30407,1.);
#9103=VECTOR('',#30412,1.);
#9104=VECTOR('',#30413,1.);
#9105=VECTOR('',#30416,1.);
#9106=VECTOR('',#30417,1.);
#9107=VECTOR('',#30420,1.);
#9108=VECTOR('',#30425,1.);
#9109=VECTOR('',#30426,1.);
#9110=VECTOR('',#30429,1.);
#9111=VECTOR('',#30430,1.);
#9112=VECTOR('',#30433,1.);
#9113=VECTOR('',#30438,1.);
#9114=VECTOR('',#30439,1.);
#9115=VECTOR('',#30442,1.);
#9116=VECTOR('',#30443,1.);
#9117=VECTOR('',#30446,1.);
#9118=VECTOR('',#30451,1.);
#9119=VECTOR('',#30452,1.);
#9120=VECTOR('',#30455,1.);
#9121=VECTOR('',#30456,1.);
#9122=VECTOR('',#30459,1.);
#9123=VECTOR('',#30464,1.);
#9124=VECTOR('',#30465,1.);
#9125=VECTOR('',#30468,1.);
#9126=VECTOR('',#30469,1.);
#9127=VECTOR('',#30472,1.);
#9128=VECTOR('',#30477,1.);
#9129=VECTOR('',#30478,1.);
#9130=VECTOR('',#30481,1.);
#9131=VECTOR('',#30482,1.);
#9132=VECTOR('',#30485,1.);
#9133=VECTOR('',#30490,1.);
#9134=VECTOR('',#30491,1.);
#9135=VECTOR('',#30494,1.);
#9136=VECTOR('',#30495,1.);
#9137=VECTOR('',#30498,1.);
#9138=VECTOR('',#30503,1.);
#9139=VECTOR('',#30504,1.);
#9140=VECTOR('',#30507,1.);
#9141=VECTOR('',#30508,1.);
#9142=VECTOR('',#30511,1.);
#9143=VECTOR('',#30516,1.);
#9144=VECTOR('',#30517,1.);
#9145=VECTOR('',#30520,1.);
#9146=VECTOR('',#30521,1.);
#9147=VECTOR('',#30524,1.);
#9148=VECTOR('',#30529,1.);
#9149=VECTOR('',#30530,1.);
#9150=VECTOR('',#30533,1.);
#9151=VECTOR('',#30534,1.);
#9152=VECTOR('',#30537,1.);
#9153=VECTOR('',#30542,1.);
#9154=VECTOR('',#30543,1.);
#9155=VECTOR('',#30546,1.);
#9156=VECTOR('',#30547,1.);
#9157=VECTOR('',#30550,1.);
#9158=VECTOR('',#30555,1.);
#9159=VECTOR('',#30556,1.);
#9160=VECTOR('',#30559,1.);
#9161=VECTOR('',#30560,1.);
#9162=VECTOR('',#30563,1.);
#9163=VECTOR('',#30568,1.);
#9164=VECTOR('',#30569,1.);
#9165=VECTOR('',#30572,1.);
#9166=VECTOR('',#30573,1.);
#9167=VECTOR('',#30576,1.);
#9168=VECTOR('',#30581,1.);
#9169=VECTOR('',#30582,1.);
#9170=VECTOR('',#30585,1.);
#9171=VECTOR('',#30586,1.);
#9172=VECTOR('',#30589,1.);
#9173=VECTOR('',#30594,1.);
#9174=VECTOR('',#30595,1.);
#9175=VECTOR('',#30598,1.);
#9176=VECTOR('',#30599,1.);
#9177=VECTOR('',#30602,1.);
#9178=VECTOR('',#30607,1.);
#9179=VECTOR('',#30608,1.);
#9180=VECTOR('',#30611,1.);
#9181=VECTOR('',#30612,1.);
#9182=VECTOR('',#30615,1.);
#9183=VECTOR('',#30620,1.);
#9184=VECTOR('',#30621,1.);
#9185=VECTOR('',#30626,1.);
#9186=VECTOR('',#30627,1.);
#9187=VECTOR('',#30630,1.);
#9188=VECTOR('',#30635,1.);
#9189=VECTOR('',#30636,1.);
#9190=VECTOR('',#30639,1.);
#9191=VECTOR('',#30640,1.);
#9192=VECTOR('',#30643,1.);
#9193=VECTOR('',#30648,1.);
#9194=VECTOR('',#30649,1.);
#9195=VECTOR('',#30652,1.);
#9196=VECTOR('',#30653,1.);
#9197=VECTOR('',#30656,1.);
#9198=VECTOR('',#30661,1.);
#9199=VECTOR('',#30662,1.);
#9200=VECTOR('',#30665,1.);
#9201=VECTOR('',#30666,1.);
#9202=VECTOR('',#30669,1.);
#9203=VECTOR('',#30674,1.);
#9204=VECTOR('',#30675,1.);
#9205=VECTOR('',#30678,1.);
#9206=VECTOR('',#30679,1.);
#9207=VECTOR('',#30682,1.);
#9208=VECTOR('',#30687,1.);
#9209=VECTOR('',#30688,1.);
#9210=VECTOR('',#30691,1.);
#9211=VECTOR('',#30692,1.);
#9212=VECTOR('',#30695,1.);
#9213=VECTOR('',#30700,1.);
#9214=VECTOR('',#30701,1.);
#9215=VECTOR('',#30704,1.);
#9216=VECTOR('',#30705,1.);
#9217=VECTOR('',#30708,1.);
#9218=VECTOR('',#30713,1.);
#9219=VECTOR('',#30714,1.);
#9220=VECTOR('',#30717,1.);
#9221=VECTOR('',#30718,1.);
#9222=VECTOR('',#30721,1.);
#9223=VECTOR('',#30726,1.);
#9224=VECTOR('',#30727,1.);
#9225=VECTOR('',#30730,1.);
#9226=VECTOR('',#30731,1.);
#9227=VECTOR('',#30734,1.);
#9228=VECTOR('',#30739,1.);
#9229=VECTOR('',#30740,1.);
#9230=VECTOR('',#30743,1.);
#9231=VECTOR('',#30744,1.);
#9232=VECTOR('',#30747,1.);
#9233=VECTOR('',#30752,1.);
#9234=VECTOR('',#30753,1.);
#9235=VECTOR('',#30756,1.);
#9236=VECTOR('',#30757,1.);
#9237=VECTOR('',#30760,1.);
#9238=VECTOR('',#30765,1.);
#9239=VECTOR('',#30766,1.);
#9240=VECTOR('',#30769,1.);
#9241=VECTOR('',#30770,1.);
#9242=VECTOR('',#30773,1.);
#9243=VECTOR('',#30778,1.);
#9244=VECTOR('',#30779,1.);
#9245=VECTOR('',#30782,1.);
#9246=VECTOR('',#30783,1.);
#9247=VECTOR('',#30786,1.);
#9248=VECTOR('',#30791,1.);
#9249=VECTOR('',#30792,1.);
#9250=VECTOR('',#30795,1.);
#9251=VECTOR('',#30796,1.);
#9252=VECTOR('',#30799,1.);
#9253=VECTOR('',#30804,1.);
#9254=VECTOR('',#30805,1.);
#9255=VECTOR('',#30808,1.);
#9256=VECTOR('',#30809,1.);
#9257=VECTOR('',#30812,1.);
#9258=VECTOR('',#30817,1.);
#9259=VECTOR('',#30818,1.);
#9260=VECTOR('',#30821,1.);
#9261=VECTOR('',#30822,1.);
#9262=VECTOR('',#30825,1.);
#9263=VECTOR('',#30830,1.);
#9264=VECTOR('',#30831,1.);
#9265=VECTOR('',#30834,1.);
#9266=VECTOR('',#30835,1.);
#9267=VECTOR('',#30838,1.);
#9268=VECTOR('',#30843,1.);
#9269=VECTOR('',#30844,1.);
#9270=VECTOR('',#30847,1.);
#9271=VECTOR('',#30848,1.);
#9272=VECTOR('',#30851,1.);
#9273=VECTOR('',#30888,0.275);
#9274=VECTOR('',#30927,1.);
#9275=VECTOR('',#30930,1.);
#9276=VECTOR('',#30935,1.);
#9277=VECTOR('',#30936,1.);
#9278=VECTOR('',#30939,1.);
#9279=VECTOR('',#30946,0.2675);
#9280=VECTOR('',#30949,0.0577350269189626);
#9281=VECTOR('',#30954,1.);
#9282=VECTOR('',#30955,1.);
#9283=VECTOR('',#30956,1.);
#9284=VECTOR('',#30957,1.);
#9285=VECTOR('',#30960,1.);
#9286=VECTOR('',#30961,1.);
#9287=VECTOR('',#30962,1.);
#9288=VECTOR('',#30965,1.);
#9289=VECTOR('',#30966,1.);
#9290=VECTOR('',#30967,1.);
#9291=VECTOR('',#30970,1.);
#9292=VECTOR('',#30971,1.);
#9293=VECTOR('',#30972,1.);
#9294=VECTOR('',#30975,1.);
#9295=VECTOR('',#30976,1.);
#9296=VECTOR('',#30977,1.);
#9297=VECTOR('',#30980,1.);
#9298=VECTOR('',#30981,1.);
#9299=VECTOR('',#30990,0.132);
#9300=VECTOR('',#30999,0.155);
#9301=VECTOR('',#31008,0.25);
#9302=VECTOR('',#31011,0.25);
#9303=VECTOR('',#31018,0.25);
#9304=VECTOR('',#31021,0.25);
#9305=VECTOR('',#31024,0.25);
#9306=VECTOR('',#31027,0.25);
#9307=VECTOR('',#31030,0.25);
#9308=VECTOR('',#31033,0.25);
#9309=VECTOR('',#31036,0.25);
#9310=VECTOR('',#31039,0.25);
#9311=VECTOR('',#31042,0.25);
#9312=VECTOR('',#31045,0.25);
#9313=VECTOR('',#31048,0.25);
#9314=VECTOR('',#31051,0.25);
#9315=VECTOR('',#31054,0.25);
#9316=VECTOR('',#31057,0.25);
#9317=VECTOR('',#31060,0.25);
#9318=VECTOR('',#31063,0.25);
#9319=VECTOR('',#31066,0.25);
#9320=VECTOR('',#31069,0.199475);
#9321=VECTOR('',#31074,0.199475);
#9322=VECTOR('',#31077,0.199475);
#9323=VECTOR('',#31080,0.199475);
#9324=VECTOR('',#31083,0.199475);
#9325=VECTOR('',#31086,0.199475);
#9326=VECTOR('',#31089,0.199475);
#9327=VECTOR('',#31092,0.199475);
#9328=VECTOR('',#31095,0.199475);
#9329=VECTOR('',#31098,0.199475);
#9330=VECTOR('',#31101,0.199475);
#9331=VECTOR('',#31104,0.199475);
#9332=VECTOR('',#31107,0.199475);
#9333=VECTOR('',#31110,0.199475);
#9334=VECTOR('',#31113,0.199475);
#9335=VECTOR('',#31116,0.199475);
#9336=VECTOR('',#31119,0.199475);
#9337=VECTOR('',#31122,0.199475);
#9338=VECTOR('',#31125,0.199475);
#9339=VECTOR('',#31142,1.);
#9340=VECTOR('',#31143,1.);
#9341=VECTOR('',#31146,1.);
#9342=VECTOR('',#31147,1.);
#9343=VECTOR('',#31150,1.);
#9344=VECTOR('',#31155,1.);
#9345=VECTOR('',#31156,1.);
#9346=VECTOR('',#31159,1.);
#9347=VECTOR('',#31160,1.);
#9348=VECTOR('',#31163,1.);
#9349=VECTOR('',#31168,1.);
#9350=VECTOR('',#31169,1.);
#9351=VECTOR('',#31172,1.);
#9352=VECTOR('',#31173,1.);
#9353=VECTOR('',#31176,1.);
#9354=VECTOR('',#31181,1.);
#9355=VECTOR('',#31182,1.);
#9356=VECTOR('',#31185,1.);
#9357=VECTOR('',#31186,1.);
#9358=VECTOR('',#31189,1.);
#9359=VECTOR('',#31194,1.);
#9360=VECTOR('',#31195,1.);
#9361=VECTOR('',#31198,1.);
#9362=VECTOR('',#31199,1.);
#9363=VECTOR('',#31202,1.);
#9364=VECTOR('',#31207,1.);
#9365=VECTOR('',#31208,1.);
#9366=VECTOR('',#31211,1.);
#9367=VECTOR('',#31212,1.);
#9368=VECTOR('',#31215,1.);
#9369=VECTOR('',#31220,1.);
#9370=VECTOR('',#31221,1.);
#9371=VECTOR('',#31224,1.);
#9372=VECTOR('',#31225,1.);
#9373=VECTOR('',#31228,1.);
#9374=VECTOR('',#31233,1.);
#9375=VECTOR('',#31234,1.);
#9376=VECTOR('',#31237,1.);
#9377=VECTOR('',#31238,1.);
#9378=VECTOR('',#31241,1.);
#9379=VECTOR('',#31246,1.);
#9380=VECTOR('',#31247,1.);
#9381=VECTOR('',#31250,1.);
#9382=VECTOR('',#31251,1.);
#9383=VECTOR('',#31254,1.);
#9384=VECTOR('',#31259,1.);
#9385=VECTOR('',#31260,1.);
#9386=VECTOR('',#31263,1.);
#9387=VECTOR('',#31264,1.);
#9388=VECTOR('',#31267,1.);
#9389=VECTOR('',#31272,1.);
#9390=VECTOR('',#31273,1.);
#9391=VECTOR('',#31276,1.);
#9392=VECTOR('',#31277,1.);
#9393=VECTOR('',#31280,1.);
#9394=VECTOR('',#31285,1.);
#9395=VECTOR('',#31286,1.);
#9396=VECTOR('',#31289,1.);
#9397=VECTOR('',#31290,1.);
#9398=VECTOR('',#31293,1.);
#9399=VECTOR('',#31298,1.);
#9400=VECTOR('',#31299,1.);
#9401=VECTOR('',#31302,1.);
#9402=VECTOR('',#31303,1.);
#9403=VECTOR('',#31306,1.);
#9404=VECTOR('',#31311,1.);
#9405=VECTOR('',#31312,1.);
#9406=VECTOR('',#31315,1.);
#9407=VECTOR('',#31316,1.);
#9408=VECTOR('',#31319,1.);
#9409=VECTOR('',#31324,1.);
#9410=VECTOR('',#31325,1.);
#9411=VECTOR('',#31328,1.);
#9412=VECTOR('',#31329,1.);
#9413=VECTOR('',#31332,1.);
#9414=VECTOR('',#31337,1.);
#9415=VECTOR('',#31338,1.);
#9416=VECTOR('',#31341,1.);
#9417=VECTOR('',#31342,1.);
#9418=VECTOR('',#31345,1.);
#9419=VECTOR('',#31350,1.);
#9420=VECTOR('',#31351,1.);
#9421=VECTOR('',#31354,1.);
#9422=VECTOR('',#31355,1.);
#9423=VECTOR('',#31358,1.);
#9424=VECTOR('',#31363,1.);
#9425=VECTOR('',#31364,1.);
#9426=VECTOR('',#31369,1.);
#9427=VECTOR('',#31370,1.);
#9428=VECTOR('',#31373,1.);
#9429=VECTOR('',#31378,1.);
#9430=VECTOR('',#31379,1.);
#9431=VECTOR('',#31382,1.);
#9432=VECTOR('',#31383,1.);
#9433=VECTOR('',#31386,1.);
#9434=VECTOR('',#31391,1.);
#9435=VECTOR('',#31392,1.);
#9436=VECTOR('',#31395,1.);
#9437=VECTOR('',#31396,1.);
#9438=VECTOR('',#31399,1.);
#9439=VECTOR('',#31404,1.);
#9440=VECTOR('',#31405,1.);
#9441=VECTOR('',#31408,1.);
#9442=VECTOR('',#31409,1.);
#9443=VECTOR('',#31412,1.);
#9444=VECTOR('',#31417,1.);
#9445=VECTOR('',#31418,1.);
#9446=VECTOR('',#31421,1.);
#9447=VECTOR('',#31422,1.);
#9448=VECTOR('',#31425,1.);
#9449=VECTOR('',#31430,1.);
#9450=VECTOR('',#31431,1.);
#9451=VECTOR('',#31434,1.);
#9452=VECTOR('',#31435,1.);
#9453=VECTOR('',#31438,1.);
#9454=VECTOR('',#31443,1.);
#9455=VECTOR('',#31444,1.);
#9456=VECTOR('',#31447,1.);
#9457=VECTOR('',#31448,1.);
#9458=VECTOR('',#31451,1.);
#9459=VECTOR('',#31456,1.);
#9460=VECTOR('',#31457,1.);
#9461=VECTOR('',#31460,1.);
#9462=VECTOR('',#31461,1.);
#9463=VECTOR('',#31464,1.);
#9464=VECTOR('',#31469,1.);
#9465=VECTOR('',#31470,1.);
#9466=VECTOR('',#31473,1.);
#9467=VECTOR('',#31474,1.);
#9468=VECTOR('',#31477,1.);
#9469=VECTOR('',#31482,1.);
#9470=VECTOR('',#31483,1.);
#9471=VECTOR('',#31486,1.);
#9472=VECTOR('',#31487,1.);
#9473=VECTOR('',#31490,1.);
#9474=VECTOR('',#31495,1.);
#9475=VECTOR('',#31496,1.);
#9476=VECTOR('',#31499,1.);
#9477=VECTOR('',#31500,1.);
#9478=VECTOR('',#31503,1.);
#9479=VECTOR('',#31508,1.);
#9480=VECTOR('',#31509,1.);
#9481=VECTOR('',#31512,1.);
#9482=VECTOR('',#31513,1.);
#9483=VECTOR('',#31516,1.);
#9484=VECTOR('',#31521,1.);
#9485=VECTOR('',#31522,1.);
#9486=VECTOR('',#31525,1.);
#9487=VECTOR('',#31526,1.);
#9488=VECTOR('',#31529,1.);
#9489=VECTOR('',#31534,1.);
#9490=VECTOR('',#31535,1.);
#9491=VECTOR('',#31538,1.);
#9492=VECTOR('',#31539,1.);
#9493=VECTOR('',#31542,1.);
#9494=VECTOR('',#31547,1.);
#9495=VECTOR('',#31548,1.);
#9496=VECTOR('',#31551,1.);
#9497=VECTOR('',#31552,1.);
#9498=VECTOR('',#31555,1.);
#9499=VECTOR('',#31560,1.);
#9500=VECTOR('',#31561,1.);
#9501=VECTOR('',#31564,1.);
#9502=VECTOR('',#31565,1.);
#9503=VECTOR('',#31568,1.);
#9504=VECTOR('',#31573,1.);
#9505=VECTOR('',#31574,1.);
#9506=VECTOR('',#31577,1.);
#9507=VECTOR('',#31578,1.);
#9508=VECTOR('',#31581,1.);
#9509=VECTOR('',#31586,1.);
#9510=VECTOR('',#31587,1.);
#9511=VECTOR('',#31590,1.);
#9512=VECTOR('',#31591,1.);
#9513=VECTOR('',#31594,1.);
#9514=VECTOR('',#31631,0.425);
#9515=VECTOR('',#31670,1.);
#9516=VECTOR('',#31673,1.);
#9517=VECTOR('',#31678,1.);
#9518=VECTOR('',#31679,1.);
#9519=VECTOR('',#31682,1.);
#9520=VECTOR('',#31689,0.4175);
#9521=VECTOR('',#31692,0.0923760430703401);
#9522=VECTOR('',#31697,1.);
#9523=VECTOR('',#31698,1.);
#9524=VECTOR('',#31699,1.);
#9525=VECTOR('',#31700,1.);
#9526=VECTOR('',#31703,1.);
#9527=VECTOR('',#31704,1.);
#9528=VECTOR('',#31705,1.);
#9529=VECTOR('',#31708,1.);
#9530=VECTOR('',#31709,1.);
#9531=VECTOR('',#31710,1.);
#9532=VECTOR('',#31713,1.);
#9533=VECTOR('',#31714,1.);
#9534=VECTOR('',#31715,1.);
#9535=VECTOR('',#31718,1.);
#9536=VECTOR('',#31719,1.);
#9537=VECTOR('',#31720,1.);
#9538=VECTOR('',#31723,1.);
#9539=VECTOR('',#31724,1.);
#9540=VECTOR('',#31733,0.22);
#9541=VECTOR('',#31742,0.255);
#9542=VERTEX_POINT('',#31818);
#9543=VERTEX_POINT('',#31819);
#9544=VERTEX_POINT('',#31821);
#9545=VERTEX_POINT('',#31823);
#9546=VERTEX_POINT('',#31827);
#9547=VERTEX_POINT('',#31828);
#9548=VERTEX_POINT('',#31833);
#9549=VERTEX_POINT('',#31834);
#9550=VERTEX_POINT('',#31839);
#9551=VERTEX_POINT('',#31840);
#9552=VERTEX_POINT('',#31845);
#9553=VERTEX_POINT('',#31846);
#9554=VERTEX_POINT('',#31851);
#9555=VERTEX_POINT('',#31852);
#9556=VERTEX_POINT('',#31857);
#9557=VERTEX_POINT('',#31858);
#9558=VERTEX_POINT('',#31866);
#9559=VERTEX_POINT('',#31868);
#9560=VERTEX_POINT('',#31872);
#9561=VERTEX_POINT('',#31876);
#9562=VERTEX_POINT('',#31880);
#9563=VERTEX_POINT('',#31884);
#9564=VERTEX_POINT('',#31886);
#9565=VERTEX_POINT('',#31888);
#9566=VERTEX_POINT('',#31890);
#9567=VERTEX_POINT('',#31892);
#9568=VERTEX_POINT('',#31894);
#9569=VERTEX_POINT('',#31896);
#9570=VERTEX_POINT('',#31899);
#9571=VERTEX_POINT('',#31901);
#9572=VERTEX_POINT('',#31905);
#9573=VERTEX_POINT('',#31909);
#9574=VERTEX_POINT('',#31913);
#9575=VERTEX_POINT('',#31917);
#9576=VERTEX_POINT('',#31918);
#9577=VERTEX_POINT('',#31923);
#9578=VERTEX_POINT('',#31924);
#9579=VERTEX_POINT('',#31929);
#9580=VERTEX_POINT('',#31930);
#9581=VERTEX_POINT('',#31938);
#9582=VERTEX_POINT('',#31940);
#9583=VERTEX_POINT('',#31944);
#9584=VERTEX_POINT('',#31948);
#9585=VERTEX_POINT('',#31952);
#9586=VERTEX_POINT('',#31962);
#9587=VERTEX_POINT('',#31963);
#9588=VERTEX_POINT('',#31965);
#9589=VERTEX_POINT('',#31967);
#9590=VERTEX_POINT('',#31971);
#9591=VERTEX_POINT('',#31972);
#9592=VERTEX_POINT('',#31977);
#9593=VERTEX_POINT('',#31978);
#9594=VERTEX_POINT('',#31983);
#9595=VERTEX_POINT('',#31984);
#9596=VERTEX_POINT('',#31989);
#9597=VERTEX_POINT('',#31990);
#9598=VERTEX_POINT('',#31995);
#9599=VERTEX_POINT('',#31996);
#9600=VERTEX_POINT('',#32001);
#9601=VERTEX_POINT('',#32002);
#9602=VERTEX_POINT('',#32010);
#9603=VERTEX_POINT('',#32012);
#9604=VERTEX_POINT('',#32016);
#9605=VERTEX_POINT('',#32020);
#9606=VERTEX_POINT('',#32024);
#9607=VERTEX_POINT('',#32028);
#9608=VERTEX_POINT('',#32030);
#9609=VERTEX_POINT('',#32032);
#9610=VERTEX_POINT('',#32034);
#9611=VERTEX_POINT('',#32036);
#9612=VERTEX_POINT('',#32038);
#9613=VERTEX_POINT('',#32040);
#9614=VERTEX_POINT('',#32052);
#9615=VERTEX_POINT('',#32053);
#9616=VERTEX_POINT('',#32058);
#9617=VERTEX_POINT('',#32059);
#9618=VERTEX_POINT('',#32064);
#9619=VERTEX_POINT('',#32065);
#9620=VERTEX_POINT('',#32079);
#9621=VERTEX_POINT('',#32081);
#9622=VERTEX_POINT('',#32085);
#9623=VERTEX_POINT('',#32089);
#9624=VERTEX_POINT('',#32091);
#9625=VERTEX_POINT('',#32095);
#9626=VERTEX_POINT('',#32099);
#9627=VERTEX_POINT('',#32101);
#9628=VERTEX_POINT('',#32105);
#9629=VERTEX_POINT('',#32109);
#9630=VERTEX_POINT('',#32111);
#9631=VERTEX_POINT('',#32115);
#9632=VERTEX_POINT('',#32119);
#9633=VERTEX_POINT('',#32121);
#9634=VERTEX_POINT('',#32125);
#9635=VERTEX_POINT('',#32129);
#9636=VERTEX_POINT('',#32131);
#9637=VERTEX_POINT('',#32135);
#9638=VERTEX_POINT('',#32139);
#9639=VERTEX_POINT('',#32141);
#9640=VERTEX_POINT('',#32145);
#9641=VERTEX_POINT('',#32149);
#9642=VERTEX_POINT('',#32153);
#9643=VERTEX_POINT('',#32157);
#9644=VERTEX_POINT('',#32162);
#9645=VERTEX_POINT('',#32166);
#9646=VERTEX_POINT('',#32170);
#9647=VERTEX_POINT('',#32175);
#9648=VERTEX_POINT('',#32179);
#9649=VERTEX_POINT('',#32183);
#9650=VERTEX_POINT('',#32188);
#9651=VERTEX_POINT('',#32192);
#9652=VERTEX_POINT('',#32196);
#9653=VERTEX_POINT('',#32201);
#9654=VERTEX_POINT('',#32205);
#9655=VERTEX_POINT('',#32209);
#9656=VERTEX_POINT('',#32214);
#9657=VERTEX_POINT('',#32218);
#9658=VERTEX_POINT('',#32222);
#9659=VERTEX_POINT('',#32227);
#9660=VERTEX_POINT('',#32231);
#9661=VERTEX_POINT('',#32235);
#9662=VERTEX_POINT('',#32250);
#9663=VERTEX_POINT('',#32251);
#9664=VERTEX_POINT('',#32253);
#9665=VERTEX_POINT('',#32255);
#9666=VERTEX_POINT('',#32259);
#9667=VERTEX_POINT('',#32261);
#9668=VERTEX_POINT('',#32265);
#9669=VERTEX_POINT('',#32266);
#9670=VERTEX_POINT('',#32271);
#9671=VERTEX_POINT('',#32272);
#9672=VERTEX_POINT('',#32277);
#9673=VERTEX_POINT('',#32278);
#9674=VERTEX_POINT('',#32286);
#9675=VERTEX_POINT('',#32288);
#9676=VERTEX_POINT('',#32292);
#9677=VERTEX_POINT('',#32296);
#9678=VERTEX_POINT('',#32300);
#9679=VERTEX_POINT('',#32302);
#9680=VERTEX_POINT('',#32304);
#9681=VERTEX_POINT('',#32306);
#9682=VERTEX_POINT('',#32308);
#9683=VERTEX_POINT('',#32310);
#9684=VERTEX_POINT('',#32312);
#9685=VERTEX_POINT('',#32315);
#9686=VERTEX_POINT('',#32317);
#9687=VERTEX_POINT('',#32319);
#9688=VERTEX_POINT('',#32321);
#9689=VERTEX_POINT('',#32325);
#9690=VERTEX_POINT('',#32327);
#9691=VERTEX_POINT('',#32330);
#9692=VERTEX_POINT('',#32332);
#9693=VERTEX_POINT('',#32334);
#9694=VERTEX_POINT('',#32337);
#9695=VERTEX_POINT('',#32339);
#9696=VERTEX_POINT('',#32341);
#9697=VERTEX_POINT('',#32345);
#9698=VERTEX_POINT('',#32347);
#9699=VERTEX_POINT('',#32351);
#9700=VERTEX_POINT('',#32353);
#9701=VERTEX_POINT('',#32357);
#9702=VERTEX_POINT('',#32361);
#9703=VERTEX_POINT('',#32362);
#9704=VERTEX_POINT('',#32375);
#9705=VERTEX_POINT('',#32377);
#9706=VERTEX_POINT('',#32379);
#9707=VERTEX_POINT('',#32383);
#9708=VERTEX_POINT('',#32387);
#9709=VERTEX_POINT('',#32391);
#9710=VERTEX_POINT('',#32395);
#9711=VERTEX_POINT('',#32397);
#9712=VERTEX_POINT('',#32401);
#9713=VERTEX_POINT('',#32402);
#9714=VERTEX_POINT('',#32407);
#9715=VERTEX_POINT('',#32408);
#9716=VERTEX_POINT('',#32416);
#9717=VERTEX_POINT('',#32418);
#9718=VERTEX_POINT('',#32422);
#9719=VERTEX_POINT('',#32426);
#9720=VERTEX_POINT('',#32434);
#9721=VERTEX_POINT('',#32435);
#9722=VERTEX_POINT('',#32440);
#9723=VERTEX_POINT('',#32444);
#9724=VERTEX_POINT('',#32448);
#9725=VERTEX_POINT('',#32449);
#9726=VERTEX_POINT('',#32454);
#9727=VERTEX_POINT('',#32455);
#9728=VERTEX_POINT('',#32467);
#9729=VERTEX_POINT('',#32469);
#9730=VERTEX_POINT('',#32471);
#9731=VERTEX_POINT('',#32473);
#9732=VERTEX_POINT('',#32475);
#9733=VERTEX_POINT('',#32477);
#9734=VERTEX_POINT('',#32479);
#9735=VERTEX_POINT('',#32481);
#9736=VERTEX_POINT('',#32483);
#9737=VERTEX_POINT('',#32485);
#9738=VERTEX_POINT('',#32488);
#9739=VERTEX_POINT('',#32492);
#9740=VERTEX_POINT('',#32496);
#9741=VERTEX_POINT('',#32498);
#9742=VERTEX_POINT('',#32502);
#9743=VERTEX_POINT('',#32506);
#9744=VERTEX_POINT('',#32511);
#9745=VERTEX_POINT('',#32513);
#9746=VERTEX_POINT('',#32517);
#9747=VERTEX_POINT('',#32523);
#9748=VERTEX_POINT('',#32525);
#9749=VERTEX_POINT('',#32529);
#9750=VERTEX_POINT('',#32535);
#9751=VERTEX_POINT('',#32537);
#9752=VERTEX_POINT('',#32541);
#9753=VERTEX_POINT('',#32547);
#9754=VERTEX_POINT('',#32551);
#9755=VERTEX_POINT('',#32555);
#9756=VERTEX_POINT('',#32559);
#9757=VERTEX_POINT('',#32563);
#9758=VERTEX_POINT('',#32567);
#9759=VERTEX_POINT('',#32571);
#9760=VERTEX_POINT('',#32573);
#9761=VERTEX_POINT('',#32577);
#9762=VERTEX_POINT('',#32578);
#9763=VERTEX_POINT('',#32585);
#9764=VERTEX_POINT('',#32586);
#9765=VERTEX_POINT('',#32591);
#9766=VERTEX_POINT('',#32595);
#9767=VERTEX_POINT('',#32598);
#9768=VERTEX_POINT('',#32599);
#9769=VERTEX_POINT('',#32603);
#9770=VERTEX_POINT('',#32609);
#9771=VERTEX_POINT('',#32610);
#9772=VERTEX_POINT('',#32614);
#9773=VERTEX_POINT('',#32620);
#9774=VERTEX_POINT('',#32621);
#9775=VERTEX_POINT('',#32625);
#9776=VERTEX_POINT('',#32637);
#9777=VERTEX_POINT('',#32638);
#9778=VERTEX_POINT('',#32642);
#9779=VERTEX_POINT('',#32648);
#9780=VERTEX_POINT('',#32649);
#9781=VERTEX_POINT('',#32653);
#9782=VERTEX_POINT('',#32659);
#9783=VERTEX_POINT('',#32660);
#9784=VERTEX_POINT('',#32664);
#9785=VERTEX_POINT('',#32673);
#9786=VERTEX_POINT('',#32674);
#9787=VERTEX_POINT('',#32676);
#9788=VERTEX_POINT('',#32678);
#9789=VERTEX_POINT('',#32682);
#9790=VERTEX_POINT('',#32683);
#9791=VERTEX_POINT('',#32688);
#9792=VERTEX_POINT('',#32689);
#9793=VERTEX_POINT('',#32694);
#9794=VERTEX_POINT('',#32695);
#9795=VERTEX_POINT('',#32700);
#9796=VERTEX_POINT('',#32701);
#9797=VERTEX_POINT('',#32706);
#9798=VERTEX_POINT('',#32707);
#9799=VERTEX_POINT('',#32712);
#9800=VERTEX_POINT('',#32713);
#9801=VERTEX_POINT('',#32721);
#9802=VERTEX_POINT('',#32723);
#9803=VERTEX_POINT('',#32727);
#9804=VERTEX_POINT('',#32731);
#9805=VERTEX_POINT('',#32735);
#9806=VERTEX_POINT('',#32739);
#9807=VERTEX_POINT('',#32741);
#9808=VERTEX_POINT('',#32743);
#9809=VERTEX_POINT('',#32745);
#9810=VERTEX_POINT('',#32748);
#9811=VERTEX_POINT('',#32749);
#9812=VERTEX_POINT('',#32751);
#9813=VERTEX_POINT('',#32753);
#9814=VERTEX_POINT('',#32757);
#9815=VERTEX_POINT('',#32758);
#9816=VERTEX_POINT('',#32763);
#9817=VERTEX_POINT('',#32768);
#9818=VERTEX_POINT('',#32772);
#9819=VERTEX_POINT('',#32776);
#9820=VERTEX_POINT('',#32780);
#9821=VERTEX_POINT('',#32787);
#9822=VERTEX_POINT('',#32789);
#9823=VERTEX_POINT('',#32793);
#9824=VERTEX_POINT('',#32797);
#9825=VERTEX_POINT('',#32801);
#9826=VERTEX_POINT('',#32809);
#9827=VERTEX_POINT('',#32811);
#9828=VERTEX_POINT('',#32815);
#9829=VERTEX_POINT('',#32819);
#9830=VERTEX_POINT('',#32823);
#9831=VERTEX_POINT('',#32827);
#9832=VERTEX_POINT('',#32828);
#9833=VERTEX_POINT('',#32833);
#9834=VERTEX_POINT('',#32834);
#9835=VERTEX_POINT('',#32839);
#9836=VERTEX_POINT('',#32840);
#9837=VERTEX_POINT('',#32848);
#9838=VERTEX_POINT('',#32850);
#9839=VERTEX_POINT('',#32854);
#9840=VERTEX_POINT('',#32858);
#9841=VERTEX_POINT('',#32862);
#9842=VERTEX_POINT('',#32866);
#9843=VERTEX_POINT('',#32868);
#9844=VERTEX_POINT('',#32872);
#9845=VERTEX_POINT('',#32876);
#9846=VERTEX_POINT('',#32878);
#9847=VERTEX_POINT('',#32882);
#9848=VERTEX_POINT('',#32886);
#9849=VERTEX_POINT('',#32890);
#9850=VERTEX_POINT('',#32894);
#9851=VERTEX_POINT('',#32895);
#9852=VERTEX_POINT('',#32900);
#9853=VERTEX_POINT('',#32901);
#9854=VERTEX_POINT('',#32906);
#9855=VERTEX_POINT('',#32907);
#9856=VERTEX_POINT('',#32921);
#9857=VERTEX_POINT('',#32924);
#9858=VERTEX_POINT('',#32926);
#9859=VERTEX_POINT('',#32930);
#9860=VERTEX_POINT('',#32935);
#9861=VERTEX_POINT('',#32939);
#9862=VERTEX_POINT('',#32945);
#9863=VERTEX_POINT('',#32946);
#9864=VERTEX_POINT('',#32950);
#9865=VERTEX_POINT('',#32956);
#9866=VERTEX_POINT('',#32957);
#9867=VERTEX_POINT('',#32961);
#9868=VERTEX_POINT('',#32967);
#9869=VERTEX_POINT('',#32968);
#9870=VERTEX_POINT('',#32972);
#9871=VERTEX_POINT('',#32990);
#9872=VERTEX_POINT('',#32992);
#9873=VERTEX_POINT('',#32994);
#9874=VERTEX_POINT('',#32998);
#9875=VERTEX_POINT('',#33000);
#9876=VERTEX_POINT('',#33004);
#9877=VERTEX_POINT('',#33008);
#9878=VERTEX_POINT('',#33012);
#9879=VERTEX_POINT('',#33016);
#9880=VERTEX_POINT('',#33020);
#9881=VERTEX_POINT('',#33022);
#9882=VERTEX_POINT('',#33024);
#9883=VERTEX_POINT('',#33026);
#9884=VERTEX_POINT('',#33029);
#9885=VERTEX_POINT('',#33033);
#9886=VERTEX_POINT('',#33037);
#9887=VERTEX_POINT('',#33041);
#9888=VERTEX_POINT('',#33044);
#9889=VERTEX_POINT('',#33046);
#9890=VERTEX_POINT('',#33050);
#9891=VERTEX_POINT('',#33051);
#9892=VERTEX_POINT('',#33056);
#9893=VERTEX_POINT('',#33060);
#9894=VERTEX_POINT('',#33066);
#9895=VERTEX_POINT('',#33067);
#9896=VERTEX_POINT('',#33071);
#9897=VERTEX_POINT('',#33077);
#9898=VERTEX_POINT('',#33078);
#9899=VERTEX_POINT('',#33082);
#9900=VERTEX_POINT('',#33088);
#9901=VERTEX_POINT('',#33089);
#9902=VERTEX_POINT('',#33093);
#9903=VERTEX_POINT('',#33100);
#9904=VERTEX_POINT('',#33102);
#9905=VERTEX_POINT('',#33104);
#9906=VERTEX_POINT('',#33108);
#9907=VERTEX_POINT('',#33112);
#9908=VERTEX_POINT('',#33114);
#9909=VERTEX_POINT('',#33116);
#9910=VERTEX_POINT('',#33118);
#9911=VERTEX_POINT('',#33120);
#9912=VERTEX_POINT('',#33122);
#9913=VERTEX_POINT('',#33124);
#9914=VERTEX_POINT('',#33127);
#9915=VERTEX_POINT('',#33131);
#9916=VERTEX_POINT('',#33133);
#9917=VERTEX_POINT('',#33135);
#9918=VERTEX_POINT('',#33137);
#9919=VERTEX_POINT('',#33139);
#9920=VERTEX_POINT('',#33141);
#9921=VERTEX_POINT('',#33143);
#9922=VERTEX_POINT('',#33146);
#9923=VERTEX_POINT('',#33148);
#9924=VERTEX_POINT('',#33152);
#9925=VERTEX_POINT('',#33158);
#9926=VERTEX_POINT('',#33160);
#9927=VERTEX_POINT('',#33164);
#9928=VERTEX_POINT('',#33170);
#9929=VERTEX_POINT('',#33172);
#9930=VERTEX_POINT('',#33176);
#9931=VERTEX_POINT('',#33182);
#9932=VERTEX_POINT('',#33184);
#9933=VERTEX_POINT('',#33188);
#9934=VERTEX_POINT('',#33194);
#9935=VERTEX_POINT('',#33196);
#9936=VERTEX_POINT('',#33200);
#9937=VERTEX_POINT('',#33206);
#9938=VERTEX_POINT('',#33208);
#9939=VERTEX_POINT('',#33212);
#9940=VERTEX_POINT('',#33214);
#9941=VERTEX_POINT('',#33220);
#9942=VERTEX_POINT('',#33222);
#9943=VERTEX_POINT('',#33226);
#9944=VERTEX_POINT('',#33227);
#9945=VERTEX_POINT('',#33235);
#9946=VERTEX_POINT('',#33236);
#9947=VERTEX_POINT('',#33238);
#9948=VERTEX_POINT('',#33264);
#9949=VERTEX_POINT('',#33267);
#9950=VERTEX_POINT('',#33272);
#9951=VERTEX_POINT('',#33297);
#9952=VERTEX_POINT('',#33298);
#9953=VERTEX_POINT('',#33345);
#9954=VERTEX_POINT('',#33346);
#9955=VERTEX_POINT('',#33393);
#9956=VERTEX_POINT('',#33394);
#9957=VERTEX_POINT('',#33441);
#9958=VERTEX_POINT('',#33442);
#9959=VERTEX_POINT('',#33489);
#9960=VERTEX_POINT('',#33490);
#9961=VERTEX_POINT('',#33543);
#9962=VERTEX_POINT('',#33544);
#9963=VERTEX_POINT('',#33591);
#9964=VERTEX_POINT('',#33592);
#9965=VERTEX_POINT('',#33639);
#9966=VERTEX_POINT('',#33640);
#9967=VERTEX_POINT('',#33693);
#9968=VERTEX_POINT('',#33694);
#9969=VERTEX_POINT('',#33741);
#9970=VERTEX_POINT('',#33742);
#9971=VERTEX_POINT('',#33744);
#9972=VERTEX_POINT('',#33750);
#9973=VERTEX_POINT('',#33757);
#9974=VERTEX_POINT('',#33758);
#9975=VERTEX_POINT('',#33781);
#9976=VERTEX_POINT('',#33782);
#9977=VERTEX_POINT('',#33806);
#9978=VERTEX_POINT('',#33807);
#9979=VERTEX_POINT('',#33831);
#9980=VERTEX_POINT('',#33832);
#9981=VERTEX_POINT('',#33855);
#9982=VERTEX_POINT('',#33856);
#9983=VERTEX_POINT('',#33880);
#9984=VERTEX_POINT('',#33881);
#9985=VERTEX_POINT('',#33905);
#9986=VERTEX_POINT('',#33906);
#9987=VERTEX_POINT('',#33929);
#9988=VERTEX_POINT('',#33930);
#9989=VERTEX_POINT('',#33955);
#9990=VERTEX_POINT('',#33956);
#9991=VERTEX_POINT('',#33979);
#9992=VERTEX_POINT('',#33980);
#9993=VERTEX_POINT('',#34295);
#9994=VERTEX_POINT('',#34373);
#9995=VERTEX_POINT('',#34447);
#9996=VERTEX_POINT('',#34809);
#9997=VERTEX_POINT('',#34888);
#9998=VERTEX_POINT('',#34890);
#9999=VERTEX_POINT('',#34894);
#10000=VERTEX_POINT('',#34896);
#10001=VERTEX_POINT('',#34900);
#10002=VERTEX_POINT('',#34902);
#10003=VERTEX_POINT('',#34906);
#10004=VERTEX_POINT('',#34908);
#10005=VERTEX_POINT('',#34912);
#10006=VERTEX_POINT('',#34913);
#10007=VERTEX_POINT('',#34915);
#10008=VERTEX_POINT('',#34917);
#10009=VERTEX_POINT('',#34921);
#10010=VERTEX_POINT('',#34925);
#10011=VERTEX_POINT('',#34931);
#10012=VERTEX_POINT('',#34932);
#10013=VERTEX_POINT('',#34934);
#10014=VERTEX_POINT('',#34936);
#10015=VERTEX_POINT('',#34940);
#10016=VERTEX_POINT('',#34944);
#10017=VERTEX_POINT('',#34950);
#10018=VERTEX_POINT('',#34951);
#10019=VERTEX_POINT('',#34953);
#10020=VERTEX_POINT('',#34955);
#10021=VERTEX_POINT('',#34959);
#10022=VERTEX_POINT('',#34963);
#10023=VERTEX_POINT('',#34969);
#10024=VERTEX_POINT('',#34970);
#10025=VERTEX_POINT('',#34972);
#10026=VERTEX_POINT('',#34974);
#10027=VERTEX_POINT('',#34978);
#10028=VERTEX_POINT('',#34982);
#10029=VERTEX_POINT('',#34988);
#10030=VERTEX_POINT('',#34989);
#10031=VERTEX_POINT('',#34991);
#10032=VERTEX_POINT('',#34993);
#10033=VERTEX_POINT('',#34997);
#10034=VERTEX_POINT('',#35001);
#10035=VERTEX_POINT('',#35007);
#10036=VERTEX_POINT('',#35008);
#10037=VERTEX_POINT('',#35010);
#10038=VERTEX_POINT('',#35012);
#10039=VERTEX_POINT('',#35016);
#10040=VERTEX_POINT('',#35020);
#10041=VERTEX_POINT('',#35026);
#10042=VERTEX_POINT('',#35027);
#10043=VERTEX_POINT('',#35029);
#10044=VERTEX_POINT('',#35031);
#10045=VERTEX_POINT('',#35035);
#10046=VERTEX_POINT('',#35039);
#10047=VERTEX_POINT('',#35045);
#10048=VERTEX_POINT('',#35046);
#10049=VERTEX_POINT('',#35048);
#10050=VERTEX_POINT('',#35050);
#10051=VERTEX_POINT('',#35054);
#10052=VERTEX_POINT('',#35058);
#10053=VERTEX_POINT('',#35064);
#10054=VERTEX_POINT('',#35065);
#10055=VERTEX_POINT('',#35067);
#10056=VERTEX_POINT('',#35069);
#10057=VERTEX_POINT('',#35073);
#10058=VERTEX_POINT('',#35077);
#10059=VERTEX_POINT('',#35083);
#10060=VERTEX_POINT('',#35084);
#10061=VERTEX_POINT('',#35086);
#10062=VERTEX_POINT('',#35088);
#10063=VERTEX_POINT('',#35092);
#10064=VERTEX_POINT('',#35096);
#10065=VERTEX_POINT('',#35102);
#10066=VERTEX_POINT('',#35103);
#10067=VERTEX_POINT('',#35105);
#10068=VERTEX_POINT('',#35107);
#10069=VERTEX_POINT('',#35111);
#10070=VERTEX_POINT('',#35115);
#10071=VERTEX_POINT('',#35121);
#10072=VERTEX_POINT('',#35122);
#10073=VERTEX_POINT('',#35124);
#10074=VERTEX_POINT('',#35126);
#10075=VERTEX_POINT('',#35130);
#10076=VERTEX_POINT('',#35132);
#10077=VERTEX_POINT('',#35136);
#10078=VERTEX_POINT('',#35140);
#10079=VERTEX_POINT('',#35144);
#10080=VERTEX_POINT('',#35145);
#10081=VERTEX_POINT('',#35147);
#10082=VERTEX_POINT('',#35149);
#10083=VERTEX_POINT('',#35153);
#10084=VERTEX_POINT('',#35157);
#10085=VERTEX_POINT('',#35163);
#10086=VERTEX_POINT('',#35164);
#10087=VERTEX_POINT('',#35166);
#10088=VERTEX_POINT('',#35168);
#10089=VERTEX_POINT('',#35172);
#10090=VERTEX_POINT('',#35176);
#10091=VERTEX_POINT('',#35182);
#10092=VERTEX_POINT('',#35183);
#10093=VERTEX_POINT('',#35185);
#10094=VERTEX_POINT('',#35187);
#10095=VERTEX_POINT('',#35191);
#10096=VERTEX_POINT('',#35195);
#10097=VERTEX_POINT('',#35201);
#10098=VERTEX_POINT('',#35202);
#10099=VERTEX_POINT('',#35204);
#10100=VERTEX_POINT('',#35206);
#10101=VERTEX_POINT('',#35210);
#10102=VERTEX_POINT('',#35214);
#10103=VERTEX_POINT('',#35220);
#10104=VERTEX_POINT('',#35221);
#10105=VERTEX_POINT('',#35223);
#10106=VERTEX_POINT('',#35225);
#10107=VERTEX_POINT('',#35229);
#10108=VERTEX_POINT('',#35233);
#10109=VERTEX_POINT('',#35239);
#10110=VERTEX_POINT('',#35240);
#10111=VERTEX_POINT('',#35242);
#10112=VERTEX_POINT('',#35244);
#10113=VERTEX_POINT('',#35248);
#10114=VERTEX_POINT('',#35252);
#10115=VERTEX_POINT('',#35258);
#10116=VERTEX_POINT('',#35259);
#10117=VERTEX_POINT('',#35261);
#10118=VERTEX_POINT('',#35263);
#10119=VERTEX_POINT('',#35267);
#10120=VERTEX_POINT('',#35271);
#10121=VERTEX_POINT('',#35277);
#10122=VERTEX_POINT('',#35278);
#10123=VERTEX_POINT('',#35280);
#10124=VERTEX_POINT('',#35282);
#10125=VERTEX_POINT('',#35286);
#10126=VERTEX_POINT('',#35290);
#10127=VERTEX_POINT('',#35296);
#10128=VERTEX_POINT('',#35297);
#10129=VERTEX_POINT('',#35299);
#10130=VERTEX_POINT('',#35301);
#10131=VERTEX_POINT('',#35305);
#10132=VERTEX_POINT('',#35309);
#10133=VERTEX_POINT('',#35315);
#10134=VERTEX_POINT('',#35316);
#10135=VERTEX_POINT('',#35318);
#10136=VERTEX_POINT('',#35320);
#10137=VERTEX_POINT('',#35324);
#10138=VERTEX_POINT('',#35328);
#10139=VERTEX_POINT('',#35334);
#10140=VERTEX_POINT('',#35335);
#10141=VERTEX_POINT('',#35337);
#10142=VERTEX_POINT('',#35339);
#10143=VERTEX_POINT('',#35343);
#10144=VERTEX_POINT('',#35347);
#10145=VERTEX_POINT('',#35353);
#10146=VERTEX_POINT('',#35354);
#10147=VERTEX_POINT('',#35356);
#10148=VERTEX_POINT('',#35358);
#10149=VERTEX_POINT('',#35362);
#10150=VERTEX_POINT('',#35366);
#10151=VERTEX_POINT('',#35372);
#10152=VERTEX_POINT('',#35374);
#10153=VERTEX_POINT('',#35378);
#10154=VERTEX_POINT('',#35383);
#10155=VERTEX_POINT('',#35386);
#10156=VERTEX_POINT('',#35390);
#10157=VERTEX_POINT('',#35393);
#10158=VERTEX_POINT('',#35397);
#10159=VERTEX_POINT('',#35400);
#10160=VERTEX_POINT('',#35404);
#10161=VERTEX_POINT('',#35409);
#10162=VERTEX_POINT('',#35410);
#10163=VERTEX_POINT('',#35412);
#10164=VERTEX_POINT('',#35414);
#10165=VERTEX_POINT('',#35418);
#10166=VERTEX_POINT('',#35420);
#10167=VERTEX_POINT('',#35424);
#10168=VERTEX_POINT('',#35426);
#10169=VERTEX_POINT('',#35430);
#10170=VERTEX_POINT('',#35432);
#10171=VERTEX_POINT('',#35436);
#10172=VERTEX_POINT('',#35438);
#10173=VERTEX_POINT('',#35446);
#10174=VERTEX_POINT('',#35447);
#10175=VERTEX_POINT('',#35449);
#10176=VERTEX_POINT('',#35451);
#10177=VERTEX_POINT('',#35456);
#10178=VERTEX_POINT('',#35458);
#10179=VERTEX_POINT('',#35462);
#10180=VERTEX_POINT('',#35466);
#10181=VERTEX_POINT('',#35473);
#10182=VERTEX_POINT('',#35480);
#10183=VERTEX_POINT('',#35482);
#10184=VERTEX_POINT('',#35484);
#10185=VERTEX_POINT('',#35488);
#10186=VERTEX_POINT('',#35490);
#10187=VERTEX_POINT('',#35495);
#10188=VERTEX_POINT('',#35501);
#10189=VERTEX_POINT('',#35503);
#10190=VERTEX_POINT('',#35507);
#10191=VERTEX_POINT('',#35510);
#10192=VERTEX_POINT('',#35513);
#10193=VERTEX_POINT('',#35514);
#10194=VERTEX_POINT('',#35519);
#10195=VERTEX_POINT('',#35521);
#10196=VERTEX_POINT('',#35525);
#10197=VERTEX_POINT('',#35528);
#10198=VERTEX_POINT('',#35533);
#10199=VERTEX_POINT('',#35537);
#10200=VERTEX_POINT('',#35539);
#10201=VERTEX_POINT('',#35543);
#10202=VERTEX_POINT('',#35546);
#10203=VERTEX_POINT('',#35550);
#10204=VERTEX_POINT('',#35556);
#10205=VERTEX_POINT('',#35557);
#10206=VERTEX_POINT('',#35560);
#10207=VERTEX_POINT('',#35562);
#10208=VERTEX_POINT('',#35566);
#10209=VERTEX_POINT('',#35568);
#10210=VERTEX_POINT('',#35572);
#10211=VERTEX_POINT('',#35576);
#10212=VERTEX_POINT('',#35580);
#10213=VERTEX_POINT('',#35583);
#10214=VERTEX_POINT('',#35584);
#10215=VERTEX_POINT('',#35586);
#10216=VERTEX_POINT('',#35588);
#10217=VERTEX_POINT('',#35592);
#10218=VERTEX_POINT('',#35596);
#10219=VERTEX_POINT('',#35602);
#10220=VERTEX_POINT('',#35603);
#10221=VERTEX_POINT('',#35605);
#10222=VERTEX_POINT('',#35607);
#10223=VERTEX_POINT('',#35611);
#10224=VERTEX_POINT('',#35615);
#10225=VERTEX_POINT('',#35621);
#10226=VERTEX_POINT('',#35622);
#10227=VERTEX_POINT('',#35624);
#10228=VERTEX_POINT('',#35626);
#10229=VERTEX_POINT('',#35630);
#10230=VERTEX_POINT('',#35634);
#10231=VERTEX_POINT('',#35640);
#10232=VERTEX_POINT('',#35641);
#10233=VERTEX_POINT('',#35643);
#10234=VERTEX_POINT('',#35645);
#10235=VERTEX_POINT('',#35649);
#10236=VERTEX_POINT('',#35653);
#10237=VERTEX_POINT('',#35659);
#10238=VERTEX_POINT('',#35660);
#10239=VERTEX_POINT('',#35662);
#10240=VERTEX_POINT('',#35664);
#10241=VERTEX_POINT('',#35668);
#10242=VERTEX_POINT('',#35672);
#10243=VERTEX_POINT('',#35678);
#10244=VERTEX_POINT('',#35679);
#10245=VERTEX_POINT('',#35681);
#10246=VERTEX_POINT('',#35683);
#10247=VERTEX_POINT('',#35687);
#10248=VERTEX_POINT('',#35691);
#10249=VERTEX_POINT('',#35697);
#10250=VERTEX_POINT('',#35698);
#10251=VERTEX_POINT('',#35700);
#10252=VERTEX_POINT('',#35702);
#10253=VERTEX_POINT('',#35706);
#10254=VERTEX_POINT('',#35710);
#10255=VERTEX_POINT('',#35716);
#10256=VERTEX_POINT('',#35717);
#10257=VERTEX_POINT('',#35719);
#10258=VERTEX_POINT('',#35721);
#10259=VERTEX_POINT('',#35725);
#10260=VERTEX_POINT('',#35729);
#10261=VERTEX_POINT('',#35735);
#10262=VERTEX_POINT('',#35736);
#10263=VERTEX_POINT('',#35738);
#10264=VERTEX_POINT('',#35740);
#10265=VERTEX_POINT('',#35744);
#10266=VERTEX_POINT('',#35746);
#10267=VERTEX_POINT('',#35750);
#10268=VERTEX_POINT('',#35754);
#10269=VERTEX_POINT('',#35758);
#10270=VERTEX_POINT('',#35759);
#10271=VERTEX_POINT('',#35761);
#10272=VERTEX_POINT('',#35763);
#10273=VERTEX_POINT('',#35767);
#10274=VERTEX_POINT('',#35771);
#10275=VERTEX_POINT('',#35777);
#10276=VERTEX_POINT('',#35778);
#10277=VERTEX_POINT('',#35780);
#10278=VERTEX_POINT('',#35782);
#10279=VERTEX_POINT('',#35786);
#10280=VERTEX_POINT('',#35790);
#10281=VERTEX_POINT('',#35796);
#10282=VERTEX_POINT('',#35797);
#10283=VERTEX_POINT('',#35799);
#10284=VERTEX_POINT('',#35801);
#10285=VERTEX_POINT('',#35805);
#10286=VERTEX_POINT('',#35809);
#10287=VERTEX_POINT('',#35815);
#10288=VERTEX_POINT('',#35816);
#10289=VERTEX_POINT('',#35818);
#10290=VERTEX_POINT('',#35820);
#10291=VERTEX_POINT('',#35824);
#10292=VERTEX_POINT('',#35828);
#10293=VERTEX_POINT('',#35834);
#10294=VERTEX_POINT('',#35835);
#10295=VERTEX_POINT('',#35837);
#10296=VERTEX_POINT('',#35839);
#10297=VERTEX_POINT('',#35843);
#10298=VERTEX_POINT('',#35847);
#10299=VERTEX_POINT('',#35853);
#10300=VERTEX_POINT('',#35854);
#10301=VERTEX_POINT('',#35856);
#10302=VERTEX_POINT('',#35858);
#10303=VERTEX_POINT('',#35862);
#10304=VERTEX_POINT('',#35866);
#10305=VERTEX_POINT('',#35872);
#10306=VERTEX_POINT('',#35873);
#10307=VERTEX_POINT('',#35875);
#10308=VERTEX_POINT('',#35877);
#10309=VERTEX_POINT('',#35881);
#10310=VERTEX_POINT('',#35885);
#10311=VERTEX_POINT('',#35891);
#10312=VERTEX_POINT('',#35892);
#10313=VERTEX_POINT('',#35894);
#10314=VERTEX_POINT('',#35896);
#10315=VERTEX_POINT('',#35900);
#10316=VERTEX_POINT('',#35904);
#10317=VERTEX_POINT('',#35910);
#10318=VERTEX_POINT('',#35911);
#10319=VERTEX_POINT('',#35913);
#10320=VERTEX_POINT('',#35915);
#10321=VERTEX_POINT('',#35919);
#10322=VERTEX_POINT('',#35923);
#10323=VERTEX_POINT('',#35929);
#10324=VERTEX_POINT('',#35931);
#10325=VERTEX_POINT('',#35935);
#10326=VERTEX_POINT('',#35937);
#10327=VERTEX_POINT('',#35942);
#10328=VERTEX_POINT('',#35946);
#10329=VERTEX_POINT('',#35952);
#10330=VERTEX_POINT('',#35955);
#10331=VERTEX_POINT('',#35960);
#10332=VERTEX_POINT('',#35963);
#10333=VERTEX_POINT('',#35969);
#10334=VERTEX_POINT('',#35971);
#10335=VERTEX_POINT('',#35975);
#10336=VERTEX_POINT('',#35978);
#10337=VERTEX_POINT('',#35984);
#10338=VERTEX_POINT('',#35986);
#10339=VERTEX_POINT('',#35990);
#10340=VERTEX_POINT('',#35992);
#10341=VERTEX_POINT('',#35996);
#10342=VERTEX_POINT('',#35997);
#10343=VERTEX_POINT('',#35999);
#10344=VERTEX_POINT('',#36001);
#10345=VERTEX_POINT('',#36003);
#10346=VERTEX_POINT('',#36005);
#10347=VERTEX_POINT('',#36009);
#10348=VERTEX_POINT('',#36013);
#10349=VERTEX_POINT('',#36014);
#10350=VERTEX_POINT('',#36016);
#10351=VERTEX_POINT('',#36018);
#10352=VERTEX_POINT('',#36020);
#10353=VERTEX_POINT('',#36022);
#10354=VERTEX_POINT('',#36024);
#10355=VERTEX_POINT('',#36026);
#10356=VERTEX_POINT('',#36030);
#10357=VERTEX_POINT('',#36032);
#10358=VERTEX_POINT('',#36036);
#10359=VERTEX_POINT('',#36040);
#10360=VERTEX_POINT('',#36044);
#10361=VERTEX_POINT('',#36048);
#10362=VERTEX_POINT('',#36052);
#10363=VERTEX_POINT('',#36053);
#10364=VERTEX_POINT('',#36055);
#10365=VERTEX_POINT('',#36057);
#10366=VERTEX_POINT('',#36061);
#10367=VERTEX_POINT('',#36063);
#10368=VERTEX_POINT('',#36067);
#10369=VERTEX_POINT('',#36068);
#10370=VERTEX_POINT('',#36073);
#10371=VERTEX_POINT('',#36074);
#10372=VERTEX_POINT('',#36079);
#10373=VERTEX_POINT('',#36080);
#10374=VERTEX_POINT('',#36088);
#10375=VERTEX_POINT('',#36090);
#10376=VERTEX_POINT('',#36094);
#10377=VERTEX_POINT('',#36102);
#10378=VERTEX_POINT('',#36104);
#10379=VERTEX_POINT('',#36108);
#10380=VERTEX_POINT('',#36112);
#10381=VERTEX_POINT('',#36116);
#10382=VERTEX_POINT('',#36141);
#10383=VERTEX_POINT('',#36143);
#10384=VERTEX_POINT('',#36147);
#10385=VERTEX_POINT('',#36151);
#10386=VERTEX_POINT('',#36158);
#10387=VERTEX_POINT('',#36159);
#10388=VERTEX_POINT('',#36161);
#10389=VERTEX_POINT('',#36175);
#10390=VERTEX_POINT('',#36177);
#10391=VERTEX_POINT('',#36180);
#10392=VERTEX_POINT('',#36193);
#10393=VERTEX_POINT('',#36194);
#10394=VERTEX_POINT('',#36241);
#10395=VERTEX_POINT('',#36242);
#10396=VERTEX_POINT('',#36295);
#10397=VERTEX_POINT('',#36296);
#10398=VERTEX_POINT('',#36343);
#10399=VERTEX_POINT('',#36344);
#10400=VERTEX_POINT('',#36391);
#10401=VERTEX_POINT('',#36392);
#10402=VERTEX_POINT('',#36439);
#10403=VERTEX_POINT('',#36440);
#10404=VERTEX_POINT('',#36493);
#10405=VERTEX_POINT('',#36494);
#10406=VERTEX_POINT('',#36541);
#10407=VERTEX_POINT('',#36542);
#10408=VERTEX_POINT('',#36589);
#10409=VERTEX_POINT('',#36590);
#10410=VERTEX_POINT('',#36643);
#10411=VERTEX_POINT('',#36644);
#10412=VERTEX_POINT('',#36691);
#10413=VERTEX_POINT('',#36692);
#10414=VERTEX_POINT('',#36739);
#10415=VERTEX_POINT('',#36740);
#10416=VERTEX_POINT('',#36793);
#10417=VERTEX_POINT('',#36794);
#10418=VERTEX_POINT('',#36841);
#10419=VERTEX_POINT('',#36842);
#10420=VERTEX_POINT('',#36844);
#10421=VERTEX_POINT('',#36851);
#10422=VERTEX_POINT('',#36859);
#10423=VERTEX_POINT('',#36860);
#10424=VERTEX_POINT('',#36883);
#10425=VERTEX_POINT('',#36884);
#10426=VERTEX_POINT('',#36908);
#10427=VERTEX_POINT('',#36909);
#10428=VERTEX_POINT('',#36933);
#10429=VERTEX_POINT('',#36934);
#10430=VERTEX_POINT('',#36957);
#10431=VERTEX_POINT('',#36958);
#10432=VERTEX_POINT('',#36982);
#10433=VERTEX_POINT('',#36983);
#10434=VERTEX_POINT('',#37007);
#10435=VERTEX_POINT('',#37008);
#10436=VERTEX_POINT('',#37031);
#10437=VERTEX_POINT('',#37032);
#10438=VERTEX_POINT('',#37056);
#10439=VERTEX_POINT('',#37057);
#10440=VERTEX_POINT('',#37081);
#10441=VERTEX_POINT('',#37082);
#10442=VERTEX_POINT('',#37105);
#10443=VERTEX_POINT('',#37106);
#10444=VERTEX_POINT('',#37129);
#10445=VERTEX_POINT('',#37130);
#10446=VERTEX_POINT('',#37154);
#10447=VERTEX_POINT('',#37155);
#10448=VERTEX_POINT('',#37179);
#10449=VERTEX_POINT('',#37180);
#10450=VERTEX_POINT('',#37182);
#10451=VERTEX_POINT('',#37583);
#10452=VERTEX_POINT('',#37655);
#10453=VERTEX_POINT('',#38147);
#10454=VERTEX_POINT('',#38219);
#10455=VERTEX_POINT('',#38220);
#10456=VERTEX_POINT('',#38224);
#10457=VERTEX_POINT('',#38225);
#10458=VERTEX_POINT('',#38227);
#10459=VERTEX_POINT('',#38229);
#10460=VERTEX_POINT('',#38233);
#10461=VERTEX_POINT('',#38237);
#10462=VERTEX_POINT('',#38243);
#10463=VERTEX_POINT('',#38244);
#10464=VERTEX_POINT('',#38246);
#10465=VERTEX_POINT('',#38248);
#10466=VERTEX_POINT('',#38252);
#10467=VERTEX_POINT('',#38256);
#10468=VERTEX_POINT('',#38262);
#10469=VERTEX_POINT('',#38263);
#10470=VERTEX_POINT('',#38265);
#10471=VERTEX_POINT('',#38267);
#10472=VERTEX_POINT('',#38271);
#10473=VERTEX_POINT('',#38275);
#10474=VERTEX_POINT('',#38281);
#10475=VERTEX_POINT('',#38282);
#10476=VERTEX_POINT('',#38284);
#10477=VERTEX_POINT('',#38286);
#10478=VERTEX_POINT('',#38290);
#10479=VERTEX_POINT('',#38294);
#10480=VERTEX_POINT('',#38300);
#10481=VERTEX_POINT('',#38301);
#10482=VERTEX_POINT('',#38303);
#10483=VERTEX_POINT('',#38305);
#10484=VERTEX_POINT('',#38309);
#10485=VERTEX_POINT('',#38313);
#10486=VERTEX_POINT('',#38319);
#10487=VERTEX_POINT('',#38320);
#10488=VERTEX_POINT('',#38322);
#10489=VERTEX_POINT('',#38324);
#10490=VERTEX_POINT('',#38328);
#10491=VERTEX_POINT('',#38332);
#10492=VERTEX_POINT('',#38338);
#10493=VERTEX_POINT('',#38339);
#10494=VERTEX_POINT('',#38341);
#10495=VERTEX_POINT('',#38343);
#10496=VERTEX_POINT('',#38347);
#10497=VERTEX_POINT('',#38351);
#10498=VERTEX_POINT('',#38357);
#10499=VERTEX_POINT('',#38358);
#10500=VERTEX_POINT('',#38360);
#10501=VERTEX_POINT('',#38362);
#10502=VERTEX_POINT('',#38366);
#10503=VERTEX_POINT('',#38370);
#10504=VERTEX_POINT('',#38376);
#10505=VERTEX_POINT('',#38377);
#10506=VERTEX_POINT('',#38379);
#10507=VERTEX_POINT('',#38381);
#10508=VERTEX_POINT('',#38385);
#10509=VERTEX_POINT('',#38389);
#10510=VERTEX_POINT('',#38395);
#10511=VERTEX_POINT('',#38396);
#10512=VERTEX_POINT('',#38398);
#10513=VERTEX_POINT('',#38400);
#10514=VERTEX_POINT('',#38404);
#10515=VERTEX_POINT('',#38408);
#10516=VERTEX_POINT('',#38414);
#10517=VERTEX_POINT('',#38415);
#10518=VERTEX_POINT('',#38417);
#10519=VERTEX_POINT('',#38419);
#10520=VERTEX_POINT('',#38423);
#10521=VERTEX_POINT('',#38427);
#10522=VERTEX_POINT('',#38433);
#10523=VERTEX_POINT('',#38434);
#10524=VERTEX_POINT('',#38436);
#10525=VERTEX_POINT('',#38438);
#10526=VERTEX_POINT('',#38442);
#10527=VERTEX_POINT('',#38444);
#10528=VERTEX_POINT('',#38448);
#10529=VERTEX_POINT('',#38452);
#10530=VERTEX_POINT('',#38456);
#10531=VERTEX_POINT('',#38457);
#10532=VERTEX_POINT('',#38459);
#10533=VERTEX_POINT('',#38461);
#10534=VERTEX_POINT('',#38465);
#10535=VERTEX_POINT('',#38469);
#10536=VERTEX_POINT('',#38475);
#10537=VERTEX_POINT('',#38476);
#10538=VERTEX_POINT('',#38478);
#10539=VERTEX_POINT('',#38480);
#10540=VERTEX_POINT('',#38484);
#10541=VERTEX_POINT('',#38488);
#10542=VERTEX_POINT('',#38494);
#10543=VERTEX_POINT('',#38495);
#10544=VERTEX_POINT('',#38497);
#10545=VERTEX_POINT('',#38499);
#10546=VERTEX_POINT('',#38503);
#10547=VERTEX_POINT('',#38507);
#10548=VERTEX_POINT('',#38513);
#10549=VERTEX_POINT('',#38514);
#10550=VERTEX_POINT('',#38516);
#10551=VERTEX_POINT('',#38518);
#10552=VERTEX_POINT('',#38522);
#10553=VERTEX_POINT('',#38526);
#10554=VERTEX_POINT('',#38532);
#10555=VERTEX_POINT('',#38533);
#10556=VERTEX_POINT('',#38535);
#10557=VERTEX_POINT('',#38537);
#10558=VERTEX_POINT('',#38541);
#10559=VERTEX_POINT('',#38545);
#10560=VERTEX_POINT('',#38551);
#10561=VERTEX_POINT('',#38552);
#10562=VERTEX_POINT('',#38554);
#10563=VERTEX_POINT('',#38556);
#10564=VERTEX_POINT('',#38560);
#10565=VERTEX_POINT('',#38564);
#10566=VERTEX_POINT('',#38570);
#10567=VERTEX_POINT('',#38571);
#10568=VERTEX_POINT('',#38573);
#10569=VERTEX_POINT('',#38575);
#10570=VERTEX_POINT('',#38579);
#10571=VERTEX_POINT('',#38583);
#10572=VERTEX_POINT('',#38589);
#10573=VERTEX_POINT('',#38590);
#10574=VERTEX_POINT('',#38592);
#10575=VERTEX_POINT('',#38594);
#10576=VERTEX_POINT('',#38598);
#10577=VERTEX_POINT('',#38602);
#10578=VERTEX_POINT('',#38608);
#10579=VERTEX_POINT('',#38609);
#10580=VERTEX_POINT('',#38611);
#10581=VERTEX_POINT('',#38613);
#10582=VERTEX_POINT('',#38617);
#10583=VERTEX_POINT('',#38621);
#10584=VERTEX_POINT('',#38627);
#10585=VERTEX_POINT('',#38628);
#10586=VERTEX_POINT('',#38630);
#10587=VERTEX_POINT('',#38632);
#10588=VERTEX_POINT('',#38636);
#10589=VERTEX_POINT('',#38640);
#10590=VERTEX_POINT('',#38646);
#10591=VERTEX_POINT('',#38647);
#10592=VERTEX_POINT('',#38649);
#10593=VERTEX_POINT('',#38651);
#10594=VERTEX_POINT('',#38655);
#10595=VERTEX_POINT('',#38659);
#10596=VERTEX_POINT('',#38665);
#10597=VERTEX_POINT('',#38666);
#10598=VERTEX_POINT('',#38668);
#10599=VERTEX_POINT('',#38670);
#10600=VERTEX_POINT('',#38674);
#10601=VERTEX_POINT('',#38678);
#10602=VERTEX_POINT('',#38684);
#10603=VERTEX_POINT('',#38689);
#10604=VERTEX_POINT('',#38692);
#10605=VERTEX_POINT('',#38696);
#10606=VERTEX_POINT('',#38701);
#10607=VERTEX_POINT('',#38707);
#10608=VERTEX_POINT('',#38708);
#10609=VERTEX_POINT('',#38710);
#10610=VERTEX_POINT('',#38727);
#10611=VERTEX_POINT('',#38729);
#10612=VERTEX_POINT('',#38732);
#10613=VERTEX_POINT('',#38748);
#10614=VERTEX_POINT('',#38749);
#10615=VERTEX_POINT('',#38802);
#10616=VERTEX_POINT('',#38803);
#10617=VERTEX_POINT('',#38850);
#10618=VERTEX_POINT('',#38851);
#10619=VERTEX_POINT('',#38898);
#10620=VERTEX_POINT('',#38899);
#10621=VERTEX_POINT('',#38952);
#10622=VERTEX_POINT('',#38953);
#10623=VERTEX_POINT('',#39000);
#10624=VERTEX_POINT('',#39001);
#10625=VERTEX_POINT('',#39048);
#10626=VERTEX_POINT('',#39049);
#10627=VERTEX_POINT('',#39102);
#10628=VERTEX_POINT('',#39103);
#10629=VERTEX_POINT('',#39150);
#10630=VERTEX_POINT('',#39151);
#10631=VERTEX_POINT('',#39198);
#10632=VERTEX_POINT('',#39199);
#10633=VERTEX_POINT('',#39252);
#10634=VERTEX_POINT('',#39253);
#10635=VERTEX_POINT('',#39300);
#10636=VERTEX_POINT('',#39301);
#10637=VERTEX_POINT('',#39348);
#10638=VERTEX_POINT('',#39349);
#10639=VERTEX_POINT('',#39402);
#10640=VERTEX_POINT('',#39403);
#10641=VERTEX_POINT('',#39405);
#10642=VERTEX_POINT('',#39412);
#10643=VERTEX_POINT('',#39420);
#10644=VERTEX_POINT('',#39421);
#10645=VERTEX_POINT('',#39445);
#10646=VERTEX_POINT('',#39446);
#10647=VERTEX_POINT('',#39470);
#10648=VERTEX_POINT('',#39471);
#10649=VERTEX_POINT('',#39494);
#10650=VERTEX_POINT('',#39495);
#10651=VERTEX_POINT('',#39519);
#10652=VERTEX_POINT('',#39520);
#10653=VERTEX_POINT('',#39544);
#10654=VERTEX_POINT('',#39545);
#10655=VERTEX_POINT('',#39568);
#10656=VERTEX_POINT('',#39569);
#10657=VERTEX_POINT('',#39593);
#10658=VERTEX_POINT('',#39594);
#10659=VERTEX_POINT('',#39618);
#10660=VERTEX_POINT('',#39619);
#10661=VERTEX_POINT('',#39642);
#10662=VERTEX_POINT('',#39643);
#10663=VERTEX_POINT('',#39667);
#10664=VERTEX_POINT('',#39668);
#10665=VERTEX_POINT('',#39692);
#10666=VERTEX_POINT('',#39693);
#10667=VERTEX_POINT('',#39716);
#10668=VERTEX_POINT('',#39717);
#10669=VERTEX_POINT('',#39741);
#10670=VERTEX_POINT('',#39742);
#10671=VERTEX_POINT('',#39766);
#10672=VERTEX_POINT('',#39819);
#10673=VERTEX_POINT('',#39821);
#10674=VERTEX_POINT('',#40282);
#10675=VERTEX_POINT('',#40341);
#10676=VERTEX_POINT('',#40805);
#10677=VERTEX_POINT('',#40806);
#10678=VERTEX_POINT('',#40808);
#10679=VERTEX_POINT('',#40812);
#10680=VERTEX_POINT('',#40814);
#10681=VERTEX_POINT('',#40820);
#10682=VERTEX_POINT('',#40826);
#10683=VERTEX_POINT('',#40827);
#10684=VERTEX_POINT('',#40829);
#10685=VERTEX_POINT('',#40833);
#10686=VERTEX_POINT('',#40835);
#10687=VERTEX_POINT('',#40841);
#10688=VERTEX_POINT('',#40847);
#10689=VERTEX_POINT('',#40848);
#10690=VERTEX_POINT('',#40850);
#10691=VERTEX_POINT('',#40854);
#10692=VERTEX_POINT('',#40856);
#10693=VERTEX_POINT('',#40862);
#10694=VERTEX_POINT('',#40868);
#10695=VERTEX_POINT('',#40869);
#10696=VERTEX_POINT('',#40871);
#10697=VERTEX_POINT('',#40875);
#10698=VERTEX_POINT('',#40877);
#10699=VERTEX_POINT('',#40883);
#10700=VERTEX_POINT('',#40889);
#10701=VERTEX_POINT('',#40890);
#10702=VERTEX_POINT('',#40892);
#10703=VERTEX_POINT('',#40896);
#10704=VERTEX_POINT('',#40898);
#10705=VERTEX_POINT('',#40904);
#10706=VERTEX_POINT('',#40910);
#10707=VERTEX_POINT('',#40911);
#10708=VERTEX_POINT('',#40913);
#10709=VERTEX_POINT('',#40917);
#10710=VERTEX_POINT('',#40919);
#10711=VERTEX_POINT('',#40925);
#10712=VERTEX_POINT('',#40931);
#10713=VERTEX_POINT('',#40932);
#10714=VERTEX_POINT('',#40934);
#10715=VERTEX_POINT('',#40938);
#10716=VERTEX_POINT('',#40940);
#10717=VERTEX_POINT('',#40946);
#10718=VERTEX_POINT('',#40952);
#10719=VERTEX_POINT('',#40953);
#10720=VERTEX_POINT('',#40955);
#10721=VERTEX_POINT('',#40959);
#10722=VERTEX_POINT('',#40961);
#10723=VERTEX_POINT('',#40967);
#10724=VERTEX_POINT('',#40973);
#10725=VERTEX_POINT('',#40974);
#10726=VERTEX_POINT('',#40976);
#10727=VERTEX_POINT('',#40980);
#10728=VERTEX_POINT('',#40982);
#10729=VERTEX_POINT('',#40988);
#10730=VERTEX_POINT('',#40994);
#10731=VERTEX_POINT('',#40995);
#10732=VERTEX_POINT('',#40997);
#10733=VERTEX_POINT('',#41001);
#10734=VERTEX_POINT('',#41003);
#10735=VERTEX_POINT('',#41009);
#10736=VERTEX_POINT('',#41015);
#10737=VERTEX_POINT('',#41016);
#10738=VERTEX_POINT('',#41018);
#10739=VERTEX_POINT('',#41022);
#10740=VERTEX_POINT('',#41024);
#10741=VERTEX_POINT('',#41030);
#10742=VERTEX_POINT('',#41036);
#10743=VERTEX_POINT('',#41037);
#10744=VERTEX_POINT('',#41039);
#10745=VERTEX_POINT('',#41043);
#10746=VERTEX_POINT('',#41045);
#10747=VERTEX_POINT('',#41051);
#10748=VERTEX_POINT('',#41057);
#10749=VERTEX_POINT('',#41058);
#10750=VERTEX_POINT('',#41060);
#10751=VERTEX_POINT('',#41064);
#10752=VERTEX_POINT('',#41066);
#10753=VERTEX_POINT('',#41072);
#10754=VERTEX_POINT('',#41078);
#10755=VERTEX_POINT('',#41079);
#10756=VERTEX_POINT('',#41081);
#10757=VERTEX_POINT('',#41085);
#10758=VERTEX_POINT('',#41087);
#10759=VERTEX_POINT('',#41093);
#10760=VERTEX_POINT('',#41099);
#10761=VERTEX_POINT('',#41100);
#10762=VERTEX_POINT('',#41102);
#10763=VERTEX_POINT('',#41106);
#10764=VERTEX_POINT('',#41108);
#10765=VERTEX_POINT('',#41114);
#10766=VERTEX_POINT('',#41120);
#10767=VERTEX_POINT('',#41121);
#10768=VERTEX_POINT('',#41123);
#10769=VERTEX_POINT('',#41127);
#10770=VERTEX_POINT('',#41129);
#10771=VERTEX_POINT('',#41135);
#10772=VERTEX_POINT('',#41141);
#10773=VERTEX_POINT('',#41142);
#10774=VERTEX_POINT('',#41144);
#10775=VERTEX_POINT('',#41148);
#10776=VERTEX_POINT('',#41150);
#10777=VERTEX_POINT('',#41156);
#10778=VERTEX_POINT('',#41162);
#10779=VERTEX_POINT('',#41163);
#10780=VERTEX_POINT('',#41165);
#10781=VERTEX_POINT('',#41167);
#10782=VERTEX_POINT('',#41171);
#10783=VERTEX_POINT('',#41173);
#10784=VERTEX_POINT('',#41179);
#10785=VERTEX_POINT('',#41185);
#10786=VERTEX_POINT('',#41186);
#10787=VERTEX_POINT('',#41188);
#10788=VERTEX_POINT('',#41192);
#10789=VERTEX_POINT('',#41194);
#10790=VERTEX_POINT('',#41200);
#10791=VERTEX_POINT('',#41206);
#10792=VERTEX_POINT('',#41207);
#10793=VERTEX_POINT('',#41209);
#10794=VERTEX_POINT('',#41213);
#10795=VERTEX_POINT('',#41215);
#10796=VERTEX_POINT('',#41221);
#10797=VERTEX_POINT('',#41227);
#10798=VERTEX_POINT('',#41228);
#10799=VERTEX_POINT('',#41230);
#10800=VERTEX_POINT('',#41234);
#10801=VERTEX_POINT('',#41236);
#10802=VERTEX_POINT('',#41242);
#10803=VERTEX_POINT('',#41248);
#10804=VERTEX_POINT('',#41249);
#10805=VERTEX_POINT('',#41251);
#10806=VERTEX_POINT('',#41255);
#10807=VERTEX_POINT('',#41257);
#10808=VERTEX_POINT('',#41263);
#10809=VERTEX_POINT('',#41269);
#10810=VERTEX_POINT('',#41270);
#10811=VERTEX_POINT('',#41272);
#10812=VERTEX_POINT('',#41276);
#10813=VERTEX_POINT('',#41278);
#10814=VERTEX_POINT('',#41284);
#10815=VERTEX_POINT('',#41290);
#10816=VERTEX_POINT('',#41291);
#10817=VERTEX_POINT('',#41293);
#10818=VERTEX_POINT('',#41297);
#10819=VERTEX_POINT('',#41299);
#10820=VERTEX_POINT('',#41305);
#10821=VERTEX_POINT('',#41311);
#10822=VERTEX_POINT('',#41312);
#10823=VERTEX_POINT('',#41314);
#10824=VERTEX_POINT('',#41318);
#10825=VERTEX_POINT('',#41320);
#10826=VERTEX_POINT('',#41326);
#10827=VERTEX_POINT('',#41332);
#10828=VERTEX_POINT('',#41333);
#10829=VERTEX_POINT('',#41335);
#10830=VERTEX_POINT('',#41339);
#10831=VERTEX_POINT('',#41341);
#10832=VERTEX_POINT('',#41347);
#10833=VERTEX_POINT('',#41353);
#10834=VERTEX_POINT('',#41354);
#10835=VERTEX_POINT('',#41356);
#10836=VERTEX_POINT('',#41360);
#10837=VERTEX_POINT('',#41362);
#10838=VERTEX_POINT('',#41368);
#10839=VERTEX_POINT('',#41374);
#10840=VERTEX_POINT('',#41375);
#10841=VERTEX_POINT('',#41377);
#10842=VERTEX_POINT('',#41381);
#10843=VERTEX_POINT('',#41383);
#10844=VERTEX_POINT('',#41389);
#10845=VERTEX_POINT('',#41395);
#10846=VERTEX_POINT('',#41396);
#10847=VERTEX_POINT('',#41398);
#10848=VERTEX_POINT('',#41402);
#10849=VERTEX_POINT('',#41404);
#10850=VERTEX_POINT('',#41410);
#10851=VERTEX_POINT('',#41416);
#10852=VERTEX_POINT('',#41417);
#10853=VERTEX_POINT('',#41419);
#10854=VERTEX_POINT('',#41423);
#10855=VERTEX_POINT('',#41425);
#10856=VERTEX_POINT('',#41431);
#10857=VERTEX_POINT('',#41437);
#10858=VERTEX_POINT('',#41438);
#10859=VERTEX_POINT('',#41440);
#10860=VERTEX_POINT('',#41444);
#10861=VERTEX_POINT('',#41446);
#10862=VERTEX_POINT('',#41452);
#10863=VERTEX_POINT('',#41458);
#10864=VERTEX_POINT('',#41459);
#10865=VERTEX_POINT('',#41461);
#10866=VERTEX_POINT('',#41465);
#10867=VERTEX_POINT('',#41467);
#10868=VERTEX_POINT('',#41473);
#10869=VERTEX_POINT('',#41479);
#10870=VERTEX_POINT('',#41480);
#10871=VERTEX_POINT('',#41482);
#10872=VERTEX_POINT('',#41486);
#10873=VERTEX_POINT('',#41488);
#10874=VERTEX_POINT('',#41494);
#10875=VERTEX_POINT('',#41500);
#10876=VERTEX_POINT('',#41501);
#10877=VERTEX_POINT('',#41503);
#10878=VERTEX_POINT('',#41507);
#10879=VERTEX_POINT('',#41509);
#10880=VERTEX_POINT('',#41515);
#10881=VERTEX_POINT('',#41521);
#10882=VERTEX_POINT('',#41522);
#10883=VERTEX_POINT('',#41524);
#10884=VERTEX_POINT('',#41528);
#10885=VERTEX_POINT('',#41530);
#10886=VERTEX_POINT('',#41536);
#10887=VERTEX_POINT('',#41559);
#10888=VERTEX_POINT('',#41579);
#10889=VERTEX_POINT('',#41581);
#10890=VERTEX_POINT('',#41583);
#10891=VERTEX_POINT('',#41585);
#10892=VERTEX_POINT('',#41589);
#10893=VERTEX_POINT('',#41591);
#10894=VERTEX_POINT('',#41603);
#10895=VERTEX_POINT('',#41607);
#10896=VERTEX_POINT('',#41608);
#10897=VERTEX_POINT('',#41612);
#10898=VERTEX_POINT('',#41613);
#10899=VERTEX_POINT('',#41615);
#10900=VERTEX_POINT('',#41617);
#10901=VERTEX_POINT('',#41621);
#10902=VERTEX_POINT('',#41623);
#10903=VERTEX_POINT('',#41627);
#10904=VERTEX_POINT('',#41629);
#10905=VERTEX_POINT('',#41633);
#10906=VERTEX_POINT('',#41635);
#10907=VERTEX_POINT('',#41639);
#10908=VERTEX_POINT('',#41641);
#10909=VERTEX_POINT('',#41649);
#10910=VERTEX_POINT('',#41656);
#10911=VERTEX_POINT('',#41663);
#10912=VERTEX_POINT('',#41664);
#10913=VERTEX_POINT('',#41666);
#10914=VERTEX_POINT('',#41683);
#10915=VERTEX_POINT('',#41685);
#10916=VERTEX_POINT('',#41688);
#10917=VERTEX_POINT('',#41704);
#10918=VERTEX_POINT('',#41705);
#10919=VERTEX_POINT('',#41752);
#10920=VERTEX_POINT('',#41753);
#10921=VERTEX_POINT('',#41806);
#10922=VERTEX_POINT('',#41807);
#10923=VERTEX_POINT('',#41854);
#10924=VERTEX_POINT('',#41855);
#10925=VERTEX_POINT('',#41902);
#10926=VERTEX_POINT('',#41903);
#10927=VERTEX_POINT('',#41956);
#10928=VERTEX_POINT('',#41957);
#10929=VERTEX_POINT('',#42004);
#10930=VERTEX_POINT('',#42005);
#10931=VERTEX_POINT('',#42052);
#10932=VERTEX_POINT('',#42053);
#10933=VERTEX_POINT('',#42100);
#10934=VERTEX_POINT('',#42101);
#10935=VERTEX_POINT('',#42154);
#10936=VERTEX_POINT('',#42155);
#10937=VERTEX_POINT('',#42202);
#10938=VERTEX_POINT('',#42203);
#10939=VERTEX_POINT('',#42250);
#10940=VERTEX_POINT('',#42251);
#10941=VERTEX_POINT('',#42304);
#10942=VERTEX_POINT('',#42305);
#10943=VERTEX_POINT('',#42352);
#10944=VERTEX_POINT('',#42353);
#10945=VERTEX_POINT('',#42400);
#10946=VERTEX_POINT('',#42401);
#10947=VERTEX_POINT('',#42451);
#10948=VERTEX_POINT('',#42452);
#10949=VERTEX_POINT('',#42502);
#10950=VERTEX_POINT('',#42503);
#10951=VERTEX_POINT('',#42550);
#10952=VERTEX_POINT('',#42551);
#10953=VERTEX_POINT('',#42598);
#10954=VERTEX_POINT('',#42599);
#10955=VERTEX_POINT('',#42652);
#10956=VERTEX_POINT('',#42653);
#10957=VERTEX_POINT('',#42700);
#10958=VERTEX_POINT('',#42701);
#10959=VERTEX_POINT('',#42748);
#10960=VERTEX_POINT('',#42749);
#10961=VERTEX_POINT('',#42802);
#10962=VERTEX_POINT('',#42803);
#10963=VERTEX_POINT('',#42850);
#10964=VERTEX_POINT('',#42851);
#10965=VERTEX_POINT('',#42898);
#10966=VERTEX_POINT('',#42899);
#10967=VERTEX_POINT('',#42946);
#10968=VERTEX_POINT('',#42947);
#10969=VERTEX_POINT('',#43000);
#10970=VERTEX_POINT('',#43001);
#10971=VERTEX_POINT('',#43048);
#10972=VERTEX_POINT('',#43049);
#10973=VERTEX_POINT('',#43096);
#10974=VERTEX_POINT('',#43097);
#10975=VERTEX_POINT('',#43150);
#10976=VERTEX_POINT('',#43151);
#10977=VERTEX_POINT('',#43198);
#10978=VERTEX_POINT('',#43199);
#10979=VERTEX_POINT('',#43246);
#10980=VERTEX_POINT('',#43247);
#10981=VERTEX_POINT('',#43294);
#10982=VERTEX_POINT('',#43295);
#10983=VERTEX_POINT('',#43348);
#10984=VERTEX_POINT('',#43349);
#10985=VERTEX_POINT('',#43396);
#10986=VERTEX_POINT('',#43397);
#10987=VERTEX_POINT('',#43444);
#10988=VERTEX_POINT('',#43445);
#10989=VERTEX_POINT('',#43498);
#10990=VERTEX_POINT('',#43499);
#10991=VERTEX_POINT('',#43546);
#10992=VERTEX_POINT('',#43547);
#10993=VERTEX_POINT('',#43594);
#10994=VERTEX_POINT('',#43595);
#10995=VERTEX_POINT('',#43645);
#10996=VERTEX_POINT('',#43646);
#10997=VERTEX_POINT('',#43696);
#10998=VERTEX_POINT('',#43697);
#10999=VERTEX_POINT('',#43744);
#11000=VERTEX_POINT('',#43745);
#11001=VERTEX_POINT('',#43792);
#11002=VERTEX_POINT('',#43793);
#11003=VERTEX_POINT('',#43846);
#11004=VERTEX_POINT('',#43847);
#11005=VERTEX_POINT('',#43894);
#11006=VERTEX_POINT('',#43895);
#11007=VERTEX_POINT('',#43942);
#11008=VERTEX_POINT('',#43943);
#11009=VERTEX_POINT('',#43996);
#11010=VERTEX_POINT('',#43997);
#11011=VERTEX_POINT('',#44044);
#11012=VERTEX_POINT('',#44045);
#11013=VERTEX_POINT('',#44092);
#11014=VERTEX_POINT('',#44093);
#11015=VERTEX_POINT('',#44140);
#11016=VERTEX_POINT('',#44141);
#11017=VERTEX_POINT('',#44194);
#11018=VERTEX_POINT('',#44195);
#11019=VERTEX_POINT('',#44242);
#11020=VERTEX_POINT('',#44243);
#11021=VERTEX_POINT('',#44290);
#11022=VERTEX_POINT('',#44291);
#11023=VERTEX_POINT('',#44344);
#11024=VERTEX_POINT('',#44345);
#11025=VERTEX_POINT('',#44392);
#11026=VERTEX_POINT('',#44393);
#11027=VERTEX_POINT('',#44440);
#11028=VERTEX_POINT('',#44441);
#11029=VERTEX_POINT('',#44488);
#11030=VERTEX_POINT('',#44489);
#11031=VERTEX_POINT('',#44542);
#11032=VERTEX_POINT('',#44543);
#11033=VERTEX_POINT('',#44545);
#11034=VERTEX_POINT('',#44552);
#11035=VERTEX_POINT('',#44560);
#11036=VERTEX_POINT('',#44561);
#11037=VERTEX_POINT('',#44585);
#11038=VERTEX_POINT('',#44586);
#11039=VERTEX_POINT('',#44610);
#11040=VERTEX_POINT('',#44611);
#11041=VERTEX_POINT('',#44634);
#11042=VERTEX_POINT('',#44635);
#11043=VERTEX_POINT('',#44658);
#11044=VERTEX_POINT('',#44659);
#11045=VERTEX_POINT('',#44683);
#11046=VERTEX_POINT('',#44684);
#11047=VERTEX_POINT('',#44708);
#11048=VERTEX_POINT('',#44709);
#11049=VERTEX_POINT('',#44732);
#11050=VERTEX_POINT('',#44733);
#11051=VERTEX_POINT('',#44757);
#11052=VERTEX_POINT('',#44758);
#11053=VERTEX_POINT('',#44782);
#11054=VERTEX_POINT('',#44783);
#11055=VERTEX_POINT('',#44806);
#11056=VERTEX_POINT('',#44807);
#11057=VERTEX_POINT('',#44830);
#11058=VERTEX_POINT('',#44831);
#11059=VERTEX_POINT('',#44855);
#11060=VERTEX_POINT('',#44856);
#11061=VERTEX_POINT('',#44880);
#11062=VERTEX_POINT('',#44881);
#11063=VERTEX_POINT('',#44904);
#11064=VERTEX_POINT('',#44905);
#11065=VERTEX_POINT('',#44929);
#11066=VERTEX_POINT('',#44930);
#11067=VERTEX_POINT('',#44954);
#11068=VERTEX_POINT('',#44955);
#11069=VERTEX_POINT('',#44978);
#11070=VERTEX_POINT('',#44979);
#11071=VERTEX_POINT('',#45003);
#11072=VERTEX_POINT('',#45004);
#11073=VERTEX_POINT('',#45027);
#11074=VERTEX_POINT('',#45028);
#11075=VERTEX_POINT('',#45052);
#11076=VERTEX_POINT('',#45053);
#11077=VERTEX_POINT('',#45076);
#11078=VERTEX_POINT('',#45077);
#11079=VERTEX_POINT('',#45101);
#11080=VERTEX_POINT('',#45102);
#11081=VERTEX_POINT('',#45126);
#11082=VERTEX_POINT('',#45127);
#11083=VERTEX_POINT('',#45150);
#11084=VERTEX_POINT('',#45151);
#11085=VERTEX_POINT('',#45175);
#11086=VERTEX_POINT('',#45176);
#11087=VERTEX_POINT('',#45200);
#11088=VERTEX_POINT('',#45201);
#11089=VERTEX_POINT('',#45224);
#11090=VERTEX_POINT('',#45225);
#11091=VERTEX_POINT('',#45248);
#11092=VERTEX_POINT('',#45249);
#11093=VERTEX_POINT('',#45273);
#11094=VERTEX_POINT('',#45274);
#11095=VERTEX_POINT('',#45298);
#11096=VERTEX_POINT('',#45299);
#11097=VERTEX_POINT('',#45322);
#11098=VERTEX_POINT('',#45323);
#11099=VERTEX_POINT('',#45347);
#11100=VERTEX_POINT('',#45348);
#11101=VERTEX_POINT('',#45372);
#11102=VERTEX_POINT('',#45373);
#11103=VERTEX_POINT('',#45396);
#11104=VERTEX_POINT('',#45397);
#11105=VERTEX_POINT('',#45420);
#11106=VERTEX_POINT('',#45421);
#11107=VERTEX_POINT('',#45445);
#11108=VERTEX_POINT('',#45446);
#11109=VERTEX_POINT('',#45470);
#11110=VERTEX_POINT('',#45471);
#11111=VERTEX_POINT('',#45494);
#11112=VERTEX_POINT('',#45495);
#11113=VERTEX_POINT('',#45519);
#11114=VERTEX_POINT('',#45520);
#11115=VERTEX_POINT('',#45544);
#11116=VERTEX_POINT('',#45545);
#11117=VERTEX_POINT('',#45568);
#11118=VERTEX_POINT('',#45569);
#11119=VERTEX_POINT('',#45593);
#11120=VERTEX_POINT('',#45594);
#11121=VERTEX_POINT('',#45617);
#11122=VERTEX_POINT('',#45618);
#11123=VERTEX_POINT('',#45642);
#11124=VERTEX_POINT('',#45643);
#11125=VERTEX_POINT('',#45666);
#11126=VERTEX_POINT('',#45667);
#11127=VERTEX_POINT('',#45691);
#11128=VERTEX_POINT('',#45692);
#11129=VERTEX_POINT('',#45716);
#11130=VERTEX_POINT('',#45717);
#11131=VERTEX_POINT('',#45740);
#11132=VERTEX_POINT('',#45741);
#11133=VERTEX_POINT('',#45765);
#11134=VERTEX_POINT('',#45766);
#11135=VERTEX_POINT('',#45790);
#11136=VERTEX_POINT('',#45791);
#11137=VERTEX_POINT('',#45814);
#11138=VERTEX_POINT('',#45815);
#11139=VERTEX_POINT('',#45838);
#11140=VERTEX_POINT('',#45839);
#11141=VERTEX_POINT('',#45863);
#11142=VERTEX_POINT('',#45864);
#11143=VERTEX_POINT('',#45888);
#11144=VERTEX_POINT('',#45889);
#11145=VERTEX_POINT('',#45912);
#11146=VERTEX_POINT('',#45913);
#11147=VERTEX_POINT('',#45937);
#11148=VERTEX_POINT('',#45938);
#11149=VERTEX_POINT('',#45962);
#11150=VERTEX_POINT('',#45963);
#11151=VERTEX_POINT('',#45986);
#11152=VERTEX_POINT('',#46039);
#11153=VERTEX_POINT('',#46041);
#11154=VERTEX_POINT('',#47606);
#11155=VERTEX_POINT('',#47665);
#11156=VERTEX_POINT('',#49233);
#11157=VERTEX_POINT('',#49234);
#11158=VERTEX_POINT('',#49236);
#11159=VERTEX_POINT('',#49240);
#11160=VERTEX_POINT('',#49242);
#11161=VERTEX_POINT('',#49248);
#11162=VERTEX_POINT('',#49254);
#11163=VERTEX_POINT('',#49255);
#11164=VERTEX_POINT('',#49257);
#11165=VERTEX_POINT('',#49261);
#11166=VERTEX_POINT('',#49263);
#11167=VERTEX_POINT('',#49269);
#11168=VERTEX_POINT('',#49275);
#11169=VERTEX_POINT('',#49276);
#11170=VERTEX_POINT('',#49278);
#11171=VERTEX_POINT('',#49282);
#11172=VERTEX_POINT('',#49284);
#11173=VERTEX_POINT('',#49290);
#11174=VERTEX_POINT('',#49296);
#11175=VERTEX_POINT('',#49297);
#11176=VERTEX_POINT('',#49299);
#11177=VERTEX_POINT('',#49303);
#11178=VERTEX_POINT('',#49305);
#11179=VERTEX_POINT('',#49311);
#11180=VERTEX_POINT('',#49317);
#11181=VERTEX_POINT('',#49318);
#11182=VERTEX_POINT('',#49320);
#11183=VERTEX_POINT('',#49324);
#11184=VERTEX_POINT('',#49326);
#11185=VERTEX_POINT('',#49332);
#11186=VERTEX_POINT('',#49338);
#11187=VERTEX_POINT('',#49339);
#11188=VERTEX_POINT('',#49341);
#11189=VERTEX_POINT('',#49345);
#11190=VERTEX_POINT('',#49347);
#11191=VERTEX_POINT('',#49353);
#11192=VERTEX_POINT('',#49359);
#11193=VERTEX_POINT('',#49360);
#11194=VERTEX_POINT('',#49362);
#11195=VERTEX_POINT('',#49366);
#11196=VERTEX_POINT('',#49368);
#11197=VERTEX_POINT('',#49374);
#11198=VERTEX_POINT('',#49380);
#11199=VERTEX_POINT('',#49381);
#11200=VERTEX_POINT('',#49383);
#11201=VERTEX_POINT('',#49387);
#11202=VERTEX_POINT('',#49389);
#11203=VERTEX_POINT('',#49395);
#11204=VERTEX_POINT('',#49401);
#11205=VERTEX_POINT('',#49402);
#11206=VERTEX_POINT('',#49404);
#11207=VERTEX_POINT('',#49408);
#11208=VERTEX_POINT('',#49410);
#11209=VERTEX_POINT('',#49416);
#11210=VERTEX_POINT('',#49422);
#11211=VERTEX_POINT('',#49423);
#11212=VERTEX_POINT('',#49425);
#11213=VERTEX_POINT('',#49429);
#11214=VERTEX_POINT('',#49431);
#11215=VERTEX_POINT('',#49437);
#11216=VERTEX_POINT('',#49443);
#11217=VERTEX_POINT('',#49444);
#11218=VERTEX_POINT('',#49446);
#11219=VERTEX_POINT('',#49450);
#11220=VERTEX_POINT('',#49452);
#11221=VERTEX_POINT('',#49458);
#11222=VERTEX_POINT('',#49464);
#11223=VERTEX_POINT('',#49465);
#11224=VERTEX_POINT('',#49467);
#11225=VERTEX_POINT('',#49471);
#11226=VERTEX_POINT('',#49473);
#11227=VERTEX_POINT('',#49479);
#11228=VERTEX_POINT('',#49485);
#11229=VERTEX_POINT('',#49486);
#11230=VERTEX_POINT('',#49488);
#11231=VERTEX_POINT('',#49492);
#11232=VERTEX_POINT('',#49494);
#11233=VERTEX_POINT('',#49500);
#11234=VERTEX_POINT('',#49506);
#11235=VERTEX_POINT('',#49507);
#11236=VERTEX_POINT('',#49509);
#11237=VERTEX_POINT('',#49513);
#11238=VERTEX_POINT('',#49515);
#11239=VERTEX_POINT('',#49521);
#11240=VERTEX_POINT('',#49527);
#11241=VERTEX_POINT('',#49528);
#11242=VERTEX_POINT('',#49530);
#11243=VERTEX_POINT('',#49534);
#11244=VERTEX_POINT('',#49536);
#11245=VERTEX_POINT('',#49542);
#11246=VERTEX_POINT('',#49548);
#11247=VERTEX_POINT('',#49549);
#11248=VERTEX_POINT('',#49551);
#11249=VERTEX_POINT('',#49555);
#11250=VERTEX_POINT('',#49557);
#11251=VERTEX_POINT('',#49563);
#11252=VERTEX_POINT('',#49569);
#11253=VERTEX_POINT('',#49570);
#11254=VERTEX_POINT('',#49572);
#11255=VERTEX_POINT('',#49576);
#11256=VERTEX_POINT('',#49578);
#11257=VERTEX_POINT('',#49584);
#11258=VERTEX_POINT('',#49590);
#11259=VERTEX_POINT('',#49591);
#11260=VERTEX_POINT('',#49593);
#11261=VERTEX_POINT('',#49595);
#11262=VERTEX_POINT('',#49599);
#11263=VERTEX_POINT('',#49601);
#11264=VERTEX_POINT('',#49607);
#11265=VERTEX_POINT('',#49613);
#11266=VERTEX_POINT('',#49614);
#11267=VERTEX_POINT('',#49616);
#11268=VERTEX_POINT('',#49620);
#11269=VERTEX_POINT('',#49622);
#11270=VERTEX_POINT('',#49628);
#11271=VERTEX_POINT('',#49634);
#11272=VERTEX_POINT('',#49635);
#11273=VERTEX_POINT('',#49637);
#11274=VERTEX_POINT('',#49641);
#11275=VERTEX_POINT('',#49643);
#11276=VERTEX_POINT('',#49649);
#11277=VERTEX_POINT('',#49655);
#11278=VERTEX_POINT('',#49656);
#11279=VERTEX_POINT('',#49658);
#11280=VERTEX_POINT('',#49662);
#11281=VERTEX_POINT('',#49664);
#11282=VERTEX_POINT('',#49670);
#11283=VERTEX_POINT('',#49676);
#11284=VERTEX_POINT('',#49677);
#11285=VERTEX_POINT('',#49679);
#11286=VERTEX_POINT('',#49683);
#11287=VERTEX_POINT('',#49685);
#11288=VERTEX_POINT('',#49691);
#11289=VERTEX_POINT('',#49697);
#11290=VERTEX_POINT('',#49698);
#11291=VERTEX_POINT('',#49700);
#11292=VERTEX_POINT('',#49704);
#11293=VERTEX_POINT('',#49706);
#11294=VERTEX_POINT('',#49712);
#11295=VERTEX_POINT('',#49718);
#11296=VERTEX_POINT('',#49719);
#11297=VERTEX_POINT('',#49721);
#11298=VERTEX_POINT('',#49725);
#11299=VERTEX_POINT('',#49727);
#11300=VERTEX_POINT('',#49733);
#11301=VERTEX_POINT('',#49739);
#11302=VERTEX_POINT('',#49740);
#11303=VERTEX_POINT('',#49742);
#11304=VERTEX_POINT('',#49746);
#11305=VERTEX_POINT('',#49748);
#11306=VERTEX_POINT('',#49754);
#11307=VERTEX_POINT('',#49760);
#11308=VERTEX_POINT('',#49761);
#11309=VERTEX_POINT('',#49763);
#11310=VERTEX_POINT('',#49767);
#11311=VERTEX_POINT('',#49769);
#11312=VERTEX_POINT('',#49775);
#11313=VERTEX_POINT('',#49781);
#11314=VERTEX_POINT('',#49782);
#11315=VERTEX_POINT('',#49784);
#11316=VERTEX_POINT('',#49788);
#11317=VERTEX_POINT('',#49790);
#11318=VERTEX_POINT('',#49796);
#11319=VERTEX_POINT('',#49802);
#11320=VERTEX_POINT('',#49803);
#11321=VERTEX_POINT('',#49805);
#11322=VERTEX_POINT('',#49809);
#11323=VERTEX_POINT('',#49811);
#11324=VERTEX_POINT('',#49817);
#11325=VERTEX_POINT('',#49823);
#11326=VERTEX_POINT('',#49824);
#11327=VERTEX_POINT('',#49826);
#11328=VERTEX_POINT('',#49830);
#11329=VERTEX_POINT('',#49832);
#11330=VERTEX_POINT('',#49838);
#11331=VERTEX_POINT('',#49844);
#11332=VERTEX_POINT('',#49845);
#11333=VERTEX_POINT('',#49847);
#11334=VERTEX_POINT('',#49851);
#11335=VERTEX_POINT('',#49853);
#11336=VERTEX_POINT('',#49859);
#11337=VERTEX_POINT('',#49865);
#11338=VERTEX_POINT('',#49866);
#11339=VERTEX_POINT('',#49868);
#11340=VERTEX_POINT('',#49872);
#11341=VERTEX_POINT('',#49874);
#11342=VERTEX_POINT('',#49880);
#11343=VERTEX_POINT('',#49886);
#11344=VERTEX_POINT('',#49887);
#11345=VERTEX_POINT('',#49889);
#11346=VERTEX_POINT('',#49893);
#11347=VERTEX_POINT('',#49895);
#11348=VERTEX_POINT('',#49901);
#11349=VERTEX_POINT('',#49907);
#11350=VERTEX_POINT('',#49908);
#11351=VERTEX_POINT('',#49910);
#11352=VERTEX_POINT('',#49914);
#11353=VERTEX_POINT('',#49916);
#11354=VERTEX_POINT('',#49922);
#11355=VERTEX_POINT('',#49928);
#11356=VERTEX_POINT('',#49929);
#11357=VERTEX_POINT('',#49931);
#11358=VERTEX_POINT('',#49935);
#11359=VERTEX_POINT('',#49937);
#11360=VERTEX_POINT('',#49943);
#11361=VERTEX_POINT('',#49949);
#11362=VERTEX_POINT('',#49950);
#11363=VERTEX_POINT('',#49952);
#11364=VERTEX_POINT('',#49956);
#11365=VERTEX_POINT('',#49958);
#11366=VERTEX_POINT('',#49964);
#11367=VERTEX_POINT('',#49987);
#11368=VERTEX_POINT('',#50007);
#11369=VERTEX_POINT('',#50009);
#11370=VERTEX_POINT('',#50011);
#11371=VERTEX_POINT('',#50013);
#11372=VERTEX_POINT('',#50017);
#11373=VERTEX_POINT('',#50019);
#11374=VERTEX_POINT('',#50031);
#11375=VERTEX_POINT('',#50035);
#11376=VERTEX_POINT('',#50036);
#11377=VERTEX_POINT('',#50040);
#11378=VERTEX_POINT('',#50041);
#11379=VERTEX_POINT('',#50043);
#11380=VERTEX_POINT('',#50045);
#11381=VERTEX_POINT('',#50049);
#11382=VERTEX_POINT('',#50051);
#11383=VERTEX_POINT('',#50055);
#11384=VERTEX_POINT('',#50057);
#11385=VERTEX_POINT('',#50061);
#11386=VERTEX_POINT('',#50063);
#11387=VERTEX_POINT('',#50067);
#11388=VERTEX_POINT('',#50069);
#11389=VERTEX_POINT('',#50077);
#11390=VERTEX_POINT('',#50084);
#11391=VERTEX_POINT('',#50091);
#11392=VERTEX_POINT('',#50092);
#11393=VERTEX_POINT('',#50094);
#11394=VERTEX_POINT('',#50117);
#11395=VERTEX_POINT('',#50119);
#11396=VERTEX_POINT('',#50122);
#11397=VERTEX_POINT('',#50144);
#11398=VERTEX_POINT('',#50145);
#11399=VERTEX_POINT('',#50192);
#11400=VERTEX_POINT('',#50193);
#11401=VERTEX_POINT('',#50240);
#11402=VERTEX_POINT('',#50241);
#11403=VERTEX_POINT('',#50288);
#11404=VERTEX_POINT('',#50289);
#11405=VERTEX_POINT('',#50342);
#11406=VERTEX_POINT('',#50343);
#11407=VERTEX_POINT('',#50390);
#11408=VERTEX_POINT('',#50391);
#11409=VERTEX_POINT('',#50438);
#11410=VERTEX_POINT('',#50439);
#11411=VERTEX_POINT('',#50492);
#11412=VERTEX_POINT('',#50493);
#11413=VERTEX_POINT('',#50540);
#11414=VERTEX_POINT('',#50541);
#11415=VERTEX_POINT('',#50588);
#11416=VERTEX_POINT('',#50589);
#11417=VERTEX_POINT('',#50636);
#11418=VERTEX_POINT('',#50637);
#11419=VERTEX_POINT('',#50690);
#11420=VERTEX_POINT('',#50691);
#11421=VERTEX_POINT('',#50738);
#11422=VERTEX_POINT('',#50739);
#11423=VERTEX_POINT('',#50786);
#11424=VERTEX_POINT('',#50787);
#11425=VERTEX_POINT('',#50840);
#11426=VERTEX_POINT('',#50841);
#11427=VERTEX_POINT('',#50888);
#11428=VERTEX_POINT('',#50889);
#11429=VERTEX_POINT('',#50936);
#11430=VERTEX_POINT('',#50937);
#11431=VERTEX_POINT('',#50984);
#11432=VERTEX_POINT('',#50985);
#11433=VERTEX_POINT('',#50987);
#11434=VERTEX_POINT('',#50995);
#11435=VERTEX_POINT('',#51003);
#11436=VERTEX_POINT('',#51004);
#11437=VERTEX_POINT('',#51028);
#11438=VERTEX_POINT('',#51029);
#11439=VERTEX_POINT('',#51052);
#11440=VERTEX_POINT('',#51053);
#11441=VERTEX_POINT('',#51076);
#11442=VERTEX_POINT('',#51077);
#11443=VERTEX_POINT('',#51101);
#11444=VERTEX_POINT('',#51102);
#11445=VERTEX_POINT('',#51126);
#11446=VERTEX_POINT('',#51127);
#11447=VERTEX_POINT('',#51150);
#11448=VERTEX_POINT('',#51151);
#11449=VERTEX_POINT('',#51175);
#11450=VERTEX_POINT('',#51176);
#11451=VERTEX_POINT('',#51200);
#11452=VERTEX_POINT('',#51201);
#11453=VERTEX_POINT('',#51224);
#11454=VERTEX_POINT('',#51225);
#11455=VERTEX_POINT('',#51248);
#11456=VERTEX_POINT('',#51249);
#11457=VERTEX_POINT('',#51273);
#11458=VERTEX_POINT('',#51274);
#11459=VERTEX_POINT('',#51298);
#11460=VERTEX_POINT('',#51299);
#11461=VERTEX_POINT('',#51322);
#11462=VERTEX_POINT('',#51323);
#11463=VERTEX_POINT('',#51347);
#11464=VERTEX_POINT('',#51348);
#11465=VERTEX_POINT('',#51372);
#11466=VERTEX_POINT('',#51373);
#11467=VERTEX_POINT('',#51396);
#11468=VERTEX_POINT('',#51397);
#11469=VERTEX_POINT('',#51420);
#11470=VERTEX_POINT('',#51421);
#11471=VERTEX_POINT('',#51445);
#11472=VERTEX_POINT('',#51504);
#11473=VERTEX_POINT('',#51506);
#11474=VERTEX_POINT('',#52080);
#11475=VERTEX_POINT('',#52147);
#11476=VERTEX_POINT('',#52725);
#11477=VERTEX_POINT('',#52726);
#11478=VERTEX_POINT('',#52728);
#11479=VERTEX_POINT('',#52732);
#11480=VERTEX_POINT('',#52734);
#11481=VERTEX_POINT('',#52740);
#11482=VERTEX_POINT('',#52746);
#11483=VERTEX_POINT('',#52747);
#11484=VERTEX_POINT('',#52749);
#11485=VERTEX_POINT('',#52753);
#11486=VERTEX_POINT('',#52755);
#11487=VERTEX_POINT('',#52761);
#11488=VERTEX_POINT('',#52767);
#11489=VERTEX_POINT('',#52768);
#11490=VERTEX_POINT('',#52770);
#11491=VERTEX_POINT('',#52774);
#11492=VERTEX_POINT('',#52776);
#11493=VERTEX_POINT('',#52782);
#11494=VERTEX_POINT('',#52788);
#11495=VERTEX_POINT('',#52789);
#11496=VERTEX_POINT('',#52791);
#11497=VERTEX_POINT('',#52795);
#11498=VERTEX_POINT('',#52797);
#11499=VERTEX_POINT('',#52803);
#11500=VERTEX_POINT('',#52809);
#11501=VERTEX_POINT('',#52810);
#11502=VERTEX_POINT('',#52812);
#11503=VERTEX_POINT('',#52816);
#11504=VERTEX_POINT('',#52818);
#11505=VERTEX_POINT('',#52824);
#11506=VERTEX_POINT('',#52830);
#11507=VERTEX_POINT('',#52831);
#11508=VERTEX_POINT('',#52833);
#11509=VERTEX_POINT('',#52837);
#11510=VERTEX_POINT('',#52839);
#11511=VERTEX_POINT('',#52845);
#11512=VERTEX_POINT('',#52851);
#11513=VERTEX_POINT('',#52852);
#11514=VERTEX_POINT('',#52854);
#11515=VERTEX_POINT('',#52858);
#11516=VERTEX_POINT('',#52860);
#11517=VERTEX_POINT('',#52866);
#11518=VERTEX_POINT('',#52872);
#11519=VERTEX_POINT('',#52873);
#11520=VERTEX_POINT('',#52875);
#11521=VERTEX_POINT('',#52879);
#11522=VERTEX_POINT('',#52881);
#11523=VERTEX_POINT('',#52887);
#11524=VERTEX_POINT('',#52893);
#11525=VERTEX_POINT('',#52894);
#11526=VERTEX_POINT('',#52896);
#11527=VERTEX_POINT('',#52900);
#11528=VERTEX_POINT('',#52902);
#11529=VERTEX_POINT('',#52908);
#11530=VERTEX_POINT('',#52914);
#11531=VERTEX_POINT('',#52915);
#11532=VERTEX_POINT('',#52917);
#11533=VERTEX_POINT('',#52921);
#11534=VERTEX_POINT('',#52923);
#11535=VERTEX_POINT('',#52929);
#11536=VERTEX_POINT('',#52935);
#11537=VERTEX_POINT('',#52936);
#11538=VERTEX_POINT('',#52938);
#11539=VERTEX_POINT('',#52942);
#11540=VERTEX_POINT('',#52944);
#11541=VERTEX_POINT('',#52950);
#11542=VERTEX_POINT('',#52956);
#11543=VERTEX_POINT('',#52957);
#11544=VERTEX_POINT('',#52959);
#11545=VERTEX_POINT('',#52963);
#11546=VERTEX_POINT('',#52965);
#11547=VERTEX_POINT('',#52971);
#11548=VERTEX_POINT('',#52977);
#11549=VERTEX_POINT('',#52978);
#11550=VERTEX_POINT('',#52980);
#11551=VERTEX_POINT('',#52984);
#11552=VERTEX_POINT('',#52986);
#11553=VERTEX_POINT('',#52992);
#11554=VERTEX_POINT('',#52998);
#11555=VERTEX_POINT('',#52999);
#11556=VERTEX_POINT('',#53001);
#11557=VERTEX_POINT('',#53005);
#11558=VERTEX_POINT('',#53007);
#11559=VERTEX_POINT('',#53013);
#11560=VERTEX_POINT('',#53019);
#11561=VERTEX_POINT('',#53020);
#11562=VERTEX_POINT('',#53022);
#11563=VERTEX_POINT('',#53026);
#11564=VERTEX_POINT('',#53028);
#11565=VERTEX_POINT('',#53034);
#11566=VERTEX_POINT('',#53040);
#11567=VERTEX_POINT('',#53041);
#11568=VERTEX_POINT('',#53043);
#11569=VERTEX_POINT('',#53047);
#11570=VERTEX_POINT('',#53049);
#11571=VERTEX_POINT('',#53055);
#11572=VERTEX_POINT('',#53061);
#11573=VERTEX_POINT('',#53062);
#11574=VERTEX_POINT('',#53064);
#11575=VERTEX_POINT('',#53068);
#11576=VERTEX_POINT('',#53070);
#11577=VERTEX_POINT('',#53076);
#11578=VERTEX_POINT('',#53082);
#11579=VERTEX_POINT('',#53083);
#11580=VERTEX_POINT('',#53085);
#11581=VERTEX_POINT('',#53087);
#11582=VERTEX_POINT('',#53091);
#11583=VERTEX_POINT('',#53093);
#11584=VERTEX_POINT('',#53099);
#11585=VERTEX_POINT('',#53105);
#11586=VERTEX_POINT('',#53106);
#11587=VERTEX_POINT('',#53108);
#11588=VERTEX_POINT('',#53112);
#11589=VERTEX_POINT('',#53114);
#11590=VERTEX_POINT('',#53120);
#11591=VERTEX_POINT('',#53126);
#11592=VERTEX_POINT('',#53127);
#11593=VERTEX_POINT('',#53129);
#11594=VERTEX_POINT('',#53133);
#11595=VERTEX_POINT('',#53135);
#11596=VERTEX_POINT('',#53141);
#11597=VERTEX_POINT('',#53147);
#11598=VERTEX_POINT('',#53148);
#11599=VERTEX_POINT('',#53150);
#11600=VERTEX_POINT('',#53154);
#11601=VERTEX_POINT('',#53156);
#11602=VERTEX_POINT('',#53162);
#11603=VERTEX_POINT('',#53168);
#11604=VERTEX_POINT('',#53169);
#11605=VERTEX_POINT('',#53171);
#11606=VERTEX_POINT('',#53175);
#11607=VERTEX_POINT('',#53177);
#11608=VERTEX_POINT('',#53183);
#11609=VERTEX_POINT('',#53189);
#11610=VERTEX_POINT('',#53190);
#11611=VERTEX_POINT('',#53192);
#11612=VERTEX_POINT('',#53196);
#11613=VERTEX_POINT('',#53198);
#11614=VERTEX_POINT('',#53204);
#11615=VERTEX_POINT('',#53210);
#11616=VERTEX_POINT('',#53211);
#11617=VERTEX_POINT('',#53213);
#11618=VERTEX_POINT('',#53217);
#11619=VERTEX_POINT('',#53219);
#11620=VERTEX_POINT('',#53225);
#11621=VERTEX_POINT('',#53231);
#11622=VERTEX_POINT('',#53232);
#11623=VERTEX_POINT('',#53234);
#11624=VERTEX_POINT('',#53238);
#11625=VERTEX_POINT('',#53240);
#11626=VERTEX_POINT('',#53246);
#11627=VERTEX_POINT('',#53252);
#11628=VERTEX_POINT('',#53253);
#11629=VERTEX_POINT('',#53255);
#11630=VERTEX_POINT('',#53259);
#11631=VERTEX_POINT('',#53261);
#11632=VERTEX_POINT('',#53267);
#11633=VERTEX_POINT('',#53273);
#11634=VERTEX_POINT('',#53274);
#11635=VERTEX_POINT('',#53276);
#11636=VERTEX_POINT('',#53280);
#11637=VERTEX_POINT('',#53282);
#11638=VERTEX_POINT('',#53288);
#11639=VERTEX_POINT('',#53294);
#11640=VERTEX_POINT('',#53295);
#11641=VERTEX_POINT('',#53297);
#11642=VERTEX_POINT('',#53301);
#11643=VERTEX_POINT('',#53303);
#11644=VERTEX_POINT('',#53309);
#11645=VERTEX_POINT('',#53315);
#11646=VERTEX_POINT('',#53316);
#11647=VERTEX_POINT('',#53318);
#11648=VERTEX_POINT('',#53322);
#11649=VERTEX_POINT('',#53324);
#11650=VERTEX_POINT('',#53330);
#11651=VERTEX_POINT('',#53336);
#11652=VERTEX_POINT('',#53337);
#11653=VERTEX_POINT('',#53339);
#11654=VERTEX_POINT('',#53343);
#11655=VERTEX_POINT('',#53345);
#11656=VERTEX_POINT('',#53351);
#11657=VERTEX_POINT('',#53357);
#11658=VERTEX_POINT('',#53358);
#11659=VERTEX_POINT('',#53360);
#11660=VERTEX_POINT('',#53364);
#11661=VERTEX_POINT('',#53366);
#11662=VERTEX_POINT('',#53372);
#11663=VERTEX_POINT('',#53378);
#11664=VERTEX_POINT('',#53379);
#11665=VERTEX_POINT('',#53381);
#11666=VERTEX_POINT('',#53385);
#11667=VERTEX_POINT('',#53387);
#11668=VERTEX_POINT('',#53393);
#11669=VERTEX_POINT('',#53399);
#11670=VERTEX_POINT('',#53400);
#11671=VERTEX_POINT('',#53402);
#11672=VERTEX_POINT('',#53406);
#11673=VERTEX_POINT('',#53408);
#11674=VERTEX_POINT('',#53414);
#11675=VERTEX_POINT('',#53420);
#11676=VERTEX_POINT('',#53421);
#11677=VERTEX_POINT('',#53423);
#11678=VERTEX_POINT('',#53427);
#11679=VERTEX_POINT('',#53429);
#11680=VERTEX_POINT('',#53435);
#11681=VERTEX_POINT('',#53441);
#11682=VERTEX_POINT('',#53442);
#11683=VERTEX_POINT('',#53444);
#11684=VERTEX_POINT('',#53448);
#11685=VERTEX_POINT('',#53450);
#11686=VERTEX_POINT('',#53456);
#11687=VERTEX_POINT('',#53479);
#11688=VERTEX_POINT('',#53499);
#11689=VERTEX_POINT('',#53501);
#11690=VERTEX_POINT('',#53503);
#11691=VERTEX_POINT('',#53505);
#11692=VERTEX_POINT('',#53509);
#11693=VERTEX_POINT('',#53511);
#11694=VERTEX_POINT('',#53523);
#11695=VERTEX_POINT('',#53527);
#11696=VERTEX_POINT('',#53528);
#11697=VERTEX_POINT('',#53532);
#11698=VERTEX_POINT('',#53533);
#11699=VERTEX_POINT('',#53535);
#11700=VERTEX_POINT('',#53537);
#11701=VERTEX_POINT('',#53541);
#11702=VERTEX_POINT('',#53543);
#11703=VERTEX_POINT('',#53547);
#11704=VERTEX_POINT('',#53549);
#11705=VERTEX_POINT('',#53553);
#11706=VERTEX_POINT('',#53555);
#11707=VERTEX_POINT('',#53559);
#11708=VERTEX_POINT('',#53561);
#11709=VERTEX_POINT('',#53569);
#11710=VERTEX_POINT('',#53576);
#11711=EDGE_CURVE('',#9542,#9543,#5852,.T.);
#11712=EDGE_CURVE('',#9543,#9544,#5063,.T.);
#11713=EDGE_CURVE('',#9544,#9545,#5853,.T.);
#11714=EDGE_CURVE('',#9545,#9542,#5064,.T.);
#11715=EDGE_CURVE('',#9546,#9547,#5854,.T.);
#11716=EDGE_CURVE('',#9547,#9543,#5855,.T.);
#11717=EDGE_CURVE('',#9542,#9546,#5856,.T.);
#11718=EDGE_CURVE('',#9548,#9549,#5857,.T.);
#11719=EDGE_CURVE('',#9549,#9547,#5065,.T.);
#11720=EDGE_CURVE('',#9546,#9548,#5066,.T.);
#11721=EDGE_CURVE('',#9550,#9551,#5858,.T.);
#11722=EDGE_CURVE('',#9551,#9549,#5859,.T.);
#11723=EDGE_CURVE('',#9548,#9550,#5860,.T.);
#11724=EDGE_CURVE('',#9552,#9553,#5861,.T.);
#11725=EDGE_CURVE('',#9553,#9551,#5067,.T.);
#11726=EDGE_CURVE('',#9550,#9552,#5068,.T.);
#11727=EDGE_CURVE('',#9554,#9555,#5862,.T.);
#11728=EDGE_CURVE('',#9555,#9553,#5863,.T.);
#11729=EDGE_CURVE('',#9552,#9554,#5864,.T.);
#11730=EDGE_CURVE('',#9556,#9557,#5865,.T.);
#11731=EDGE_CURVE('',#9557,#9555,#5069,.T.);
#11732=EDGE_CURVE('',#9554,#9556,#5070,.T.);
#11733=EDGE_CURVE('',#9544,#9557,#5866,.T.);
#11734=EDGE_CURVE('',#9556,#9545,#5867,.T.);
#11735=EDGE_CURVE('',#9555,#9558,#5868,.T.);
#11736=EDGE_CURVE('',#9559,#9558,#5869,.T.);
#11737=EDGE_CURVE('',#9553,#9559,#5870,.T.);
#11738=EDGE_CURVE('',#9557,#9560,#5871,.T.);
#11739=EDGE_CURVE('',#9558,#9560,#5071,.T.);
#11740=EDGE_CURVE('',#9561,#9544,#5872,.T.);
#11741=EDGE_CURVE('',#9560,#9561,#5873,.T.);
#11742=EDGE_CURVE('',#9543,#9562,#5874,.T.);
#11743=EDGE_CURVE('',#9561,#9562,#5072,.T.);
#11744=EDGE_CURVE('',#9563,#9563,#5073,.T.);
#11745=EDGE_CURVE('',#9564,#9564,#5074,.T.);
#11746=EDGE_CURVE('',#9565,#9565,#5075,.T.);
#11747=EDGE_CURVE('',#9566,#9566,#5076,.T.);
#11748=EDGE_CURVE('',#9567,#9567,#5077,.T.);
#11749=EDGE_CURVE('',#9568,#9568,#5078,.T.);
#11750=EDGE_CURVE('',#9569,#9569,#5079,.T.);
#11751=EDGE_CURVE('',#9570,#9561,#5875,.T.);
#11752=EDGE_CURVE('',#9562,#9571,#5876,.T.);
#11753=EDGE_CURVE('',#9571,#9570,#5080,.T.);
#11754=EDGE_CURVE('',#9572,#9560,#5877,.T.);
#11755=EDGE_CURVE('',#9570,#9572,#5878,.T.);
#11756=EDGE_CURVE('',#9573,#9558,#5879,.T.);
#11757=EDGE_CURVE('',#9572,#9573,#5081,.T.);
#11758=EDGE_CURVE('',#9574,#9559,#5880,.T.);
#11759=EDGE_CURVE('',#9573,#9574,#5881,.T.);
#11760=EDGE_CURVE('',#9575,#9576,#5882,.T.);
#11761=EDGE_CURVE('',#9576,#9559,#5082,.T.);
#11762=EDGE_CURVE('',#9574,#9575,#5083,.T.);
#11763=EDGE_CURVE('',#9577,#9578,#5883,.T.);
#11764=EDGE_CURVE('',#9578,#9576,#5884,.T.);
#11765=EDGE_CURVE('',#9575,#9577,#5885,.T.);
#11766=EDGE_CURVE('',#9579,#9580,#5886,.T.);
#11767=EDGE_CURVE('',#9580,#9578,#5084,.T.);
#11768=EDGE_CURVE('',#9577,#9579,#5085,.T.);
#11769=EDGE_CURVE('',#9562,#9580,#5887,.T.);
#11770=EDGE_CURVE('',#9579,#9571,#5888,.T.);
#11771=EDGE_CURVE('',#9581,#9573,#5889,.T.);
#11772=EDGE_CURVE('',#9582,#9581,#5890,.T.);
#11773=EDGE_CURVE('',#9574,#9582,#5891,.T.);
#11774=EDGE_CURVE('',#9572,#9583,#5892,.T.);
#11775=EDGE_CURVE('',#9581,#9583,#5086,.T.);
#11776=EDGE_CURVE('',#9584,#9570,#5893,.T.);
#11777=EDGE_CURVE('',#9583,#9584,#5894,.T.);
#11778=EDGE_CURVE('',#9571,#9585,#5895,.T.);
#11779=EDGE_CURVE('',#9584,#9585,#5087,.T.);
#11780=EDGE_CURVE('',#9551,#9576,#5896,.T.);
#11781=EDGE_CURVE('',#9549,#9578,#5897,.T.);
#11782=EDGE_CURVE('',#9547,#9580,#5898,.T.);
#11783=EDGE_CURVE('',#9586,#9587,#5899,.T.);
#11784=EDGE_CURVE('',#9587,#9588,#5900,.T.);
#11785=EDGE_CURVE('',#9588,#9589,#5901,.T.);
#11786=EDGE_CURVE('',#9589,#9586,#5902,.T.);
#11787=EDGE_CURVE('',#9590,#9591,#5903,.T.);
#11788=EDGE_CURVE('',#9591,#9587,#5088,.T.);
#11789=EDGE_CURVE('',#9586,#9590,#5089,.T.);
#11790=EDGE_CURVE('',#9592,#9593,#5904,.T.);
#11791=EDGE_CURVE('',#9593,#9591,#5905,.T.);
#11792=EDGE_CURVE('',#9590,#9592,#5906,.T.);
#11793=EDGE_CURVE('',#9594,#9595,#5907,.T.);
#11794=EDGE_CURVE('',#9595,#9593,#5090,.T.);
#11795=EDGE_CURVE('',#9592,#9594,#5091,.T.);
#11796=EDGE_CURVE('',#9596,#9597,#5908,.T.);
#11797=EDGE_CURVE('',#9597,#9595,#5909,.T.);
#11798=EDGE_CURVE('',#9594,#9596,#5910,.T.);
#11799=EDGE_CURVE('',#9598,#9599,#5911,.T.);
#11800=EDGE_CURVE('',#9599,#9597,#5092,.T.);
#11801=EDGE_CURVE('',#9596,#9598,#5093,.T.);
#11802=EDGE_CURVE('',#9600,#9601,#5912,.T.);
#11803=EDGE_CURVE('',#9601,#9599,#5913,.T.);
#11804=EDGE_CURVE('',#9598,#9600,#5914,.T.);
#11805=EDGE_CURVE('',#9588,#9601,#5094,.T.);
#11806=EDGE_CURVE('',#9600,#9589,#5095,.T.);
#11807=EDGE_CURVE('',#9599,#9602,#5915,.T.);
#11808=EDGE_CURVE('',#9603,#9602,#5096,.T.);
#11809=EDGE_CURVE('',#9597,#9603,#5916,.T.);
#11810=EDGE_CURVE('',#9601,#9604,#5917,.T.);
#11811=EDGE_CURVE('',#9602,#9604,#5918,.T.);
#11812=EDGE_CURVE('',#9605,#9588,#5919,.T.);
#11813=EDGE_CURVE('',#9604,#9605,#5097,.T.);
#11814=EDGE_CURVE('',#9587,#9606,#5920,.T.);
#11815=EDGE_CURVE('',#9605,#9606,#5921,.T.);
#11816=EDGE_CURVE('',#9607,#9607,#5098,.T.);
#11817=EDGE_CURVE('',#9608,#9608,#5099,.T.);
#11818=EDGE_CURVE('',#9609,#9609,#5100,.T.);
#11819=EDGE_CURVE('',#9610,#9610,#5101,.T.);
#11820=EDGE_CURVE('',#9611,#9611,#5102,.T.);
#11821=EDGE_CURVE('',#9612,#9612,#5103,.T.);
#11822=EDGE_CURVE('',#9613,#9613,#5104,.T.);
#11823=EDGE_CURVE('',#9581,#9605,#5922,.T.);
#11824=EDGE_CURVE('',#9606,#9582,#5923,.T.);
#11825=EDGE_CURVE('',#9583,#9604,#5924,.T.);
#11826=EDGE_CURVE('',#9584,#9602,#5925,.T.);
#11827=EDGE_CURVE('',#9585,#9603,#5926,.T.);
#11828=EDGE_CURVE('',#9614,#9615,#5927,.T.);
#11829=EDGE_CURVE('',#9615,#9603,#5928,.T.);
#11830=EDGE_CURVE('',#9585,#9614,#5929,.T.);
#11831=EDGE_CURVE('',#9616,#9617,#5930,.T.);
#11832=EDGE_CURVE('',#9617,#9615,#5105,.T.);
#11833=EDGE_CURVE('',#9614,#9616,#5106,.T.);
#11834=EDGE_CURVE('',#9618,#9619,#5931,.T.);
#11835=EDGE_CURVE('',#9619,#9617,#5932,.T.);
#11836=EDGE_CURVE('',#9616,#9618,#5933,.T.);
#11837=EDGE_CURVE('',#9606,#9619,#5107,.T.);
#11838=EDGE_CURVE('',#9618,#9582,#5108,.T.);
#11839=EDGE_CURVE('',#9595,#9615,#5934,.T.);
#11840=EDGE_CURVE('',#9593,#9617,#5935,.T.);
#11841=EDGE_CURVE('',#9591,#9619,#5936,.T.);
#11842=EDGE_CURVE('',#9563,#9620,#5937,.T.);
#11843=EDGE_CURVE('',#9620,#9621,#5109,.T.);
#11844=EDGE_CURVE('',#9621,#9620,#5110,.T.);
#11845=EDGE_CURVE('',#9622,#9622,#5111,.T.);
#11846=EDGE_CURVE('',#9622,#9621,#5938,.T.);
#11847=EDGE_CURVE('',#9569,#9623,#5939,.T.);
#11848=EDGE_CURVE('',#9623,#9624,#5112,.T.);
#11849=EDGE_CURVE('',#9624,#9623,#5113,.T.);
#11850=EDGE_CURVE('',#9625,#9625,#5114,.T.);
#11851=EDGE_CURVE('',#9625,#9624,#5940,.T.);
#11852=EDGE_CURVE('',#9564,#9626,#5941,.T.);
#11853=EDGE_CURVE('',#9626,#9627,#5115,.T.);
#11854=EDGE_CURVE('',#9627,#9626,#5116,.T.);
#11855=EDGE_CURVE('',#9628,#9628,#5117,.T.);
#11856=EDGE_CURVE('',#9628,#9627,#5942,.T.);
#11857=EDGE_CURVE('',#9568,#9629,#5943,.T.);
#11858=EDGE_CURVE('',#9629,#9630,#5118,.T.);
#11859=EDGE_CURVE('',#9630,#9629,#5119,.T.);
#11860=EDGE_CURVE('',#9631,#9631,#5120,.T.);
#11861=EDGE_CURVE('',#9631,#9630,#5944,.T.);
#11862=EDGE_CURVE('',#9607,#9632,#5945,.T.);
#11863=EDGE_CURVE('',#9632,#9633,#5121,.T.);
#11864=EDGE_CURVE('',#9633,#9632,#5122,.T.);
#11865=EDGE_CURVE('',#9634,#9634,#5123,.T.);
#11866=EDGE_CURVE('',#9634,#9633,#5946,.T.);
#11867=EDGE_CURVE('',#9613,#9635,#5947,.T.);
#11868=EDGE_CURVE('',#9635,#9636,#5124,.T.);
#11869=EDGE_CURVE('',#9636,#9635,#5125,.T.);
#11870=EDGE_CURVE('',#9637,#9637,#5126,.T.);
#11871=EDGE_CURVE('',#9637,#9636,#5948,.T.);
#11872=EDGE_CURVE('',#9608,#9638,#5949,.T.);
#11873=EDGE_CURVE('',#9638,#9639,#5127,.T.);
#11874=EDGE_CURVE('',#9639,#9638,#5128,.T.);
#11875=EDGE_CURVE('',#9640,#9640,#5129,.T.);
#11876=EDGE_CURVE('',#9640,#9639,#5950,.T.);
#11877=EDGE_CURVE('',#9567,#9641,#5951,.T.);
#11878=EDGE_CURVE('',#9641,#9641,#5130,.T.);
#11879=EDGE_CURVE('',#9641,#9642,#5952,.T.);
#11880=EDGE_CURVE('',#9642,#9642,#5131,.T.);
#11881=EDGE_CURVE('',#9642,#9643,#5953,.T.);
#11882=EDGE_CURVE('',#9643,#9643,#5132,.T.);
#11883=EDGE_CURVE('',#9566,#9644,#5954,.T.);
#11884=EDGE_CURVE('',#9644,#9644,#5133,.T.);
#11885=EDGE_CURVE('',#9644,#9645,#5955,.T.);
#11886=EDGE_CURVE('',#9645,#9645,#5134,.T.);
#11887=EDGE_CURVE('',#9645,#9646,#5956,.T.);
#11888=EDGE_CURVE('',#9646,#9646,#5135,.T.);
#11889=EDGE_CURVE('',#9565,#9647,#5957,.T.);
#11890=EDGE_CURVE('',#9647,#9647,#5136,.T.);
#11891=EDGE_CURVE('',#9647,#9648,#5958,.T.);
#11892=EDGE_CURVE('',#9648,#9648,#5137,.T.);
#11893=EDGE_CURVE('',#9648,#9649,#5959,.T.);
#11894=EDGE_CURVE('',#9649,#9649,#5138,.T.);
#11895=EDGE_CURVE('',#9609,#9650,#5960,.T.);
#11896=EDGE_CURVE('',#9650,#9650,#5139,.T.);
#11897=EDGE_CURVE('',#9650,#9651,#5961,.T.);
#11898=EDGE_CURVE('',#9651,#9651,#5140,.T.);
#11899=EDGE_CURVE('',#9651,#9652,#5962,.T.);
#11900=EDGE_CURVE('',#9652,#9652,#5141,.T.);
#11901=EDGE_CURVE('',#9610,#9653,#5963,.T.);
#11902=EDGE_CURVE('',#9653,#9653,#5142,.T.);
#11903=EDGE_CURVE('',#9653,#9654,#5964,.T.);
#11904=EDGE_CURVE('',#9654,#9654,#5143,.T.);
#11905=EDGE_CURVE('',#9654,#9655,#5965,.T.);
#11906=EDGE_CURVE('',#9655,#9655,#5144,.T.);
#11907=EDGE_CURVE('',#9611,#9656,#5966,.T.);
#11908=EDGE_CURVE('',#9656,#9656,#5145,.T.);
#11909=EDGE_CURVE('',#9656,#9657,#5967,.T.);
#11910=EDGE_CURVE('',#9657,#9657,#5146,.T.);
#11911=EDGE_CURVE('',#9657,#9658,#5968,.T.);
#11912=EDGE_CURVE('',#9658,#9658,#5147,.T.);
#11913=EDGE_CURVE('',#9612,#9659,#5969,.T.);
#11914=EDGE_CURVE('',#9659,#9659,#5148,.T.);
#11915=EDGE_CURVE('',#9659,#9660,#5970,.T.);
#11916=EDGE_CURVE('',#9660,#9660,#5149,.T.);
#11917=EDGE_CURVE('',#9660,#9661,#5971,.T.);
#11918=EDGE_CURVE('',#9661,#9661,#5150,.T.);
#11919=EDGE_CURVE('',#9614,#9579,#5972,.T.);
#11920=EDGE_CURVE('',#9618,#9575,#5973,.T.);
#11921=EDGE_CURVE('',#9577,#9616,#5974,.T.);
#11922=EDGE_CURVE('',#9662,#9663,#5975,.T.);
#11923=EDGE_CURVE('',#9663,#9664,#5976,.T.);
#11924=EDGE_CURVE('',#9664,#9665,#5977,.T.);
#11925=EDGE_CURVE('',#9665,#9662,#5978,.T.);
#11926=EDGE_CURVE('',#9663,#9666,#5979,.T.);
#11927=EDGE_CURVE('',#9666,#9667,#5980,.T.);
#11928=EDGE_CURVE('',#9667,#9664,#5981,.T.);
#11929=EDGE_CURVE('',#9668,#9669,#5982,.T.);
#11930=EDGE_CURVE('',#9669,#9667,#5151,.T.);
#11931=EDGE_CURVE('',#9666,#9668,#5152,.T.);
#11932=EDGE_CURVE('',#9670,#9671,#5983,.T.);
#11933=EDGE_CURVE('',#9671,#9669,#5984,.T.);
#11934=EDGE_CURVE('',#9668,#9670,#5985,.T.);
#11935=EDGE_CURVE('',#9672,#9673,#5986,.T.);
#11936=EDGE_CURVE('',#9673,#9671,#5153,.T.);
#11937=EDGE_CURVE('',#9670,#9672,#5154,.T.);
#11938=EDGE_CURVE('',#9665,#9673,#5987,.T.);
#11939=EDGE_CURVE('',#9672,#9662,#5988,.T.);
#11940=EDGE_CURVE('',#9674,#9673,#5989,.T.);
#11941=EDGE_CURVE('',#9675,#9674,#5155,.T.);
#11942=EDGE_CURVE('',#9675,#9671,#5990,.T.);
#11943=EDGE_CURVE('',#9665,#9676,#5991,.T.);
#11944=EDGE_CURVE('',#9674,#9676,#5992,.T.);
#11945=EDGE_CURVE('',#9664,#9677,#5993,.T.);
#11946=EDGE_CURVE('',#9676,#9677,#5994,.T.);
#11947=EDGE_CURVE('',#9678,#9678,#5156,.T.);
#11948=EDGE_CURVE('',#9679,#9679,#5157,.T.);
#11949=EDGE_CURVE('',#9680,#9680,#5158,.T.);
#11950=EDGE_CURVE('',#9681,#9681,#5159,.T.);
#11951=EDGE_CURVE('',#9682,#9682,#5160,.T.);
#11952=EDGE_CURVE('',#9683,#9683,#5161,.T.);
#11953=EDGE_CURVE('',#9684,#9684,#5162,.T.);
#11954=EDGE_CURVE('',#9685,#9676,#5995,.T.);
#11955=EDGE_CURVE('',#9677,#9686,#5996,.T.);
#11956=EDGE_CURVE('',#9686,#9687,#5997,.T.);
#11957=EDGE_CURVE('',#9687,#9688,#5998,.T.);
#11958=EDGE_CURVE('',#9688,#9685,#5999,.T.);
#11959=EDGE_CURVE('',#9689,#9687,#6000,.T.);
#11960=EDGE_CURVE('',#9690,#9689,#6001,.T.);
#11961=EDGE_CURVE('',#9688,#9690,#6002,.T.);
#11962=EDGE_CURVE('',#9691,#9691,#5163,.T.);
#11963=EDGE_CURVE('',#9692,#9692,#5164,.T.);
#11964=EDGE_CURVE('',#9693,#9693,#5165,.T.);
#11965=EDGE_CURVE('',#9694,#9686,#6003,.T.);
#11966=EDGE_CURVE('',#9694,#9695,#6004,.T.);
#11967=EDGE_CURVE('',#9695,#9696,#6005,.T.);
#11968=EDGE_CURVE('',#9696,#9689,#6006,.T.);
#11969=EDGE_CURVE('',#9677,#9697,#6007,.T.);
#11970=EDGE_CURVE('',#9698,#9697,#6008,.T.);
#11971=EDGE_CURVE('',#9698,#9694,#6009,.T.);
#11972=EDGE_CURVE('',#9685,#9699,#6010,.T.);
#11973=EDGE_CURVE('',#9699,#9700,#6011,.T.);
#11974=EDGE_CURVE('',#9700,#9674,#6012,.T.);
#11975=EDGE_CURVE('',#9701,#9675,#6013,.T.);
#11976=EDGE_CURVE('',#9700,#9701,#5166,.T.);
#11977=EDGE_CURVE('',#9702,#9703,#6014,.T.);
#11978=EDGE_CURVE('',#9703,#9675,#6015,.T.);
#11979=EDGE_CURVE('',#9701,#9702,#6016,.T.);
#11980=EDGE_CURVE('',#9697,#9703,#5167,.T.);
#11981=EDGE_CURVE('',#9702,#9698,#5168,.T.);
#11982=EDGE_CURVE('',#9703,#9669,#6017,.T.);
#11983=EDGE_CURVE('',#9697,#9667,#6018,.T.);
#11984=EDGE_CURVE('',#9696,#9704,#6019,.T.);
#11985=EDGE_CURVE('',#9704,#9705,#6020,.T.);
#11986=EDGE_CURVE('',#9705,#9706,#6021,.T.);
#11987=EDGE_CURVE('',#9690,#9706,#6022,.T.);
#11988=EDGE_CURVE('',#9706,#9707,#6023,.T.);
#11989=EDGE_CURVE('',#9707,#9699,#6024,.T.);
#11990=EDGE_CURVE('',#9708,#9707,#6025,.T.);
#11991=EDGE_CURVE('',#9700,#9708,#6026,.T.);
#11992=EDGE_CURVE('',#9705,#9709,#6027,.T.);
#11993=EDGE_CURVE('',#9708,#9709,#6028,.T.);
#11994=EDGE_CURVE('',#9695,#9710,#6029,.T.);
#11995=EDGE_CURVE('',#9710,#9711,#6030,.T.);
#11996=EDGE_CURVE('',#9711,#9704,#6031,.T.);
#11997=EDGE_CURVE('',#9712,#9713,#6032,.T.);
#11998=EDGE_CURVE('',#9713,#9711,#5169,.T.);
#11999=EDGE_CURVE('',#9710,#9712,#5170,.T.);
#12000=EDGE_CURVE('',#9714,#9715,#6033,.T.);
#12001=EDGE_CURVE('',#9715,#9713,#6034,.T.);
#12002=EDGE_CURVE('',#9712,#9714,#6035,.T.);
#12003=EDGE_CURVE('',#9709,#9715,#5171,.T.);
#12004=EDGE_CURVE('',#9714,#9708,#5172,.T.);
#12005=EDGE_CURVE('',#9709,#9716,#6036,.T.);
#12006=EDGE_CURVE('',#9717,#9716,#5173,.T.);
#12007=EDGE_CURVE('',#9715,#9717,#6037,.T.);
#12008=EDGE_CURVE('',#9718,#9705,#6038,.T.);
#12009=EDGE_CURVE('',#9716,#9718,#6039,.T.);
#12010=EDGE_CURVE('',#9719,#9704,#6040,.T.);
#12011=EDGE_CURVE('',#9718,#9719,#6041,.T.);
#12012=EDGE_CURVE('',#9702,#9712,#6042,.T.);
#12013=EDGE_CURVE('',#9710,#9698,#6043,.T.);
#12014=EDGE_CURVE('',#9720,#9721,#6044,.T.);
#12015=EDGE_CURVE('',#9721,#9718,#6045,.T.);
#12016=EDGE_CURVE('',#9719,#9720,#6046,.T.);
#12017=EDGE_CURVE('',#9721,#9722,#6047,.T.);
#12018=EDGE_CURVE('',#9722,#9716,#6048,.T.);
#12019=EDGE_CURVE('',#9723,#9717,#6049,.T.);
#12020=EDGE_CURVE('',#9722,#9723,#5174,.T.);
#12021=EDGE_CURVE('',#9724,#9725,#6050,.T.);
#12022=EDGE_CURVE('',#9725,#9717,#6051,.T.);
#12023=EDGE_CURVE('',#9723,#9724,#6052,.T.);
#12024=EDGE_CURVE('',#9726,#9727,#6053,.T.);
#12025=EDGE_CURVE('',#9727,#9725,#5175,.T.);
#12026=EDGE_CURVE('',#9724,#9726,#5176,.T.);
#12027=EDGE_CURVE('',#9719,#9727,#6054,.T.);
#12028=EDGE_CURVE('',#9726,#9720,#6055,.T.);
#12029=EDGE_CURVE('',#9713,#9725,#6056,.T.);
#12030=EDGE_CURVE('',#9711,#9727,#6057,.T.);
#12031=EDGE_CURVE('',#9728,#9728,#5177,.T.);
#12032=EDGE_CURVE('',#9729,#9729,#5178,.T.);
#12033=EDGE_CURVE('',#9730,#9730,#5179,.T.);
#12034=EDGE_CURVE('',#9731,#9731,#5180,.T.);
#12035=EDGE_CURVE('',#9732,#9732,#5181,.T.);
#12036=EDGE_CURVE('',#9733,#9733,#5182,.T.);
#12037=EDGE_CURVE('',#9734,#9734,#5183,.T.);
#12038=EDGE_CURVE('',#9735,#9735,#5184,.T.);
#12039=EDGE_CURVE('',#9736,#9736,#5185,.T.);
#12040=EDGE_CURVE('',#9737,#9737,#5186,.T.);
#12041=EDGE_CURVE('',#9678,#9738,#6058,.T.);
#12042=EDGE_CURVE('',#9738,#9738,#5187,.T.);
#12043=EDGE_CURVE('',#9738,#9739,#6059,.T.);
#12044=EDGE_CURVE('',#9739,#9739,#5188,.T.);
#12045=EDGE_CURVE('',#9728,#9740,#6060,.T.);
#12046=EDGE_CURVE('',#9740,#9741,#5189,.T.);
#12047=EDGE_CURVE('',#9741,#9740,#5190,.T.);
#12048=EDGE_CURVE('',#9742,#9742,#5191,.T.);
#12049=EDGE_CURVE('',#9742,#9741,#6061,.T.);
#12050=EDGE_CURVE('',#9739,#9743,#6062,.T.);
#12051=EDGE_CURVE('',#9743,#9743,#5192,.T.);
#12052=EDGE_CURVE('',#9737,#9744,#6063,.T.);
#12053=EDGE_CURVE('',#9744,#9745,#5193,.T.);
#12054=EDGE_CURVE('',#9745,#9744,#5194,.T.);
#12055=EDGE_CURVE('',#9746,#9746,#5195,.T.);
#12056=EDGE_CURVE('',#9746,#9745,#6064,.T.);
#12057=EDGE_CURVE('',#9684,#9746,#6065,.T.);
#12058=EDGE_CURVE('',#9729,#9747,#6066,.T.);
#12059=EDGE_CURVE('',#9747,#9748,#5196,.T.);
#12060=EDGE_CURVE('',#9748,#9747,#5197,.T.);
#12061=EDGE_CURVE('',#9749,#9749,#5198,.T.);
#12062=EDGE_CURVE('',#9749,#9748,#6067,.T.);
#12063=EDGE_CURVE('',#9679,#9749,#6068,.T.);
#12064=EDGE_CURVE('',#9736,#9750,#6069,.T.);
#12065=EDGE_CURVE('',#9750,#9751,#5199,.T.);
#12066=EDGE_CURVE('',#9751,#9750,#5200,.T.);
#12067=EDGE_CURVE('',#9752,#9752,#5201,.T.);
#12068=EDGE_CURVE('',#9752,#9751,#6070,.T.);
#12069=EDGE_CURVE('',#9683,#9752,#6071,.T.);
#12070=EDGE_CURVE('',#9680,#9753,#6072,.T.);
#12071=EDGE_CURVE('',#9753,#9753,#5202,.T.);
#12072=EDGE_CURVE('',#9753,#9754,#6073,.T.);
#12073=EDGE_CURVE('',#9754,#9754,#5203,.T.);
#12074=EDGE_CURVE('',#9682,#9755,#6074,.T.);
#12075=EDGE_CURVE('',#9755,#9755,#5204,.T.);
#12076=EDGE_CURVE('',#9755,#9756,#6075,.T.);
#12077=EDGE_CURVE('',#9756,#9756,#5205,.T.);
#12078=EDGE_CURVE('',#9681,#9757,#6076,.T.);
#12079=EDGE_CURVE('',#9757,#9757,#5206,.T.);
#12080=EDGE_CURVE('',#9757,#9758,#6077,.T.);
#12081=EDGE_CURVE('',#9758,#9758,#5207,.T.);
#12082=EDGE_CURVE('',#9759,#9759,#5208,.T.);
#12083=EDGE_CURVE('',#9759,#9760,#6078,.T.);
#12084=EDGE_CURVE('',#9760,#9760,#5209,.T.);
#12085=EDGE_CURVE('',#9761,#9762,#5210,.T.);
#12086=EDGE_CURVE('',#9762,#9761,#5211,.T.);
#12087=EDGE_CURVE('',#9762,#9760,#6079,.T.);
#12088=EDGE_CURVE('',#9714,#9701,#6080,.T.);
#12089=EDGE_CURVE('',#9763,#9764,#5212,.T.);
#12090=EDGE_CURVE('',#9764,#9763,#5213,.T.);
#12091=EDGE_CURVE('',#9763,#9761,#6081,.T.);
#12092=EDGE_CURVE('',#9765,#9765,#5214,.T.);
#12093=EDGE_CURVE('',#9765,#9764,#6082,.T.);
#12094=EDGE_CURVE('',#9766,#9765,#6083,.T.);
#12095=EDGE_CURVE('',#9767,#9768,#6084,.T.);
#12096=EDGE_CURVE('',#9768,#9768,#5215,.T.);
#12097=EDGE_CURVE('',#9768,#9769,#6085,.T.);
#12098=EDGE_CURVE('',#9769,#9769,#5216,.T.);
#12099=EDGE_CURVE('',#9769,#9693,#6086,.T.);
#12100=EDGE_CURVE('',#9770,#9771,#6087,.T.);
#12101=EDGE_CURVE('',#9771,#9771,#5217,.T.);
#12102=EDGE_CURVE('',#9771,#9772,#6088,.T.);
#12103=EDGE_CURVE('',#9772,#9772,#5218,.T.);
#12104=EDGE_CURVE('',#9772,#9692,#6089,.T.);
#12105=EDGE_CURVE('',#9773,#9774,#6090,.T.);
#12106=EDGE_CURVE('',#9774,#9774,#5219,.T.);
#12107=EDGE_CURVE('',#9774,#9775,#6091,.T.);
#12108=EDGE_CURVE('',#9775,#9775,#5220,.T.);
#12109=EDGE_CURVE('',#9775,#9691,#6092,.T.);
#12110=EDGE_CURVE('',#9758,#9730,#6093,.T.);
#12111=EDGE_CURVE('',#9756,#9735,#6094,.T.);
#12112=EDGE_CURVE('',#9754,#9731,#6095,.T.);
#12113=EDGE_CURVE('',#9776,#9777,#6096,.T.);
#12114=EDGE_CURVE('',#9777,#9777,#5221,.T.);
#12115=EDGE_CURVE('',#9777,#9778,#6097,.T.);
#12116=EDGE_CURVE('',#9778,#9778,#5222,.T.);
#12117=EDGE_CURVE('',#9778,#9732,#6098,.T.);
#12118=EDGE_CURVE('',#9779,#9780,#6099,.T.);
#12119=EDGE_CURVE('',#9780,#9780,#5223,.T.);
#12120=EDGE_CURVE('',#9780,#9781,#6100,.T.);
#12121=EDGE_CURVE('',#9781,#9781,#5224,.T.);
#12122=EDGE_CURVE('',#9781,#9733,#6101,.T.);
#12123=EDGE_CURVE('',#9782,#9783,#6102,.T.);
#12124=EDGE_CURVE('',#9783,#9783,#5225,.T.);
#12125=EDGE_CURVE('',#9783,#9784,#6103,.T.);
#12126=EDGE_CURVE('',#9784,#9784,#5226,.T.);
#12127=EDGE_CURVE('',#9784,#9734,#6104,.T.);
#12128=EDGE_CURVE('',#9785,#9786,#6105,.T.);
#12129=EDGE_CURVE('',#9786,#9787,#5227,.T.);
#12130=EDGE_CURVE('',#9787,#9788,#6106,.T.);
#12131=EDGE_CURVE('',#9788,#9785,#5228,.T.);
#12132=EDGE_CURVE('',#9789,#9790,#6107,.T.);
#12133=EDGE_CURVE('',#9790,#9786,#6108,.T.);
#12134=EDGE_CURVE('',#9785,#9789,#6109,.T.);
#12135=EDGE_CURVE('',#9791,#9792,#6110,.T.);
#12136=EDGE_CURVE('',#9792,#9790,#5229,.T.);
#12137=EDGE_CURVE('',#9789,#9791,#5230,.T.);
#12138=EDGE_CURVE('',#9793,#9794,#6111,.T.);
#12139=EDGE_CURVE('',#9794,#9792,#6112,.T.);
#12140=EDGE_CURVE('',#9791,#9793,#6113,.T.);
#12141=EDGE_CURVE('',#9795,#9796,#6114,.T.);
#12142=EDGE_CURVE('',#9796,#9794,#5231,.T.);
#12143=EDGE_CURVE('',#9793,#9795,#5232,.T.);
#12144=EDGE_CURVE('',#9797,#9798,#6115,.T.);
#12145=EDGE_CURVE('',#9798,#9796,#6116,.T.);
#12146=EDGE_CURVE('',#9795,#9797,#6117,.T.);
#12147=EDGE_CURVE('',#9799,#9800,#6118,.T.);
#12148=EDGE_CURVE('',#9800,#9798,#5233,.T.);
#12149=EDGE_CURVE('',#9797,#9799,#5234,.T.);
#12150=EDGE_CURVE('',#9787,#9800,#6119,.T.);
#12151=EDGE_CURVE('',#9799,#9788,#6120,.T.);
#12152=EDGE_CURVE('',#9798,#9801,#6121,.T.);
#12153=EDGE_CURVE('',#9802,#9801,#6122,.T.);
#12154=EDGE_CURVE('',#9796,#9802,#6123,.T.);
#12155=EDGE_CURVE('',#9800,#9803,#6124,.T.);
#12156=EDGE_CURVE('',#9801,#9803,#5235,.T.);
#12157=EDGE_CURVE('',#9804,#9787,#6125,.T.);
#12158=EDGE_CURVE('',#9803,#9804,#6126,.T.);
#12159=EDGE_CURVE('',#9786,#9805,#6127,.T.);
#12160=EDGE_CURVE('',#9804,#9805,#5236,.T.);
#12161=EDGE_CURVE('',#9806,#9806,#5237,.T.);
#12162=EDGE_CURVE('',#9807,#9807,#5238,.T.);
#12163=EDGE_CURVE('',#9808,#9808,#5239,.T.);
#12164=EDGE_CURVE('',#9809,#9809,#5240,.T.);
#12165=EDGE_CURVE('',#9810,#9811,#6128,.T.);
#12166=EDGE_CURVE('',#9811,#9812,#6129,.T.);
#12167=EDGE_CURVE('',#9812,#9813,#6130,.T.);
#12168=EDGE_CURVE('',#9813,#9810,#6131,.T.);
#12169=EDGE_CURVE('',#9814,#9815,#6132,.T.);
#12170=EDGE_CURVE('',#9815,#9811,#5241,.T.);
#12171=EDGE_CURVE('',#9810,#9814,#5242,.T.);
#12172=EDGE_CURVE('',#9816,#9805,#6133,.T.);
#12173=EDGE_CURVE('',#9805,#9815,#6134,.T.);
#12174=EDGE_CURVE('',#9814,#9816,#6135,.T.);
#12175=EDGE_CURVE('',#9817,#9804,#6136,.T.);
#12176=EDGE_CURVE('',#9816,#9817,#5243,.T.);
#12177=EDGE_CURVE('',#9818,#9803,#6137,.T.);
#12178=EDGE_CURVE('',#9817,#9818,#6138,.T.);
#12179=EDGE_CURVE('',#9819,#9801,#6139,.T.);
#12180=EDGE_CURVE('',#9818,#9819,#5244,.T.);
#12181=EDGE_CURVE('',#9820,#9802,#6140,.T.);
#12182=EDGE_CURVE('',#9819,#9820,#6141,.T.);
#12183=EDGE_CURVE('',#9812,#9802,#5245,.T.);
#12184=EDGE_CURVE('',#9820,#9813,#5246,.T.);
#12185=EDGE_CURVE('',#9816,#9821,#6142,.T.);
#12186=EDGE_CURVE('',#9822,#9821,#5247,.T.);
#12187=EDGE_CURVE('',#9822,#9817,#6143,.T.);
#12188=EDGE_CURVE('',#9823,#9814,#6144,.T.);
#12189=EDGE_CURVE('',#9821,#9823,#6145,.T.);
#12190=EDGE_CURVE('',#9810,#9824,#6146,.T.);
#12191=EDGE_CURVE('',#9823,#9824,#5248,.T.);
#12192=EDGE_CURVE('',#9825,#9813,#6147,.T.);
#12193=EDGE_CURVE('',#9824,#9825,#6148,.T.);
#12194=EDGE_CURVE('',#9794,#9812,#6149,.T.);
#12195=EDGE_CURVE('',#9792,#9811,#6150,.T.);
#12196=EDGE_CURVE('',#9821,#9826,#6151,.T.);
#12197=EDGE_CURVE('',#9826,#9827,#5249,.T.);
#12198=EDGE_CURVE('',#9827,#9822,#6152,.T.);
#12199=EDGE_CURVE('',#9823,#9828,#6153,.T.);
#12200=EDGE_CURVE('',#9828,#9826,#6154,.T.);
#12201=EDGE_CURVE('',#9824,#9829,#6155,.T.);
#12202=EDGE_CURVE('',#9829,#9828,#5250,.T.);
#12203=EDGE_CURVE('',#9825,#9830,#6156,.T.);
#12204=EDGE_CURVE('',#9830,#9829,#6157,.T.);
#12205=EDGE_CURVE('',#9831,#9832,#6158,.T.);
#12206=EDGE_CURVE('',#9832,#9830,#5251,.T.);
#12207=EDGE_CURVE('',#9825,#9831,#5252,.T.);
#12208=EDGE_CURVE('',#9833,#9834,#6159,.T.);
#12209=EDGE_CURVE('',#9834,#9832,#6160,.T.);
#12210=EDGE_CURVE('',#9831,#9833,#6161,.T.);
#12211=EDGE_CURVE('',#9835,#9836,#6162,.T.);
#12212=EDGE_CURVE('',#9836,#9834,#5253,.T.);
#12213=EDGE_CURVE('',#9833,#9835,#5254,.T.);
#12214=EDGE_CURVE('',#9827,#9836,#6163,.T.);
#12215=EDGE_CURVE('',#9835,#9822,#6164,.T.);
#12216=EDGE_CURVE('',#9837,#9834,#6165,.T.);
#12217=EDGE_CURVE('',#9838,#9837,#6166,.T.);
#12218=EDGE_CURVE('',#9838,#9832,#6167,.T.);
#12219=EDGE_CURVE('',#9839,#9836,#6168,.T.);
#12220=EDGE_CURVE('',#9837,#9839,#5255,.T.);
#12221=EDGE_CURVE('',#9840,#9827,#6169,.T.);
#12222=EDGE_CURVE('',#9839,#9840,#6170,.T.);
#12223=EDGE_CURVE('',#9826,#9841,#6171,.T.);
#12224=EDGE_CURVE('',#9840,#9841,#5256,.T.);
#12225=EDGE_CURVE('',#9806,#9842,#6172,.T.);
#12226=EDGE_CURVE('',#9842,#9843,#5257,.T.);
#12227=EDGE_CURVE('',#9843,#9842,#5258,.T.);
#12228=EDGE_CURVE('',#9844,#9844,#5259,.T.);
#12229=EDGE_CURVE('',#9844,#9843,#6173,.T.);
#12230=EDGE_CURVE('',#9845,#9840,#6174,.T.);
#12231=EDGE_CURVE('',#9841,#9846,#6175,.T.);
#12232=EDGE_CURVE('',#9846,#9845,#5260,.T.);
#12233=EDGE_CURVE('',#9847,#9839,#6176,.T.);
#12234=EDGE_CURVE('',#9845,#9847,#6177,.T.);
#12235=EDGE_CURVE('',#9848,#9837,#6178,.T.);
#12236=EDGE_CURVE('',#9847,#9848,#5261,.T.);
#12237=EDGE_CURVE('',#9849,#9838,#6179,.T.);
#12238=EDGE_CURVE('',#9848,#9849,#6180,.T.);
#12239=EDGE_CURVE('',#9850,#9851,#6181,.T.);
#12240=EDGE_CURVE('',#9851,#9838,#5262,.T.);
#12241=EDGE_CURVE('',#9849,#9850,#5263,.T.);
#12242=EDGE_CURVE('',#9852,#9853,#6182,.T.);
#12243=EDGE_CURVE('',#9853,#9851,#6183,.T.);
#12244=EDGE_CURVE('',#9850,#9852,#6184,.T.);
#12245=EDGE_CURVE('',#9854,#9855,#6185,.T.);
#12246=EDGE_CURVE('',#9855,#9853,#5264,.T.);
#12247=EDGE_CURVE('',#9852,#9854,#5265,.T.);
#12248=EDGE_CURVE('',#9841,#9855,#6186,.T.);
#12249=EDGE_CURVE('',#9854,#9846,#6187,.T.);
#12250=EDGE_CURVE('',#9851,#9830,#6188,.T.);
#12251=EDGE_CURVE('',#9853,#9829,#6189,.T.);
#12252=EDGE_CURVE('',#9855,#9828,#6190,.T.);
#12253=EDGE_CURVE('',#9856,#9856,#5266,.T.);
#12254=EDGE_CURVE('',#9857,#9857,#5267,.T.);
#12255=EDGE_CURVE('',#9857,#9858,#6191,.T.);
#12256=EDGE_CURVE('',#9858,#9858,#5268,.T.);
#12257=EDGE_CURVE('',#9859,#9859,#5269,.T.);
#12258=EDGE_CURVE('',#9859,#9857,#6192,.T.);
#12259=EDGE_CURVE('',#9860,#9860,#5270,.T.);
#12260=EDGE_CURVE('',#9860,#9856,#6193,.T.);
#12261=EDGE_CURVE('',#9860,#9861,#6194,.T.);
#12262=EDGE_CURVE('',#9861,#9861,#5271,.T.);
#12263=EDGE_CURVE('',#9861,#9859,#6195,.T.);
#12264=EDGE_CURVE('',#9862,#9863,#6196,.T.);
#12265=EDGE_CURVE('',#9863,#9863,#5272,.T.);
#12266=EDGE_CURVE('',#9863,#9864,#6197,.T.);
#12267=EDGE_CURVE('',#9864,#9864,#5273,.T.);
#12268=EDGE_CURVE('',#9864,#9807,#6198,.T.);
#12269=EDGE_CURVE('',#9865,#9866,#6199,.T.);
#12270=EDGE_CURVE('',#9866,#9866,#5274,.T.);
#12271=EDGE_CURVE('',#9866,#9867,#6200,.T.);
#12272=EDGE_CURVE('',#9867,#9867,#5275,.T.);
#12273=EDGE_CURVE('',#9867,#9808,#6201,.T.);
#12274=EDGE_CURVE('',#9868,#9869,#6202,.T.);
#12275=EDGE_CURVE('',#9869,#9869,#5276,.T.);
#12276=EDGE_CURVE('',#9869,#9870,#6203,.T.);
#12277=EDGE_CURVE('',#9870,#9870,#5277,.T.);
#12278=EDGE_CURVE('',#9870,#9809,#6204,.T.);
#12279=EDGE_CURVE('',#9790,#9815,#6205,.T.);
#12280=EDGE_CURVE('',#9833,#9819,#6206,.T.);
#12281=EDGE_CURVE('',#9820,#9831,#6207,.T.);
#12282=EDGE_CURVE('',#9818,#9835,#6208,.T.);
#12283=EDGE_CURVE('',#9871,#9871,#5278,.T.);
#12284=EDGE_CURVE('',#9871,#9872,#6209,.T.);
#12285=EDGE_CURVE('',#9872,#9873,#5279,.T.);
#12286=EDGE_CURVE('',#9873,#9872,#5280,.T.);
#12287=EDGE_CURVE('',#9873,#9874,#6210,.T.);
#12288=EDGE_CURVE('',#9875,#9874,#5281,.T.);
#12289=EDGE_CURVE('',#9874,#9875,#5282,.T.);
#12290=EDGE_CURVE('',#9871,#9876,#6211,.T.);
#12291=EDGE_CURVE('',#9876,#9876,#5283,.T.);
#12292=EDGE_CURVE('',#9877,#9877,#5284,.T.);
#12293=EDGE_CURVE('',#9877,#9875,#6212,.T.);
#12294=EDGE_CURVE('',#9878,#9878,#5285,.T.);
#12295=EDGE_CURVE('',#9878,#9877,#6213,.T.);
#12296=EDGE_CURVE('',#9878,#9879,#6214,.T.);
#12297=EDGE_CURVE('',#9879,#9879,#5286,.T.);
#12298=EDGE_CURVE('',#9880,#9880,#5287,.T.);
#12299=EDGE_CURVE('',#9881,#9881,#5288,.T.);
#12300=EDGE_CURVE('',#9882,#9882,#5289,.T.);
#12301=EDGE_CURVE('',#9883,#9883,#5290,.T.);
#12302=EDGE_CURVE('',#9884,#9884,#5291,.T.);
#12303=EDGE_CURVE('',#9884,#9880,#6215,.T.);
#12304=EDGE_CURVE('',#9885,#9885,#5292,.T.);
#12305=EDGE_CURVE('',#9885,#9884,#6216,.T.);
#12306=EDGE_CURVE('',#9876,#9886,#6217,.T.);
#12307=EDGE_CURVE('',#9886,#9886,#5293,.T.);
#12308=EDGE_CURVE('',#9887,#9887,#5294,.T.);
#12309=EDGE_CURVE('',#9885,#9888,#6218,.T.);
#12310=EDGE_CURVE('',#9888,#9889,#5295,.T.);
#12311=EDGE_CURVE('',#9889,#9888,#5296,.T.);
#12312=EDGE_CURVE('',#9890,#9891,#5297,.T.);
#12313=EDGE_CURVE('',#9891,#9890,#5298,.T.);
#12314=EDGE_CURVE('',#9891,#9889,#6219,.T.);
#12315=EDGE_CURVE('',#9892,#9892,#5299,.T.);
#12316=EDGE_CURVE('',#9892,#9887,#6220,.T.);
#12317=EDGE_CURVE('',#9892,#9893,#6221,.T.);
#12318=EDGE_CURVE('',#9893,#9893,#5300,.T.);
#12319=EDGE_CURVE('',#9893,#9890,#6222,.T.);
#12320=EDGE_CURVE('',#9894,#9895,#6223,.T.);
#12321=EDGE_CURVE('',#9895,#9895,#5301,.T.);
#12322=EDGE_CURVE('',#9895,#9896,#6224,.T.);
#12323=EDGE_CURVE('',#9896,#9896,#5302,.T.);
#12324=EDGE_CURVE('',#9896,#9881,#6225,.T.);
#12325=EDGE_CURVE('',#9897,#9898,#6226,.T.);
#12326=EDGE_CURVE('',#9898,#9898,#5303,.T.);
#12327=EDGE_CURVE('',#9898,#9899,#6227,.T.);
#12328=EDGE_CURVE('',#9899,#9899,#5304,.T.);
#12329=EDGE_CURVE('',#9899,#9882,#6228,.T.);
#12330=EDGE_CURVE('',#9900,#9901,#6229,.T.);
#12331=EDGE_CURVE('',#9901,#9901,#5305,.T.);
#12332=EDGE_CURVE('',#9901,#9902,#6230,.T.);
#12333=EDGE_CURVE('',#9902,#9902,#5306,.T.);
#12334=EDGE_CURVE('',#9902,#9883,#6231,.T.);
#12335=EDGE_CURVE('',#9903,#9903,#5307,.T.);
#12336=EDGE_CURVE('',#9903,#9904,#6232,.T.);
#12337=EDGE_CURVE('',#9904,#9905,#5308,.T.);
#12338=EDGE_CURVE('',#9905,#9904,#5309,.T.);
#12339=EDGE_CURVE('',#9906,#9906,#5310,.T.);
#12340=EDGE_CURVE('',#9906,#9905,#6233,.T.);
#12341=EDGE_CURVE('',#9907,#9907,#5311,.T.);
#12342=EDGE_CURVE('',#9908,#9908,#5312,.T.);
#12343=EDGE_CURVE('',#9909,#9909,#5313,.T.);
#12344=EDGE_CURVE('',#9910,#9910,#5314,.T.);
#12345=EDGE_CURVE('',#9911,#9911,#5315,.T.);
#12346=EDGE_CURVE('',#9912,#9912,#5316,.T.);
#12347=EDGE_CURVE('',#9913,#9913,#5317,.T.);
#12348=EDGE_CURVE('',#9914,#9914,#5318,.T.);
#12349=EDGE_CURVE('',#9914,#9906,#6234,.T.);
#12350=EDGE_CURVE('',#9915,#9915,#5319,.T.);
#12351=EDGE_CURVE('',#9916,#9916,#5320,.T.);
#12352=EDGE_CURVE('',#9917,#9917,#5321,.T.);
#12353=EDGE_CURVE('',#9918,#9918,#5322,.T.);
#12354=EDGE_CURVE('',#9919,#9919,#5323,.T.);
#12355=EDGE_CURVE('',#9920,#9920,#5324,.T.);
#12356=EDGE_CURVE('',#9921,#9921,#5325,.T.);
#12357=EDGE_CURVE('',#9908,#9922,#6235,.T.);
#12358=EDGE_CURVE('',#9922,#9923,#5326,.T.);
#12359=EDGE_CURVE('',#9923,#9922,#5327,.T.);
#12360=EDGE_CURVE('',#9924,#9924,#5328,.T.);
#12361=EDGE_CURVE('',#9924,#9923,#6236,.T.);
#12362=EDGE_CURVE('',#9916,#9924,#6237,.T.);
#12363=EDGE_CURVE('',#9913,#9925,#6238,.T.);
#12364=EDGE_CURVE('',#9925,#9926,#5329,.T.);
#12365=EDGE_CURVE('',#9926,#9925,#5330,.T.);
#12366=EDGE_CURVE('',#9927,#9927,#5331,.T.);
#12367=EDGE_CURVE('',#9927,#9926,#6239,.T.);
#12368=EDGE_CURVE('',#9921,#9927,#6240,.T.);
#12369=EDGE_CURVE('',#9909,#9928,#6241,.T.);
#12370=EDGE_CURVE('',#9928,#9929,#5332,.T.);
#12371=EDGE_CURVE('',#9929,#9928,#5333,.T.);
#12372=EDGE_CURVE('',#9930,#9930,#5334,.T.);
#12373=EDGE_CURVE('',#9930,#9929,#6242,.T.);
#12374=EDGE_CURVE('',#9917,#9930,#6243,.T.);
#12375=EDGE_CURVE('',#9912,#9931,#6244,.T.);
#12376=EDGE_CURVE('',#9931,#9932,#5335,.T.);
#12377=EDGE_CURVE('',#9932,#9931,#5336,.T.);
#12378=EDGE_CURVE('',#9933,#9933,#5337,.T.);
#12379=EDGE_CURVE('',#9933,#9932,#6245,.T.);
#12380=EDGE_CURVE('',#9920,#9933,#6246,.T.);
#12381=EDGE_CURVE('',#9910,#9934,#6247,.T.);
#12382=EDGE_CURVE('',#9934,#9935,#5338,.T.);
#12383=EDGE_CURVE('',#9935,#9934,#5339,.T.);
#12384=EDGE_CURVE('',#9936,#9936,#5340,.T.);
#12385=EDGE_CURVE('',#9936,#9935,#6248,.T.);
#12386=EDGE_CURVE('',#9918,#9936,#6249,.T.);
#12387=EDGE_CURVE('',#9907,#9937,#6250,.T.);
#12388=EDGE_CURVE('',#9937,#9938,#5341,.T.);
#12389=EDGE_CURVE('',#9938,#9937,#5342,.T.);
#12390=EDGE_CURVE('',#9938,#9939,#6251,.T.);
#12391=EDGE_CURVE('',#9940,#9939,#5343,.T.);
#12392=EDGE_CURVE('',#9939,#9940,#5344,.T.);
#12393=EDGE_CURVE('',#9940,#9915,#6252,.T.);
#12394=EDGE_CURVE('',#9919,#9941,#6253,.T.);
#12395=EDGE_CURVE('',#9941,#9942,#5345,.T.);
#12396=EDGE_CURVE('',#9942,#9941,#5346,.T.);
#12397=EDGE_CURVE('',#9943,#9944,#5347,.T.);
#12398=EDGE_CURVE('',#9944,#9943,#5348,.T.);
#12399=EDGE_CURVE('',#9944,#9942,#6254,.T.);
#12400=EDGE_CURVE('',#9943,#9911,#6255,.T.);
#12401=EDGE_CURVE('',#9945,#9946,#6256,.T.);
#12402=EDGE_CURVE('',#9945,#9947,#373,.T.);
#12403=EDGE_CURVE('',#9947,#9948,#6257,.T.);
#12404=EDGE_CURVE('',#9948,#9948,#5349,.T.);
#12405=EDGE_CURVE('',#9947,#9949,#374,.T.);
#12406=EDGE_CURVE('',#9949,#9950,#5350,.T.);
#12407=EDGE_CURVE('',#9950,#9946,#375,.T.);
#12408=EDGE_CURVE('',#9951,#9952,#6258,.T.);
#12409=EDGE_CURVE('',#9951,#9945,#376,.T.);
#12410=EDGE_CURVE('',#9946,#9952,#377,.T.);
#12411=EDGE_CURVE('',#9953,#9954,#6259,.T.);
#12412=EDGE_CURVE('',#9953,#9951,#378,.T.);
#12413=EDGE_CURVE('',#9952,#9954,#379,.T.);
#12414=EDGE_CURVE('',#9955,#9956,#6260,.T.);
#12415=EDGE_CURVE('',#9955,#9953,#380,.T.);
#12416=EDGE_CURVE('',#9954,#9956,#381,.T.);
#12417=EDGE_CURVE('',#9957,#9958,#6261,.T.);
#12418=EDGE_CURVE('',#9957,#9955,#382,.T.);
#12419=EDGE_CURVE('',#9956,#9958,#383,.T.);
#12420=EDGE_CURVE('',#9959,#9960,#6262,.T.);
#12421=EDGE_CURVE('',#9959,#9957,#384,.T.);
#12422=EDGE_CURVE('',#9958,#9960,#385,.T.);
#12423=EDGE_CURVE('',#9961,#9962,#6263,.T.);
#12424=EDGE_CURVE('',#9961,#9959,#386,.T.);
#12425=EDGE_CURVE('',#9960,#9962,#387,.T.);
#12426=EDGE_CURVE('',#9963,#9964,#6264,.T.);
#12427=EDGE_CURVE('',#9963,#9961,#388,.T.);
#12428=EDGE_CURVE('',#9962,#9964,#389,.T.);
#12429=EDGE_CURVE('',#9965,#9966,#6265,.T.);
#12430=EDGE_CURVE('',#9965,#9963,#390,.T.);
#12431=EDGE_CURVE('',#9964,#9966,#391,.T.);
#12432=EDGE_CURVE('',#9967,#9968,#6266,.T.);
#12433=EDGE_CURVE('',#9967,#9965,#392,.T.);
#12434=EDGE_CURVE('',#9966,#9968,#393,.T.);
#12435=EDGE_CURVE('',#9969,#9970,#6267,.T.);
#12436=EDGE_CURVE('',#9969,#9971,#394,.T.);
#12437=EDGE_CURVE('',#9972,#9971,#5351,.T.);
#12438=EDGE_CURVE('',#9970,#9972,#395,.T.);
#12439=EDGE_CURVE('',#9973,#9974,#6268,.T.);
#12440=EDGE_CURVE('',#9973,#9969,#396,.T.);
#12441=EDGE_CURVE('',#9974,#9970,#397,.T.);
#12442=EDGE_CURVE('',#9975,#9976,#6269,.T.);
#12443=EDGE_CURVE('',#9975,#9973,#398,.T.);
#12444=EDGE_CURVE('',#9976,#9974,#399,.T.);
#12445=EDGE_CURVE('',#9977,#9978,#6270,.T.);
#12446=EDGE_CURVE('',#9977,#9975,#400,.T.);
#12447=EDGE_CURVE('',#9978,#9976,#401,.T.);
#12448=EDGE_CURVE('',#9979,#9980,#6271,.T.);
#12449=EDGE_CURVE('',#9979,#9977,#402,.T.);
#12450=EDGE_CURVE('',#9980,#9978,#403,.T.);
#12451=EDGE_CURVE('',#9981,#9982,#6272,.T.);
#12452=EDGE_CURVE('',#9981,#9979,#404,.T.);
#12453=EDGE_CURVE('',#9982,#9980,#405,.T.);
#12454=EDGE_CURVE('',#9983,#9984,#6273,.T.);
#12455=EDGE_CURVE('',#9983,#9981,#406,.T.);
#12456=EDGE_CURVE('',#9984,#9982,#407,.T.);
#12457=EDGE_CURVE('',#9985,#9986,#6274,.T.);
#12458=EDGE_CURVE('',#9985,#9983,#408,.T.);
#12459=EDGE_CURVE('',#9986,#9984,#409,.T.);
#12460=EDGE_CURVE('',#9987,#9988,#6275,.T.);
#12461=EDGE_CURVE('',#9987,#9985,#410,.T.);
#12462=EDGE_CURVE('',#9988,#9986,#411,.T.);
#12463=EDGE_CURVE('',#9989,#9990,#6276,.T.);
#12464=EDGE_CURVE('',#9989,#9987,#412,.T.);
#12465=EDGE_CURVE('',#9990,#9988,#413,.T.);
#12466=EDGE_CURVE('',#9991,#9992,#6277,.T.);
#12467=EDGE_CURVE('',#9991,#9989,#414,.T.);
#12468=EDGE_CURVE('',#9992,#9990,#415,.T.);
#12469=EDGE_CURVE('',#9993,#9972,#416,.T.);
#12470=EDGE_CURVE('',#9968,#9993,#417,.T.);
#12471=EDGE_CURVE('',#9994,#9950,#418,.T.);
#12472=EDGE_CURVE('',#9994,#9992,#419,.T.);
#12473=EDGE_CURVE('',#9949,#9995,#420,.T.);
#12474=EDGE_CURVE('',#9995,#9994,#5352,.T.);
#12475=EDGE_CURVE('',#9995,#9991,#421,.T.);
#12476=EDGE_CURVE('',#9971,#9996,#422,.T.);
#12477=EDGE_CURVE('',#9996,#9967,#423,.T.);
#12478=EDGE_CURVE('',#9997,#9997,#5353,.T.);
#12479=EDGE_CURVE('',#9997,#9998,#6278,.T.);
#12480=EDGE_CURVE('',#9998,#9998,#5354,.T.);
#12481=EDGE_CURVE('',#9999,#9999,#5355,.T.);
#12482=EDGE_CURVE('',#9999,#10000,#6279,.T.);
#12483=EDGE_CURVE('',#10000,#10000,#5356,.T.);
#12484=EDGE_CURVE('',#10001,#10001,#5357,.T.);
#12485=EDGE_CURVE('',#10001,#10002,#6280,.T.);
#12486=EDGE_CURVE('',#10002,#10002,#5358,.T.);
#12487=EDGE_CURVE('',#10003,#10003,#5359,.T.);
#12488=EDGE_CURVE('',#10003,#10004,#6281,.T.);
#12489=EDGE_CURVE('',#10004,#10004,#5360,.T.);
#12490=EDGE_CURVE('',#10005,#10006,#6282,.T.);
#12491=EDGE_CURVE('',#10007,#10005,#6283,.T.);
#12492=EDGE_CURVE('',#10007,#10008,#6284,.T.);
#12493=EDGE_CURVE('',#10008,#10006,#6285,.T.);
#12494=EDGE_CURVE('',#10006,#10009,#5361,.T.);
#12495=EDGE_CURVE('',#10009,#10008,#6286,.T.);
#12496=EDGE_CURVE('',#10009,#10010,#6287,.T.);
#12497=EDGE_CURVE('',#10010,#10007,#6288,.T.);
#12498=EDGE_CURVE('',#10010,#10005,#5362,.T.);
#12499=EDGE_CURVE('',#10011,#10012,#6289,.T.);
#12500=EDGE_CURVE('',#10013,#10011,#6290,.T.);
#12501=EDGE_CURVE('',#10013,#10014,#6291,.T.);
#12502=EDGE_CURVE('',#10014,#10012,#6292,.T.);
#12503=EDGE_CURVE('',#10012,#10015,#5363,.T.);
#12504=EDGE_CURVE('',#10015,#10014,#6293,.T.);
#12505=EDGE_CURVE('',#10015,#10016,#6294,.T.);
#12506=EDGE_CURVE('',#10016,#10013,#6295,.T.);
#12507=EDGE_CURVE('',#10016,#10011,#5364,.T.);
#12508=EDGE_CURVE('',#10017,#10018,#6296,.T.);
#12509=EDGE_CURVE('',#10019,#10017,#6297,.T.);
#12510=EDGE_CURVE('',#10019,#10020,#6298,.T.);
#12511=EDGE_CURVE('',#10020,#10018,#6299,.T.);
#12512=EDGE_CURVE('',#10018,#10021,#5365,.T.);
#12513=EDGE_CURVE('',#10021,#10020,#6300,.T.);
#12514=EDGE_CURVE('',#10021,#10022,#6301,.T.);
#12515=EDGE_CURVE('',#10022,#10019,#6302,.T.);
#12516=EDGE_CURVE('',#10022,#10017,#5366,.T.);
#12517=EDGE_CURVE('',#10023,#10024,#6303,.T.);
#12518=EDGE_CURVE('',#10025,#10023,#6304,.T.);
#12519=EDGE_CURVE('',#10025,#10026,#6305,.T.);
#12520=EDGE_CURVE('',#10026,#10024,#6306,.T.);
#12521=EDGE_CURVE('',#10024,#10027,#5367,.T.);
#12522=EDGE_CURVE('',#10027,#10026,#6307,.T.);
#12523=EDGE_CURVE('',#10027,#10028,#6308,.T.);
#12524=EDGE_CURVE('',#10028,#10025,#6309,.T.);
#12525=EDGE_CURVE('',#10028,#10023,#5368,.T.);
#12526=EDGE_CURVE('',#10029,#10030,#6310,.T.);
#12527=EDGE_CURVE('',#10031,#10029,#6311,.T.);
#12528=EDGE_CURVE('',#10031,#10032,#6312,.T.);
#12529=EDGE_CURVE('',#10032,#10030,#6313,.T.);
#12530=EDGE_CURVE('',#10030,#10033,#5369,.T.);
#12531=EDGE_CURVE('',#10033,#10032,#6314,.T.);
#12532=EDGE_CURVE('',#10033,#10034,#6315,.T.);
#12533=EDGE_CURVE('',#10034,#10031,#6316,.T.);
#12534=EDGE_CURVE('',#10034,#10029,#5370,.T.);
#12535=EDGE_CURVE('',#10035,#10036,#6317,.T.);
#12536=EDGE_CURVE('',#10037,#10035,#6318,.T.);
#12537=EDGE_CURVE('',#10037,#10038,#6319,.T.);
#12538=EDGE_CURVE('',#10038,#10036,#6320,.T.);
#12539=EDGE_CURVE('',#10036,#10039,#5371,.T.);
#12540=EDGE_CURVE('',#10039,#10038,#6321,.T.);
#12541=EDGE_CURVE('',#10039,#10040,#6322,.T.);
#12542=EDGE_CURVE('',#10040,#10037,#6323,.T.);
#12543=EDGE_CURVE('',#10040,#10035,#5372,.T.);
#12544=EDGE_CURVE('',#10041,#10042,#6324,.T.);
#12545=EDGE_CURVE('',#10043,#10041,#6325,.T.);
#12546=EDGE_CURVE('',#10043,#10044,#6326,.T.);
#12547=EDGE_CURVE('',#10044,#10042,#6327,.T.);
#12548=EDGE_CURVE('',#10042,#10045,#5373,.T.);
#12549=EDGE_CURVE('',#10045,#10044,#6328,.T.);
#12550=EDGE_CURVE('',#10045,#10046,#6329,.T.);
#12551=EDGE_CURVE('',#10046,#10043,#6330,.T.);
#12552=EDGE_CURVE('',#10046,#10041,#5374,.T.);
#12553=EDGE_CURVE('',#10047,#10048,#6331,.T.);
#12554=EDGE_CURVE('',#10049,#10047,#6332,.T.);
#12555=EDGE_CURVE('',#10049,#10050,#6333,.T.);
#12556=EDGE_CURVE('',#10050,#10048,#6334,.T.);
#12557=EDGE_CURVE('',#10048,#10051,#5375,.T.);
#12558=EDGE_CURVE('',#10051,#10050,#6335,.T.);
#12559=EDGE_CURVE('',#10051,#10052,#6336,.T.);
#12560=EDGE_CURVE('',#10052,#10049,#6337,.T.);
#12561=EDGE_CURVE('',#10052,#10047,#5376,.T.);
#12562=EDGE_CURVE('',#10053,#10054,#6338,.T.);
#12563=EDGE_CURVE('',#10055,#10053,#6339,.T.);
#12564=EDGE_CURVE('',#10055,#10056,#6340,.T.);
#12565=EDGE_CURVE('',#10056,#10054,#6341,.T.);
#12566=EDGE_CURVE('',#10054,#10057,#5377,.T.);
#12567=EDGE_CURVE('',#10057,#10056,#6342,.T.);
#12568=EDGE_CURVE('',#10057,#10058,#6343,.T.);
#12569=EDGE_CURVE('',#10058,#10055,#6344,.T.);
#12570=EDGE_CURVE('',#10058,#10053,#5378,.T.);
#12571=EDGE_CURVE('',#10059,#10060,#6345,.T.);
#12572=EDGE_CURVE('',#10061,#10059,#6346,.T.);
#12573=EDGE_CURVE('',#10061,#10062,#6347,.T.);
#12574=EDGE_CURVE('',#10062,#10060,#6348,.T.);
#12575=EDGE_CURVE('',#10060,#10063,#5379,.T.);
#12576=EDGE_CURVE('',#10063,#10062,#6349,.T.);
#12577=EDGE_CURVE('',#10063,#10064,#6350,.T.);
#12578=EDGE_CURVE('',#10064,#10061,#6351,.T.);
#12579=EDGE_CURVE('',#10064,#10059,#5380,.T.);
#12580=EDGE_CURVE('',#10065,#10066,#6352,.T.);
#12581=EDGE_CURVE('',#10067,#10065,#6353,.T.);
#12582=EDGE_CURVE('',#10067,#10068,#6354,.T.);
#12583=EDGE_CURVE('',#10068,#10066,#6355,.T.);
#12584=EDGE_CURVE('',#10066,#10069,#5381,.T.);
#12585=EDGE_CURVE('',#10069,#10068,#6356,.T.);
#12586=EDGE_CURVE('',#10069,#10070,#6357,.T.);
#12587=EDGE_CURVE('',#10070,#10067,#6358,.T.);
#12588=EDGE_CURVE('',#10070,#10065,#5382,.T.);
#12589=EDGE_CURVE('',#10071,#10072,#6359,.T.);
#12590=EDGE_CURVE('',#10073,#10071,#6360,.T.);
#12591=EDGE_CURVE('',#10073,#10074,#6361,.T.);
#12592=EDGE_CURVE('',#10074,#10072,#6362,.T.);
#12593=EDGE_CURVE('',#10072,#10075,#5383,.T.);
#12594=EDGE_CURVE('',#10076,#10074,#6363,.T.);
#12595=EDGE_CURVE('',#10075,#10076,#5384,.T.);
#12596=EDGE_CURVE('',#10076,#10077,#6364,.T.);
#12597=EDGE_CURVE('',#10077,#10073,#6365,.T.);
#12598=EDGE_CURVE('',#10077,#10078,#5385,.T.);
#12599=EDGE_CURVE('',#10078,#10071,#5386,.T.);
#12600=EDGE_CURVE('',#10079,#10080,#6366,.T.);
#12601=EDGE_CURVE('',#10081,#10079,#6367,.T.);
#12602=EDGE_CURVE('',#10081,#10082,#6368,.T.);
#12603=EDGE_CURVE('',#10082,#10080,#6369,.T.);
#12604=EDGE_CURVE('',#10080,#10083,#5387,.T.);
#12605=EDGE_CURVE('',#10083,#10082,#6370,.T.);
#12606=EDGE_CURVE('',#10083,#10084,#6371,.T.);
#12607=EDGE_CURVE('',#10084,#10081,#6372,.T.);
#12608=EDGE_CURVE('',#10084,#10079,#5388,.T.);
#12609=EDGE_CURVE('',#10085,#10086,#6373,.T.);
#12610=EDGE_CURVE('',#10087,#10085,#6374,.T.);
#12611=EDGE_CURVE('',#10087,#10088,#6375,.T.);
#12612=EDGE_CURVE('',#10088,#10086,#6376,.T.);
#12613=EDGE_CURVE('',#10086,#10089,#5389,.T.);
#12614=EDGE_CURVE('',#10089,#10088,#6377,.T.);
#12615=EDGE_CURVE('',#10089,#10090,#6378,.T.);
#12616=EDGE_CURVE('',#10090,#10087,#6379,.T.);
#12617=EDGE_CURVE('',#10090,#10085,#5390,.T.);
#12618=EDGE_CURVE('',#10091,#10092,#6380,.T.);
#12619=EDGE_CURVE('',#10093,#10091,#6381,.T.);
#12620=EDGE_CURVE('',#10093,#10094,#6382,.T.);
#12621=EDGE_CURVE('',#10094,#10092,#6383,.T.);
#12622=EDGE_CURVE('',#10092,#10095,#5391,.T.);
#12623=EDGE_CURVE('',#10095,#10094,#6384,.T.);
#12624=EDGE_CURVE('',#10095,#10096,#6385,.T.);
#12625=EDGE_CURVE('',#10096,#10093,#6386,.T.);
#12626=EDGE_CURVE('',#10096,#10091,#5392,.T.);
#12627=EDGE_CURVE('',#10097,#10098,#6387,.T.);
#12628=EDGE_CURVE('',#10099,#10097,#6388,.T.);
#12629=EDGE_CURVE('',#10099,#10100,#6389,.T.);
#12630=EDGE_CURVE('',#10100,#10098,#6390,.T.);
#12631=EDGE_CURVE('',#10098,#10101,#5393,.T.);
#12632=EDGE_CURVE('',#10101,#10100,#6391,.T.);
#12633=EDGE_CURVE('',#10101,#10102,#6392,.T.);
#12634=EDGE_CURVE('',#10102,#10099,#6393,.T.);
#12635=EDGE_CURVE('',#10102,#10097,#5394,.T.);
#12636=EDGE_CURVE('',#10103,#10104,#6394,.T.);
#12637=EDGE_CURVE('',#10105,#10103,#6395,.T.);
#12638=EDGE_CURVE('',#10105,#10106,#6396,.T.);
#12639=EDGE_CURVE('',#10106,#10104,#6397,.T.);
#12640=EDGE_CURVE('',#10104,#10107,#5395,.T.);
#12641=EDGE_CURVE('',#10107,#10106,#6398,.T.);
#12642=EDGE_CURVE('',#10107,#10108,#6399,.T.);
#12643=EDGE_CURVE('',#10108,#10105,#6400,.T.);
#12644=EDGE_CURVE('',#10108,#10103,#5396,.T.);
#12645=EDGE_CURVE('',#10109,#10110,#6401,.T.);
#12646=EDGE_CURVE('',#10111,#10109,#6402,.T.);
#12647=EDGE_CURVE('',#10111,#10112,#6403,.T.);
#12648=EDGE_CURVE('',#10112,#10110,#6404,.T.);
#12649=EDGE_CURVE('',#10110,#10113,#5397,.T.);
#12650=EDGE_CURVE('',#10113,#10112,#6405,.T.);
#12651=EDGE_CURVE('',#10113,#10114,#6406,.T.);
#12652=EDGE_CURVE('',#10114,#10111,#6407,.T.);
#12653=EDGE_CURVE('',#10114,#10109,#5398,.T.);
#12654=EDGE_CURVE('',#10115,#10116,#6408,.T.);
#12655=EDGE_CURVE('',#10117,#10115,#6409,.T.);
#12656=EDGE_CURVE('',#10117,#10118,#6410,.T.);
#12657=EDGE_CURVE('',#10118,#10116,#6411,.T.);
#12658=EDGE_CURVE('',#10116,#10119,#5399,.T.);
#12659=EDGE_CURVE('',#10119,#10118,#6412,.T.);
#12660=EDGE_CURVE('',#10119,#10120,#6413,.T.);
#12661=EDGE_CURVE('',#10120,#10117,#6414,.T.);
#12662=EDGE_CURVE('',#10120,#10115,#5400,.T.);
#12663=EDGE_CURVE('',#10121,#10122,#6415,.T.);
#12664=EDGE_CURVE('',#10123,#10121,#6416,.T.);
#12665=EDGE_CURVE('',#10123,#10124,#6417,.T.);
#12666=EDGE_CURVE('',#10124,#10122,#6418,.T.);
#12667=EDGE_CURVE('',#10122,#10125,#5401,.T.);
#12668=EDGE_CURVE('',#10125,#10124,#6419,.T.);
#12669=EDGE_CURVE('',#10125,#10126,#6420,.T.);
#12670=EDGE_CURVE('',#10126,#10123,#6421,.T.);
#12671=EDGE_CURVE('',#10126,#10121,#5402,.T.);
#12672=EDGE_CURVE('',#10127,#10128,#6422,.T.);
#12673=EDGE_CURVE('',#10129,#10127,#6423,.T.);
#12674=EDGE_CURVE('',#10129,#10130,#6424,.T.);
#12675=EDGE_CURVE('',#10130,#10128,#6425,.T.);
#12676=EDGE_CURVE('',#10128,#10131,#5403,.T.);
#12677=EDGE_CURVE('',#10131,#10130,#6426,.T.);
#12678=EDGE_CURVE('',#10131,#10132,#6427,.T.);
#12679=EDGE_CURVE('',#10132,#10129,#6428,.T.);
#12680=EDGE_CURVE('',#10132,#10127,#5404,.T.);
#12681=EDGE_CURVE('',#10133,#10134,#6429,.T.);
#12682=EDGE_CURVE('',#10135,#10133,#6430,.T.);
#12683=EDGE_CURVE('',#10135,#10136,#6431,.T.);
#12684=EDGE_CURVE('',#10136,#10134,#6432,.T.);
#12685=EDGE_CURVE('',#10134,#10137,#5405,.T.);
#12686=EDGE_CURVE('',#10137,#10136,#6433,.T.);
#12687=EDGE_CURVE('',#10137,#10138,#6434,.T.);
#12688=EDGE_CURVE('',#10138,#10135,#6435,.T.);
#12689=EDGE_CURVE('',#10138,#10133,#5406,.T.);
#12690=EDGE_CURVE('',#10139,#10140,#6436,.T.);
#12691=EDGE_CURVE('',#10141,#10139,#6437,.T.);
#12692=EDGE_CURVE('',#10141,#10142,#6438,.T.);
#12693=EDGE_CURVE('',#10142,#10140,#6439,.T.);
#12694=EDGE_CURVE('',#10140,#10143,#5407,.T.);
#12695=EDGE_CURVE('',#10143,#10142,#6440,.T.);
#12696=EDGE_CURVE('',#10143,#10144,#6441,.T.);
#12697=EDGE_CURVE('',#10144,#10141,#6442,.T.);
#12698=EDGE_CURVE('',#10144,#10139,#5408,.T.);
#12699=EDGE_CURVE('',#10145,#10146,#6443,.T.);
#12700=EDGE_CURVE('',#10147,#10145,#6444,.T.);
#12701=EDGE_CURVE('',#10147,#10148,#6445,.T.);
#12702=EDGE_CURVE('',#10148,#10146,#6446,.T.);
#12703=EDGE_CURVE('',#10146,#10149,#5409,.T.);
#12704=EDGE_CURVE('',#10149,#10148,#6447,.T.);
#12705=EDGE_CURVE('',#10149,#10150,#6448,.T.);
#12706=EDGE_CURVE('',#10150,#10147,#6449,.T.);
#12707=EDGE_CURVE('',#10150,#10145,#5410,.T.);
#12708=EDGE_CURVE('',#10151,#10151,#5411,.T.);
#12709=EDGE_CURVE('',#10151,#10152,#6450,.T.);
#12710=EDGE_CURVE('',#10152,#10152,#5412,.T.);
#12711=EDGE_CURVE('',#10153,#10153,#5413,.T.);
#12712=EDGE_CURVE('',#10153,#10151,#6451,.T.);
#12713=EDGE_CURVE('',#10154,#10154,#5414,.T.);
#12714=EDGE_CURVE('',#10154,#10155,#6452,.T.);
#12715=EDGE_CURVE('',#10155,#10155,#5415,.T.);
#12716=EDGE_CURVE('',#10156,#10156,#5416,.T.);
#12717=EDGE_CURVE('',#10156,#10075,#6453,.T.);
#12718=EDGE_CURVE('',#10078,#10157,#6454,.T.);
#12719=EDGE_CURVE('',#10157,#10157,#5417,.T.);
#12720=EDGE_CURVE('',#10158,#10158,#5418,.T.);
#12721=EDGE_CURVE('',#10159,#10159,#5419,.T.);
#12722=EDGE_CURVE('',#10159,#10158,#6455,.T.);
#12723=EDGE_CURVE('',#10160,#10160,#5420,.T.);
#12724=EDGE_CURVE('',#10160,#10159,#6456,.T.);
#12725=EDGE_CURVE('',#10161,#10162,#6457,.T.);
#12726=EDGE_CURVE('',#10161,#10163,#6458,.T.);
#12727=EDGE_CURVE('',#10164,#10163,#6459,.T.);
#12728=EDGE_CURVE('',#10162,#10164,#6460,.T.);
#12729=EDGE_CURVE('',#10162,#10165,#6461,.T.);
#12730=EDGE_CURVE('',#10166,#10164,#6462,.T.);
#12731=EDGE_CURVE('',#10165,#10166,#6463,.T.);
#12732=EDGE_CURVE('',#10165,#10167,#6464,.T.);
#12733=EDGE_CURVE('',#10168,#10166,#6465,.T.);
#12734=EDGE_CURVE('',#10167,#10168,#6466,.T.);
#12735=EDGE_CURVE('',#10167,#10169,#6467,.T.);
#12736=EDGE_CURVE('',#10170,#10168,#6468,.T.);
#12737=EDGE_CURVE('',#10169,#10170,#6469,.T.);
#12738=EDGE_CURVE('',#10169,#10171,#6470,.T.);
#12739=EDGE_CURVE('',#10172,#10170,#6471,.T.);
#12740=EDGE_CURVE('',#10171,#10172,#6472,.T.);
#12741=EDGE_CURVE('',#10171,#10161,#6473,.T.);
#12742=EDGE_CURVE('',#10163,#10172,#6474,.T.);
#12743=EDGE_CURVE('',#10173,#10174,#6475,.T.);
#12744=EDGE_CURVE('',#10175,#10173,#6476,.T.);
#12745=EDGE_CURVE('',#10176,#10175,#6477,.T.);
#12746=EDGE_CURVE('',#10174,#10176,#6478,.T.);
#12747=EDGE_CURVE('',#9996,#9993,#5421,.F.);
#12748=EDGE_CURVE('',#10173,#10177,#6479,.T.);
#12749=EDGE_CURVE('',#10178,#10177,#6480,.T.);
#12750=EDGE_CURVE('',#10175,#10178,#6481,.T.);
#12751=EDGE_CURVE('',#10179,#10178,#6482,.T.);
#12752=EDGE_CURVE('',#10176,#10179,#6483,.T.);
#12753=EDGE_CURVE('',#10180,#10179,#6484,.T.);
#12754=EDGE_CURVE('',#10174,#10180,#6485,.T.);
#12755=EDGE_CURVE('',#10177,#10180,#6486,.T.);
#12756=EDGE_CURVE('',#10181,#10181,#5422,.T.);
#12757=EDGE_CURVE('',#9948,#10181,#6487,.T.);
#12758=EDGE_CURVE('',#10182,#10182,#5423,.T.);
#12759=EDGE_CURVE('',#10182,#10183,#6488,.T.);
#12760=EDGE_CURVE('',#10183,#10184,#5424,.T.);
#12761=EDGE_CURVE('',#10184,#10183,#5425,.T.);
#12762=EDGE_CURVE('',#10184,#10185,#6489,.T.);
#12763=EDGE_CURVE('',#10186,#10185,#5426,.T.);
#12764=EDGE_CURVE('',#10185,#10186,#5427,.T.);
#12765=EDGE_CURVE('',#10186,#10187,#6490,.T.);
#12766=EDGE_CURVE('',#10187,#10187,#5428,.T.);
#12767=EDGE_CURVE('',#10188,#10188,#5429,.T.);
#12768=EDGE_CURVE('',#10188,#10189,#6491,.T.);
#12769=EDGE_CURVE('',#10189,#10189,#5430,.T.);
#12770=EDGE_CURVE('',#10190,#10190,#5431,.T.);
#12771=EDGE_CURVE('',#10191,#10191,#5432,.T.);
#12772=EDGE_CURVE('',#10192,#10193,#5433,.T.);
#12773=EDGE_CURVE('',#10193,#10192,#5434,.T.);
#12774=EDGE_CURVE('',#10193,#10191,#6492,.T.);
#12775=EDGE_CURVE('',#10194,#10194,#5435,.T.);
#12776=EDGE_CURVE('',#10194,#10195,#6493,.T.);
#12777=EDGE_CURVE('',#10195,#10195,#5436,.T.);
#12778=EDGE_CURVE('',#10196,#10196,#5437,.T.);
#12779=EDGE_CURVE('',#10197,#10197,#5438,.T.);
#12780=EDGE_CURVE('',#10190,#10197,#6494,.T.);
#12781=EDGE_CURVE('',#10198,#10198,#5439,.T.);
#12782=EDGE_CURVE('',#10198,#10192,#6495,.T.);
#12783=EDGE_CURVE('',#10196,#10199,#6496,.T.);
#12784=EDGE_CURVE('',#10200,#10199,#5440,.T.);
#12785=EDGE_CURVE('',#10199,#10200,#5441,.T.);
#12786=EDGE_CURVE('',#10201,#10201,#5442,.T.);
#12787=EDGE_CURVE('',#10200,#10202,#6497,.T.);
#12788=EDGE_CURVE('',#10202,#10202,#5443,.T.);
#12789=EDGE_CURVE('',#10203,#10203,#5444,.T.);
#12790=EDGE_CURVE('',#10201,#10203,#6498,.T.);
#12791=EDGE_CURVE('',#10204,#10205,#5445,.T.);
#12792=EDGE_CURVE('',#10205,#10204,#5446,.T.);
#12793=EDGE_CURVE('',#10204,#10206,#6499,.T.);
#12794=EDGE_CURVE('',#10206,#10207,#5447,.T.);
#12795=EDGE_CURVE('',#10207,#10206,#5448,.T.);
#12796=EDGE_CURVE('',#10207,#10208,#6500,.T.);
#12797=EDGE_CURVE('',#10209,#10208,#5449,.T.);
#12798=EDGE_CURVE('',#10208,#10209,#5450,.T.);
#12799=EDGE_CURVE('',#10210,#10210,#5451,.T.);
#12800=EDGE_CURVE('',#10210,#10205,#6501,.T.);
#12801=EDGE_CURVE('',#10209,#10211,#6502,.T.);
#12802=EDGE_CURVE('',#10211,#10211,#5452,.T.);
#12803=EDGE_CURVE('',#10212,#10212,#5453,.T.);
#12804=EDGE_CURVE('',#10213,#10214,#6503,.T.);
#12805=EDGE_CURVE('',#10215,#10213,#6504,.T.);
#12806=EDGE_CURVE('',#10215,#10216,#6505,.T.);
#12807=EDGE_CURVE('',#10216,#10214,#6506,.T.);
#12808=EDGE_CURVE('',#10214,#10217,#5454,.T.);
#12809=EDGE_CURVE('',#10217,#10216,#6507,.T.);
#12810=EDGE_CURVE('',#10217,#10218,#6508,.T.);
#12811=EDGE_CURVE('',#10218,#10215,#6509,.T.);
#12812=EDGE_CURVE('',#10218,#10213,#5455,.T.);
#12813=EDGE_CURVE('',#10219,#10220,#6510,.T.);
#12814=EDGE_CURVE('',#10221,#10219,#6511,.T.);
#12815=EDGE_CURVE('',#10221,#10222,#6512,.T.);
#12816=EDGE_CURVE('',#10222,#10220,#6513,.T.);
#12817=EDGE_CURVE('',#10220,#10223,#5456,.T.);
#12818=EDGE_CURVE('',#10223,#10222,#6514,.T.);
#12819=EDGE_CURVE('',#10223,#10224,#6515,.T.);
#12820=EDGE_CURVE('',#10224,#10221,#6516,.T.);
#12821=EDGE_CURVE('',#10224,#10219,#5457,.T.);
#12822=EDGE_CURVE('',#10225,#10226,#6517,.T.);
#12823=EDGE_CURVE('',#10227,#10225,#6518,.T.);
#12824=EDGE_CURVE('',#10227,#10228,#6519,.T.);
#12825=EDGE_CURVE('',#10228,#10226,#6520,.T.);
#12826=EDGE_CURVE('',#10226,#10229,#5458,.T.);
#12827=EDGE_CURVE('',#10229,#10228,#6521,.T.);
#12828=EDGE_CURVE('',#10229,#10230,#6522,.T.);
#12829=EDGE_CURVE('',#10230,#10227,#6523,.T.);
#12830=EDGE_CURVE('',#10230,#10225,#5459,.T.);
#12831=EDGE_CURVE('',#10231,#10232,#6524,.T.);
#12832=EDGE_CURVE('',#10233,#10231,#6525,.T.);
#12833=EDGE_CURVE('',#10233,#10234,#6526,.T.);
#12834=EDGE_CURVE('',#10234,#10232,#6527,.T.);
#12835=EDGE_CURVE('',#10232,#10235,#5460,.T.);
#12836=EDGE_CURVE('',#10235,#10234,#6528,.T.);
#12837=EDGE_CURVE('',#10235,#10236,#6529,.T.);
#12838=EDGE_CURVE('',#10236,#10233,#6530,.T.);
#12839=EDGE_CURVE('',#10236,#10231,#5461,.T.);
#12840=EDGE_CURVE('',#10237,#10238,#6531,.T.);
#12841=EDGE_CURVE('',#10239,#10237,#6532,.T.);
#12842=EDGE_CURVE('',#10239,#10240,#6533,.T.);
#12843=EDGE_CURVE('',#10240,#10238,#6534,.T.);
#12844=EDGE_CURVE('',#10238,#10241,#5462,.T.);
#12845=EDGE_CURVE('',#10241,#10240,#6535,.T.);
#12846=EDGE_CURVE('',#10241,#10242,#6536,.T.);
#12847=EDGE_CURVE('',#10242,#10239,#6537,.T.);
#12848=EDGE_CURVE('',#10242,#10237,#5463,.T.);
#12849=EDGE_CURVE('',#10243,#10244,#6538,.T.);
#12850=EDGE_CURVE('',#10245,#10243,#6539,.T.);
#12851=EDGE_CURVE('',#10245,#10246,#6540,.T.);
#12852=EDGE_CURVE('',#10246,#10244,#6541,.T.);
#12853=EDGE_CURVE('',#10244,#10247,#5464,.T.);
#12854=EDGE_CURVE('',#10247,#10246,#6542,.T.);
#12855=EDGE_CURVE('',#10247,#10248,#6543,.T.);
#12856=EDGE_CURVE('',#10248,#10245,#6544,.T.);
#12857=EDGE_CURVE('',#10248,#10243,#5465,.T.);
#12858=EDGE_CURVE('',#10249,#10250,#6545,.T.);
#12859=EDGE_CURVE('',#10251,#10249,#6546,.T.);
#12860=EDGE_CURVE('',#10251,#10252,#6547,.T.);
#12861=EDGE_CURVE('',#10252,#10250,#6548,.T.);
#12862=EDGE_CURVE('',#10250,#10253,#5466,.T.);
#12863=EDGE_CURVE('',#10253,#10252,#6549,.T.);
#12864=EDGE_CURVE('',#10253,#10254,#6550,.T.);
#12865=EDGE_CURVE('',#10254,#10251,#6551,.T.);
#12866=EDGE_CURVE('',#10254,#10249,#5467,.T.);
#12867=EDGE_CURVE('',#10255,#10256,#6552,.T.);
#12868=EDGE_CURVE('',#10257,#10255,#6553,.T.);
#12869=EDGE_CURVE('',#10257,#10258,#6554,.T.);
#12870=EDGE_CURVE('',#10258,#10256,#6555,.T.);
#12871=EDGE_CURVE('',#10256,#10259,#5468,.T.);
#12872=EDGE_CURVE('',#10259,#10258,#6556,.T.);
#12873=EDGE_CURVE('',#10259,#10260,#6557,.T.);
#12874=EDGE_CURVE('',#10260,#10257,#6558,.T.);
#12875=EDGE_CURVE('',#10260,#10255,#5469,.T.);
#12876=EDGE_CURVE('',#10261,#10262,#6559,.T.);
#12877=EDGE_CURVE('',#10263,#10261,#6560,.T.);
#12878=EDGE_CURVE('',#10263,#10264,#6561,.T.);
#12879=EDGE_CURVE('',#10264,#10262,#6562,.T.);
#12880=EDGE_CURVE('',#10262,#10265,#5470,.T.);
#12881=EDGE_CURVE('',#10266,#10264,#6563,.T.);
#12882=EDGE_CURVE('',#10265,#10266,#5471,.T.);
#12883=EDGE_CURVE('',#10266,#10267,#6564,.T.);
#12884=EDGE_CURVE('',#10267,#10263,#6565,.T.);
#12885=EDGE_CURVE('',#10267,#10268,#5472,.T.);
#12886=EDGE_CURVE('',#10268,#10261,#5473,.T.);
#12887=EDGE_CURVE('',#10269,#10270,#6566,.T.);
#12888=EDGE_CURVE('',#10271,#10269,#6567,.T.);
#12889=EDGE_CURVE('',#10271,#10272,#6568,.T.);
#12890=EDGE_CURVE('',#10272,#10270,#6569,.T.);
#12891=EDGE_CURVE('',#10270,#10273,#5474,.T.);
#12892=EDGE_CURVE('',#10273,#10272,#6570,.T.);
#12893=EDGE_CURVE('',#10273,#10274,#6571,.T.);
#12894=EDGE_CURVE('',#10274,#10271,#6572,.T.);
#12895=EDGE_CURVE('',#10274,#10269,#5475,.T.);
#12896=EDGE_CURVE('',#10275,#10276,#6573,.T.);
#12897=EDGE_CURVE('',#10277,#10275,#6574,.T.);
#12898=EDGE_CURVE('',#10277,#10278,#6575,.T.);
#12899=EDGE_CURVE('',#10278,#10276,#6576,.T.);
#12900=EDGE_CURVE('',#10276,#10279,#5476,.T.);
#12901=EDGE_CURVE('',#10279,#10278,#6577,.T.);
#12902=EDGE_CURVE('',#10279,#10280,#6578,.T.);
#12903=EDGE_CURVE('',#10280,#10277,#6579,.T.);
#12904=EDGE_CURVE('',#10280,#10275,#5477,.T.);
#12905=EDGE_CURVE('',#10281,#10282,#6580,.T.);
#12906=EDGE_CURVE('',#10283,#10281,#6581,.T.);
#12907=EDGE_CURVE('',#10283,#10284,#6582,.T.);
#12908=EDGE_CURVE('',#10284,#10282,#6583,.T.);
#12909=EDGE_CURVE('',#10282,#10285,#5478,.T.);
#12910=EDGE_CURVE('',#10285,#10284,#6584,.T.);
#12911=EDGE_CURVE('',#10285,#10286,#6585,.T.);
#12912=EDGE_CURVE('',#10286,#10283,#6586,.T.);
#12913=EDGE_CURVE('',#10286,#10281,#5479,.T.);
#12914=EDGE_CURVE('',#10287,#10288,#6587,.T.);
#12915=EDGE_CURVE('',#10289,#10287,#6588,.T.);
#12916=EDGE_CURVE('',#10289,#10290,#6589,.T.);
#12917=EDGE_CURVE('',#10290,#10288,#6590,.T.);
#12918=EDGE_CURVE('',#10288,#10291,#5480,.T.);
#12919=EDGE_CURVE('',#10291,#10290,#6591,.T.);
#12920=EDGE_CURVE('',#10291,#10292,#6592,.T.);
#12921=EDGE_CURVE('',#10292,#10289,#6593,.T.);
#12922=EDGE_CURVE('',#10292,#10287,#5481,.T.);
#12923=EDGE_CURVE('',#10293,#10294,#6594,.T.);
#12924=EDGE_CURVE('',#10295,#10293,#6595,.T.);
#12925=EDGE_CURVE('',#10295,#10296,#6596,.T.);
#12926=EDGE_CURVE('',#10296,#10294,#6597,.T.);
#12927=EDGE_CURVE('',#10294,#10297,#5482,.T.);
#12928=EDGE_CURVE('',#10297,#10296,#6598,.T.);
#12929=EDGE_CURVE('',#10297,#10298,#6599,.T.);
#12930=EDGE_CURVE('',#10298,#10295,#6600,.T.);
#12931=EDGE_CURVE('',#10298,#10293,#5483,.T.);
#12932=EDGE_CURVE('',#10299,#10300,#6601,.T.);
#12933=EDGE_CURVE('',#10301,#10299,#6602,.T.);
#12934=EDGE_CURVE('',#10301,#10302,#6603,.T.);
#12935=EDGE_CURVE('',#10302,#10300,#6604,.T.);
#12936=EDGE_CURVE('',#10300,#10303,#5484,.T.);
#12937=EDGE_CURVE('',#10303,#10302,#6605,.T.);
#12938=EDGE_CURVE('',#10303,#10304,#6606,.T.);
#12939=EDGE_CURVE('',#10304,#10301,#6607,.T.);
#12940=EDGE_CURVE('',#10304,#10299,#5485,.T.);
#12941=EDGE_CURVE('',#10305,#10306,#6608,.T.);
#12942=EDGE_CURVE('',#10307,#10305,#6609,.T.);
#12943=EDGE_CURVE('',#10307,#10308,#6610,.T.);
#12944=EDGE_CURVE('',#10308,#10306,#6611,.T.);
#12945=EDGE_CURVE('',#10306,#10309,#5486,.T.);
#12946=EDGE_CURVE('',#10309,#10308,#6612,.T.);
#12947=EDGE_CURVE('',#10309,#10310,#6613,.T.);
#12948=EDGE_CURVE('',#10310,#10307,#6614,.T.);
#12949=EDGE_CURVE('',#10310,#10305,#5487,.T.);
#12950=EDGE_CURVE('',#10311,#10312,#6615,.T.);
#12951=EDGE_CURVE('',#10313,#10311,#6616,.T.);
#12952=EDGE_CURVE('',#10313,#10314,#6617,.T.);
#12953=EDGE_CURVE('',#10314,#10312,#6618,.T.);
#12954=EDGE_CURVE('',#10312,#10315,#5488,.T.);
#12955=EDGE_CURVE('',#10315,#10314,#6619,.T.);
#12956=EDGE_CURVE('',#10315,#10316,#6620,.T.);
#12957=EDGE_CURVE('',#10316,#10313,#6621,.T.);
#12958=EDGE_CURVE('',#10316,#10311,#5489,.T.);
#12959=EDGE_CURVE('',#10317,#10318,#6622,.T.);
#12960=EDGE_CURVE('',#10319,#10317,#6623,.T.);
#12961=EDGE_CURVE('',#10319,#10320,#6624,.T.);
#12962=EDGE_CURVE('',#10320,#10318,#6625,.T.);
#12963=EDGE_CURVE('',#10318,#10321,#5490,.T.);
#12964=EDGE_CURVE('',#10321,#10320,#6626,.T.);
#12965=EDGE_CURVE('',#10321,#10322,#6627,.T.);
#12966=EDGE_CURVE('',#10322,#10319,#6628,.T.);
#12967=EDGE_CURVE('',#10322,#10317,#5491,.T.);
#12968=EDGE_CURVE('',#10323,#10323,#5492,.T.);
#12969=EDGE_CURVE('',#10323,#10324,#6629,.T.);
#12970=EDGE_CURVE('',#10324,#10324,#5493,.T.);
#12971=EDGE_CURVE('',#10325,#10325,#5494,.T.);
#12972=EDGE_CURVE('',#10325,#10326,#6630,.T.);
#12973=EDGE_CURVE('',#10326,#10326,#5495,.T.);
#12974=EDGE_CURVE('',#10327,#10327,#5496,.T.);
#12975=EDGE_CURVE('',#10328,#10328,#5497,.T.);
#12976=EDGE_CURVE('',#10328,#10327,#6631,.T.);
#12977=EDGE_CURVE('',#10212,#10328,#6632,.T.);
#12978=EDGE_CURVE('',#10329,#10329,#5498,.T.);
#12979=EDGE_CURVE('',#10330,#10330,#5499,.T.);
#12980=EDGE_CURVE('',#10330,#10265,#6633,.T.);
#12981=EDGE_CURVE('',#10268,#10329,#6634,.T.);
#12982=EDGE_CURVE('',#10331,#10331,#5500,.T.);
#12983=EDGE_CURVE('',#10332,#10332,#5501,.T.);
#12984=EDGE_CURVE('',#10332,#10331,#6635,.T.);
#12985=EDGE_CURVE('',#10333,#10333,#5502,.T.);
#12986=EDGE_CURVE('',#10333,#10334,#6636,.T.);
#12987=EDGE_CURVE('',#10334,#10334,#5503,.T.);
#12988=EDGE_CURVE('',#10335,#10335,#5504,.T.);
#12989=EDGE_CURVE('',#10336,#10336,#5505,.T.);
#12990=EDGE_CURVE('',#10336,#10335,#6637,.T.);
#12991=EDGE_CURVE('',#10337,#10337,#5506,.T.);
#12992=EDGE_CURVE('',#10337,#10338,#6638,.T.);
#12993=EDGE_CURVE('',#10338,#10338,#5507,.T.);
#12994=EDGE_CURVE('',#10338,#10339,#6639,.T.);
#12995=EDGE_CURVE('',#10340,#10339,#5508,.T.);
#12996=EDGE_CURVE('',#10339,#10340,#5509,.T.);
#12997=EDGE_CURVE('',#10341,#10342,#6640,.T.);
#12998=EDGE_CURVE('',#10343,#10341,#5510,.T.);
#12999=EDGE_CURVE('',#10344,#10343,#6641,.T.);
#13000=EDGE_CURVE('',#10345,#10344,#5511,.T.);
#13001=EDGE_CURVE('',#10346,#10345,#6642,.T.);
#13002=EDGE_CURVE('',#10346,#10342,#6643,.T.);
#13003=EDGE_CURVE('',#10347,#10347,#5512,.T.);
#13004=EDGE_CURVE('',#10347,#10340,#6644,.T.);
#13005=EDGE_CURVE('',#10348,#10349,#5513,.T.);
#13006=EDGE_CURVE('',#10350,#10348,#6645,.T.);
#13007=EDGE_CURVE('',#10351,#10350,#5514,.T.);
#13008=EDGE_CURVE('',#10352,#10351,#6646,.T.);
#13009=EDGE_CURVE('',#10353,#10352,#5515,.T.);
#13010=EDGE_CURVE('',#10354,#10353,#6647,.T.);
#13011=EDGE_CURVE('',#10355,#10354,#5516,.T.);
#13012=EDGE_CURVE('',#10349,#10355,#6648,.T.);
#13013=EDGE_CURVE('',#10356,#10346,#6649,.F.);
#13014=EDGE_CURVE('',#10345,#10357,#6650,.T.);
#13015=EDGE_CURVE('',#10357,#10356,#6651,.T.);
#13016=EDGE_CURVE('',#10344,#10358,#6652,.T.);
#13017=EDGE_CURVE('',#10358,#10357,#5517,.T.);
#13018=EDGE_CURVE('',#10343,#10359,#6653,.T.);
#13019=EDGE_CURVE('',#10359,#10358,#6654,.T.);
#13020=EDGE_CURVE('',#10341,#10360,#6655,.T.);
#13021=EDGE_CURVE('',#10360,#10359,#5518,.T.);
#13022=EDGE_CURVE('',#10342,#10361,#6656,.F.);
#13023=EDGE_CURVE('',#10361,#10360,#6657,.T.);
#13024=EDGE_CURVE('',#10362,#10363,#6658,.T.);
#13025=EDGE_CURVE('',#10363,#10364,#6659,.T.);
#13026=EDGE_CURVE('',#10364,#10365,#6660,.T.);
#13027=EDGE_CURVE('',#10365,#10362,#6661,.T.);
#13028=EDGE_CURVE('',#10365,#10366,#6662,.T.);
#13029=EDGE_CURVE('',#10366,#10367,#6663,.T.);
#13030=EDGE_CURVE('',#10367,#10362,#6664,.T.);
#13031=EDGE_CURVE('',#10368,#10369,#6665,.T.);
#13032=EDGE_CURVE('',#10369,#10367,#5519,.T.);
#13033=EDGE_CURVE('',#10366,#10368,#5520,.T.);
#13034=EDGE_CURVE('',#10370,#10371,#6666,.T.);
#13035=EDGE_CURVE('',#10371,#10369,#6667,.T.);
#13036=EDGE_CURVE('',#10368,#10370,#6668,.T.);
#13037=EDGE_CURVE('',#10372,#10373,#6669,.T.);
#13038=EDGE_CURVE('',#10373,#10371,#5521,.T.);
#13039=EDGE_CURVE('',#10370,#10372,#5522,.T.);
#13040=EDGE_CURVE('',#10363,#10373,#6670,.T.);
#13041=EDGE_CURVE('',#10372,#10364,#6671,.T.);
#13042=EDGE_CURVE('',#10373,#10374,#6672,.T.);
#13043=EDGE_CURVE('',#10375,#10374,#5523,.T.);
#13044=EDGE_CURVE('',#10375,#10371,#6673,.T.);
#13045=EDGE_CURVE('',#10376,#10357,#6674,.T.);
#13046=EDGE_CURVE('',#10374,#10376,#6675,.T.);
#13047=EDGE_CURVE('',#10363,#10356,#6676,.T.);
#13048=EDGE_CURVE('',#10362,#10361,#6677,.T.);
#13049=EDGE_CURVE('',#10349,#10377,#6678,.T.);
#13050=EDGE_CURVE('',#10377,#10378,#5524,.T.);
#13051=EDGE_CURVE('',#10378,#10348,#6679,.T.);
#13052=EDGE_CURVE('',#10355,#10379,#6680,.T.);
#13053=EDGE_CURVE('',#10379,#10377,#6681,.T.);
#13054=EDGE_CURVE('',#10354,#10380,#6682,.T.);
#13055=EDGE_CURVE('',#10380,#10379,#5525,.T.);
#13056=EDGE_CURVE('',#10353,#10381,#6683,.T.);
#13057=EDGE_CURVE('',#10381,#10380,#6684,.T.);
#13058=EDGE_CURVE('',#10352,#10376,#6685,.T.);
#13059=EDGE_CURVE('',#10376,#10381,#5526,.T.);
#13060=EDGE_CURVE('',#10351,#10374,#6686,.T.);
#13061=EDGE_CURVE('',#10350,#10375,#6687,.T.);
#13062=EDGE_CURVE('',#10378,#10375,#6688,.T.);
#13063=EDGE_CURVE('',#10369,#10378,#6689,.T.);
#13064=EDGE_CURVE('',#10377,#10367,#6690,.T.);
#13065=EDGE_CURVE('',#10360,#10379,#6691,.T.);
#13066=EDGE_CURVE('',#10380,#10359,#6692,.T.);
#13067=EDGE_CURVE('',#10358,#10381,#6693,.T.);
#13068=EDGE_CURVE('',#10382,#10382,#5527,.T.);
#13069=EDGE_CURVE('',#10382,#10383,#6694,.T.);
#13070=EDGE_CURVE('',#10383,#10383,#5528,.T.);
#13071=EDGE_CURVE('',#10383,#10384,#6695,.T.);
#13072=EDGE_CURVE('',#10384,#10384,#5529,.T.);
#13073=EDGE_CURVE('',#10385,#10385,#5530,.T.);
#13074=EDGE_CURVE('',#10385,#10384,#6696,.T.);
#13075=EDGE_CURVE('',#10382,#10385,#6697,.T.);
#13076=EDGE_CURVE('',#10386,#10387,#6698,.T.);
#13077=EDGE_CURVE('',#10386,#10388,#424,.T.);
#13078=EDGE_CURVE('',#10388,#10389,#5531,.T.);
#13079=EDGE_CURVE('',#10389,#10390,#6699,.T.);
#13080=EDGE_CURVE('',#10390,#10390,#5532,.T.);
#13081=EDGE_CURVE('',#10389,#10391,#5533,.T.);
#13082=EDGE_CURVE('',#10391,#10387,#425,.T.);
#13083=EDGE_CURVE('',#10392,#10393,#6700,.T.);
#13084=EDGE_CURVE('',#10392,#10386,#426,.T.);
#13085=EDGE_CURVE('',#10387,#10393,#427,.T.);
#13086=EDGE_CURVE('',#10394,#10395,#6701,.T.);
#13087=EDGE_CURVE('',#10394,#10392,#428,.T.);
#13088=EDGE_CURVE('',#10393,#10395,#429,.T.);
#13089=EDGE_CURVE('',#10396,#10397,#6702,.T.);
#13090=EDGE_CURVE('',#10396,#10394,#430,.T.);
#13091=EDGE_CURVE('',#10395,#10397,#431,.T.);
#13092=EDGE_CURVE('',#10398,#10399,#6703,.T.);
#13093=EDGE_CURVE('',#10398,#10396,#432,.T.);
#13094=EDGE_CURVE('',#10397,#10399,#433,.T.);
#13095=EDGE_CURVE('',#10400,#10401,#6704,.T.);
#13096=EDGE_CURVE('',#10400,#10398,#434,.T.);
#13097=EDGE_CURVE('',#10399,#10401,#435,.T.);
#13098=EDGE_CURVE('',#10402,#10403,#6705,.T.);
#13099=EDGE_CURVE('',#10402,#10400,#436,.T.);
#13100=EDGE_CURVE('',#10401,#10403,#437,.T.);
#13101=EDGE_CURVE('',#10404,#10405,#6706,.T.);
#13102=EDGE_CURVE('',#10404,#10402,#438,.T.);
#13103=EDGE_CURVE('',#10403,#10405,#439,.T.);
#13104=EDGE_CURVE('',#10406,#10407,#6707,.T.);
#13105=EDGE_CURVE('',#10406,#10404,#440,.T.);
#13106=EDGE_CURVE('',#10405,#10407,#441,.T.);
#13107=EDGE_CURVE('',#10408,#10409,#6708,.T.);
#13108=EDGE_CURVE('',#10408,#10406,#442,.T.);
#13109=EDGE_CURVE('',#10407,#10409,#443,.T.);
#13110=EDGE_CURVE('',#10410,#10411,#6709,.T.);
#13111=EDGE_CURVE('',#10410,#10408,#444,.T.);
#13112=EDGE_CURVE('',#10409,#10411,#445,.T.);
#13113=EDGE_CURVE('',#10412,#10413,#6710,.T.);
#13114=EDGE_CURVE('',#10412,#10410,#446,.T.);
#13115=EDGE_CURVE('',#10411,#10413,#447,.T.);
#13116=EDGE_CURVE('',#10414,#10415,#6711,.T.);
#13117=EDGE_CURVE('',#10414,#10412,#448,.T.);
#13118=EDGE_CURVE('',#10413,#10415,#449,.T.);
#13119=EDGE_CURVE('',#10416,#10417,#6712,.T.);
#13120=EDGE_CURVE('',#10416,#10414,#450,.T.);
#13121=EDGE_CURVE('',#10415,#10417,#451,.T.);
#13122=EDGE_CURVE('',#10418,#10419,#6713,.T.);
#13123=EDGE_CURVE('',#10418,#10420,#452,.T.);
#13124=EDGE_CURVE('',#10421,#10420,#5534,.T.);
#13125=EDGE_CURVE('',#10419,#10421,#453,.T.);
#13126=EDGE_CURVE('',#10422,#10423,#6714,.T.);
#13127=EDGE_CURVE('',#10422,#10418,#454,.T.);
#13128=EDGE_CURVE('',#10423,#10419,#455,.T.);
#13129=EDGE_CURVE('',#10424,#10425,#6715,.T.);
#13130=EDGE_CURVE('',#10424,#10422,#456,.T.);
#13131=EDGE_CURVE('',#10425,#10423,#457,.T.);
#13132=EDGE_CURVE('',#10426,#10427,#6716,.T.);
#13133=EDGE_CURVE('',#10426,#10424,#458,.T.);
#13134=EDGE_CURVE('',#10427,#10425,#459,.T.);
#13135=EDGE_CURVE('',#10428,#10429,#6717,.T.);
#13136=EDGE_CURVE('',#10428,#10426,#460,.T.);
#13137=EDGE_CURVE('',#10429,#10427,#461,.T.);
#13138=EDGE_CURVE('',#10430,#10431,#6718,.T.);
#13139=EDGE_CURVE('',#10430,#10428,#462,.T.);
#13140=EDGE_CURVE('',#10431,#10429,#463,.T.);
#13141=EDGE_CURVE('',#10432,#10433,#6719,.T.);
#13142=EDGE_CURVE('',#10432,#10430,#464,.T.);
#13143=EDGE_CURVE('',#10433,#10431,#465,.T.);
#13144=EDGE_CURVE('',#10434,#10435,#6720,.T.);
#13145=EDGE_CURVE('',#10434,#10432,#466,.T.);
#13146=EDGE_CURVE('',#10435,#10433,#467,.T.);
#13147=EDGE_CURVE('',#10436,#10437,#6721,.T.);
#13148=EDGE_CURVE('',#10436,#10434,#468,.T.);
#13149=EDGE_CURVE('',#10437,#10435,#469,.T.);
#13150=EDGE_CURVE('',#10438,#10439,#6722,.T.);
#13151=EDGE_CURVE('',#10438,#10436,#470,.T.);
#13152=EDGE_CURVE('',#10439,#10437,#471,.T.);
#13153=EDGE_CURVE('',#10440,#10441,#6723,.T.);
#13154=EDGE_CURVE('',#10440,#10438,#472,.T.);
#13155=EDGE_CURVE('',#10441,#10439,#473,.T.);
#13156=EDGE_CURVE('',#10442,#10443,#6724,.T.);
#13157=EDGE_CURVE('',#10442,#10440,#474,.T.);
#13158=EDGE_CURVE('',#10443,#10441,#475,.T.);
#13159=EDGE_CURVE('',#10444,#10445,#6725,.T.);
#13160=EDGE_CURVE('',#10444,#10442,#476,.T.);
#13161=EDGE_CURVE('',#10445,#10443,#477,.T.);
#13162=EDGE_CURVE('',#10446,#10447,#6726,.T.);
#13163=EDGE_CURVE('',#10446,#10444,#478,.T.);
#13164=EDGE_CURVE('',#10447,#10445,#479,.T.);
#13165=EDGE_CURVE('',#10448,#10449,#6727,.T.);
#13166=EDGE_CURVE('',#10450,#10448,#5535,.T.);
#13167=EDGE_CURVE('',#10450,#10446,#480,.T.);
#13168=EDGE_CURVE('',#10449,#10447,#481,.T.);
#13169=EDGE_CURVE('',#10451,#10421,#482,.T.);
#13170=EDGE_CURVE('',#10417,#10451,#483,.T.);
#13171=EDGE_CURVE('',#10452,#10391,#484,.T.);
#13172=EDGE_CURVE('',#10452,#10449,#485,.T.);
#13173=EDGE_CURVE('',#10388,#10450,#486,.T.);
#13174=EDGE_CURVE('',#10448,#10452,#5536,.T.);
#13175=EDGE_CURVE('',#10420,#10453,#487,.T.);
#13176=EDGE_CURVE('',#10453,#10416,#488,.T.);
#13177=EDGE_CURVE('',#10453,#10451,#5537,.T.);
#13178=EDGE_CURVE('',#10454,#10455,#6728,.T.);
#13179=EDGE_CURVE('',#10455,#10455,#5538,.T.);
#13180=EDGE_CURVE('',#10456,#10457,#6729,.T.);
#13181=EDGE_CURVE('',#10458,#10456,#6730,.T.);
#13182=EDGE_CURVE('',#10458,#10459,#6731,.T.);
#13183=EDGE_CURVE('',#10459,#10457,#6732,.T.);
#13184=EDGE_CURVE('',#10457,#10460,#5539,.T.);
#13185=EDGE_CURVE('',#10460,#10459,#6733,.T.);
#13186=EDGE_CURVE('',#10460,#10461,#6734,.T.);
#13187=EDGE_CURVE('',#10461,#10458,#6735,.T.);
#13188=EDGE_CURVE('',#10461,#10456,#5540,.T.);
#13189=EDGE_CURVE('',#10462,#10463,#6736,.T.);
#13190=EDGE_CURVE('',#10464,#10462,#6737,.T.);
#13191=EDGE_CURVE('',#10464,#10465,#6738,.T.);
#13192=EDGE_CURVE('',#10465,#10463,#6739,.T.);
#13193=EDGE_CURVE('',#10463,#10466,#5541,.T.);
#13194=EDGE_CURVE('',#10466,#10465,#6740,.T.);
#13195=EDGE_CURVE('',#10466,#10467,#6741,.T.);
#13196=EDGE_CURVE('',#10467,#10464,#6742,.T.);
#13197=EDGE_CURVE('',#10467,#10462,#5542,.T.);
#13198=EDGE_CURVE('',#10468,#10469,#6743,.T.);
#13199=EDGE_CURVE('',#10470,#10468,#6744,.T.);
#13200=EDGE_CURVE('',#10470,#10471,#6745,.T.);
#13201=EDGE_CURVE('',#10471,#10469,#6746,.T.);
#13202=EDGE_CURVE('',#10469,#10472,#5543,.T.);
#13203=EDGE_CURVE('',#10472,#10471,#6747,.T.);
#13204=EDGE_CURVE('',#10472,#10473,#6748,.T.);
#13205=EDGE_CURVE('',#10473,#10470,#6749,.T.);
#13206=EDGE_CURVE('',#10473,#10468,#5544,.T.);
#13207=EDGE_CURVE('',#10474,#10475,#6750,.T.);
#13208=EDGE_CURVE('',#10476,#10474,#6751,.T.);
#13209=EDGE_CURVE('',#10476,#10477,#6752,.T.);
#13210=EDGE_CURVE('',#10477,#10475,#6753,.T.);
#13211=EDGE_CURVE('',#10475,#10478,#5545,.T.);
#13212=EDGE_CURVE('',#10478,#10477,#6754,.T.);
#13213=EDGE_CURVE('',#10478,#10479,#6755,.T.);
#13214=EDGE_CURVE('',#10479,#10476,#6756,.T.);
#13215=EDGE_CURVE('',#10479,#10474,#5546,.T.);
#13216=EDGE_CURVE('',#10480,#10481,#6757,.T.);
#13217=EDGE_CURVE('',#10482,#10480,#6758,.T.);
#13218=EDGE_CURVE('',#10482,#10483,#6759,.T.);
#13219=EDGE_CURVE('',#10483,#10481,#6760,.T.);
#13220=EDGE_CURVE('',#10481,#10484,#5547,.T.);
#13221=EDGE_CURVE('',#10484,#10483,#6761,.T.);
#13222=EDGE_CURVE('',#10484,#10485,#6762,.T.);
#13223=EDGE_CURVE('',#10485,#10482,#6763,.T.);
#13224=EDGE_CURVE('',#10485,#10480,#5548,.T.);
#13225=EDGE_CURVE('',#10486,#10487,#6764,.T.);
#13226=EDGE_CURVE('',#10488,#10486,#6765,.T.);
#13227=EDGE_CURVE('',#10488,#10489,#6766,.T.);
#13228=EDGE_CURVE('',#10489,#10487,#6767,.T.);
#13229=EDGE_CURVE('',#10487,#10490,#5549,.T.);
#13230=EDGE_CURVE('',#10490,#10489,#6768,.T.);
#13231=EDGE_CURVE('',#10490,#10491,#6769,.T.);
#13232=EDGE_CURVE('',#10491,#10488,#6770,.T.);
#13233=EDGE_CURVE('',#10491,#10486,#5550,.T.);
#13234=EDGE_CURVE('',#10492,#10493,#6771,.T.);
#13235=EDGE_CURVE('',#10494,#10492,#6772,.T.);
#13236=EDGE_CURVE('',#10494,#10495,#6773,.T.);
#13237=EDGE_CURVE('',#10495,#10493,#6774,.T.);
#13238=EDGE_CURVE('',#10493,#10496,#5551,.T.);
#13239=EDGE_CURVE('',#10496,#10495,#6775,.T.);
#13240=EDGE_CURVE('',#10496,#10497,#6776,.T.);
#13241=EDGE_CURVE('',#10497,#10494,#6777,.T.);
#13242=EDGE_CURVE('',#10497,#10492,#5552,.T.);
#13243=EDGE_CURVE('',#10498,#10499,#6778,.T.);
#13244=EDGE_CURVE('',#10500,#10498,#6779,.T.);
#13245=EDGE_CURVE('',#10500,#10501,#6780,.T.);
#13246=EDGE_CURVE('',#10501,#10499,#6781,.T.);
#13247=EDGE_CURVE('',#10499,#10502,#5553,.T.);
#13248=EDGE_CURVE('',#10502,#10501,#6782,.T.);
#13249=EDGE_CURVE('',#10502,#10503,#6783,.T.);
#13250=EDGE_CURVE('',#10503,#10500,#6784,.T.);
#13251=EDGE_CURVE('',#10503,#10498,#5554,.T.);
#13252=EDGE_CURVE('',#10504,#10505,#6785,.T.);
#13253=EDGE_CURVE('',#10506,#10504,#6786,.T.);
#13254=EDGE_CURVE('',#10506,#10507,#6787,.T.);
#13255=EDGE_CURVE('',#10507,#10505,#6788,.T.);
#13256=EDGE_CURVE('',#10505,#10508,#5555,.T.);
#13257=EDGE_CURVE('',#10508,#10507,#6789,.T.);
#13258=EDGE_CURVE('',#10508,#10509,#6790,.T.);
#13259=EDGE_CURVE('',#10509,#10506,#6791,.T.);
#13260=EDGE_CURVE('',#10509,#10504,#5556,.T.);
#13261=EDGE_CURVE('',#10510,#10511,#6792,.T.);
#13262=EDGE_CURVE('',#10512,#10510,#6793,.T.);
#13263=EDGE_CURVE('',#10512,#10513,#6794,.T.);
#13264=EDGE_CURVE('',#10513,#10511,#6795,.T.);
#13265=EDGE_CURVE('',#10511,#10514,#5557,.T.);
#13266=EDGE_CURVE('',#10514,#10513,#6796,.T.);
#13267=EDGE_CURVE('',#10514,#10515,#6797,.T.);
#13268=EDGE_CURVE('',#10515,#10512,#6798,.T.);
#13269=EDGE_CURVE('',#10515,#10510,#5558,.T.);
#13270=EDGE_CURVE('',#10516,#10517,#6799,.T.);
#13271=EDGE_CURVE('',#10518,#10516,#6800,.T.);
#13272=EDGE_CURVE('',#10518,#10519,#6801,.T.);
#13273=EDGE_CURVE('',#10519,#10517,#6802,.T.);
#13274=EDGE_CURVE('',#10517,#10520,#5559,.T.);
#13275=EDGE_CURVE('',#10520,#10519,#6803,.T.);
#13276=EDGE_CURVE('',#10520,#10521,#6804,.T.);
#13277=EDGE_CURVE('',#10521,#10518,#6805,.T.);
#13278=EDGE_CURVE('',#10521,#10516,#5560,.T.);
#13279=EDGE_CURVE('',#10522,#10523,#6806,.T.);
#13280=EDGE_CURVE('',#10524,#10522,#6807,.T.);
#13281=EDGE_CURVE('',#10524,#10525,#6808,.T.);
#13282=EDGE_CURVE('',#10525,#10523,#6809,.T.);
#13283=EDGE_CURVE('',#10523,#10526,#5561,.T.);
#13284=EDGE_CURVE('',#10527,#10525,#6810,.T.);
#13285=EDGE_CURVE('',#10526,#10527,#5562,.T.);
#13286=EDGE_CURVE('',#10527,#10528,#6811,.T.);
#13287=EDGE_CURVE('',#10528,#10524,#6812,.T.);
#13288=EDGE_CURVE('',#10528,#10529,#5563,.T.);
#13289=EDGE_CURVE('',#10529,#10522,#5564,.T.);
#13290=EDGE_CURVE('',#10530,#10531,#6813,.T.);
#13291=EDGE_CURVE('',#10532,#10530,#6814,.T.);
#13292=EDGE_CURVE('',#10532,#10533,#6815,.T.);
#13293=EDGE_CURVE('',#10533,#10531,#6816,.T.);
#13294=EDGE_CURVE('',#10531,#10534,#5565,.T.);
#13295=EDGE_CURVE('',#10534,#10533,#6817,.T.);
#13296=EDGE_CURVE('',#10534,#10535,#6818,.T.);
#13297=EDGE_CURVE('',#10535,#10532,#6819,.T.);
#13298=EDGE_CURVE('',#10535,#10530,#5566,.T.);
#13299=EDGE_CURVE('',#10536,#10537,#6820,.T.);
#13300=EDGE_CURVE('',#10538,#10536,#6821,.T.);
#13301=EDGE_CURVE('',#10538,#10539,#6822,.T.);
#13302=EDGE_CURVE('',#10539,#10537,#6823,.T.);
#13303=EDGE_CURVE('',#10537,#10540,#5567,.T.);
#13304=EDGE_CURVE('',#10540,#10539,#6824,.T.);
#13305=EDGE_CURVE('',#10540,#10541,#6825,.T.);
#13306=EDGE_CURVE('',#10541,#10538,#6826,.T.);
#13307=EDGE_CURVE('',#10541,#10536,#5568,.T.);
#13308=EDGE_CURVE('',#10542,#10543,#6827,.T.);
#13309=EDGE_CURVE('',#10544,#10542,#6828,.T.);
#13310=EDGE_CURVE('',#10544,#10545,#6829,.T.);
#13311=EDGE_CURVE('',#10545,#10543,#6830,.T.);
#13312=EDGE_CURVE('',#10543,#10546,#5569,.T.);
#13313=EDGE_CURVE('',#10546,#10545,#6831,.T.);
#13314=EDGE_CURVE('',#10546,#10547,#6832,.T.);
#13315=EDGE_CURVE('',#10547,#10544,#6833,.T.);
#13316=EDGE_CURVE('',#10547,#10542,#5570,.T.);
#13317=EDGE_CURVE('',#10548,#10549,#6834,.T.);
#13318=EDGE_CURVE('',#10550,#10548,#6835,.T.);
#13319=EDGE_CURVE('',#10550,#10551,#6836,.T.);
#13320=EDGE_CURVE('',#10551,#10549,#6837,.T.);
#13321=EDGE_CURVE('',#10549,#10552,#5571,.T.);
#13322=EDGE_CURVE('',#10552,#10551,#6838,.T.);
#13323=EDGE_CURVE('',#10552,#10553,#6839,.T.);
#13324=EDGE_CURVE('',#10553,#10550,#6840,.T.);
#13325=EDGE_CURVE('',#10553,#10548,#5572,.T.);
#13326=EDGE_CURVE('',#10554,#10555,#6841,.T.);
#13327=EDGE_CURVE('',#10556,#10554,#6842,.T.);
#13328=EDGE_CURVE('',#10556,#10557,#6843,.T.);
#13329=EDGE_CURVE('',#10557,#10555,#6844,.T.);
#13330=EDGE_CURVE('',#10555,#10558,#5573,.T.);
#13331=EDGE_CURVE('',#10558,#10557,#6845,.T.);
#13332=EDGE_CURVE('',#10558,#10559,#6846,.T.);
#13333=EDGE_CURVE('',#10559,#10556,#6847,.T.);
#13334=EDGE_CURVE('',#10559,#10554,#5574,.T.);
#13335=EDGE_CURVE('',#10560,#10561,#6848,.T.);
#13336=EDGE_CURVE('',#10562,#10560,#6849,.T.);
#13337=EDGE_CURVE('',#10562,#10563,#6850,.T.);
#13338=EDGE_CURVE('',#10563,#10561,#6851,.T.);
#13339=EDGE_CURVE('',#10561,#10564,#5575,.T.);
#13340=EDGE_CURVE('',#10564,#10563,#6852,.T.);
#13341=EDGE_CURVE('',#10564,#10565,#6853,.T.);
#13342=EDGE_CURVE('',#10565,#10562,#6854,.T.);
#13343=EDGE_CURVE('',#10565,#10560,#5576,.T.);
#13344=EDGE_CURVE('',#10566,#10567,#6855,.T.);
#13345=EDGE_CURVE('',#10568,#10566,#6856,.T.);
#13346=EDGE_CURVE('',#10568,#10569,#6857,.T.);
#13347=EDGE_CURVE('',#10569,#10567,#6858,.T.);
#13348=EDGE_CURVE('',#10567,#10570,#5577,.T.);
#13349=EDGE_CURVE('',#10570,#10569,#6859,.T.);
#13350=EDGE_CURVE('',#10570,#10571,#6860,.T.);
#13351=EDGE_CURVE('',#10571,#10568,#6861,.T.);
#13352=EDGE_CURVE('',#10571,#10566,#5578,.T.);
#13353=EDGE_CURVE('',#10572,#10573,#6862,.T.);
#13354=EDGE_CURVE('',#10574,#10572,#6863,.T.);
#13355=EDGE_CURVE('',#10574,#10575,#6864,.T.);
#13356=EDGE_CURVE('',#10575,#10573,#6865,.T.);
#13357=EDGE_CURVE('',#10573,#10576,#5579,.T.);
#13358=EDGE_CURVE('',#10576,#10575,#6866,.T.);
#13359=EDGE_CURVE('',#10576,#10577,#6867,.T.);
#13360=EDGE_CURVE('',#10577,#10574,#6868,.T.);
#13361=EDGE_CURVE('',#10577,#10572,#5580,.T.);
#13362=EDGE_CURVE('',#10578,#10579,#6869,.T.);
#13363=EDGE_CURVE('',#10580,#10578,#6870,.T.);
#13364=EDGE_CURVE('',#10580,#10581,#6871,.T.);
#13365=EDGE_CURVE('',#10581,#10579,#6872,.T.);
#13366=EDGE_CURVE('',#10579,#10582,#5581,.T.);
#13367=EDGE_CURVE('',#10582,#10581,#6873,.T.);
#13368=EDGE_CURVE('',#10582,#10583,#6874,.T.);
#13369=EDGE_CURVE('',#10583,#10580,#6875,.T.);
#13370=EDGE_CURVE('',#10583,#10578,#5582,.T.);
#13371=EDGE_CURVE('',#10584,#10585,#6876,.T.);
#13372=EDGE_CURVE('',#10586,#10584,#6877,.T.);
#13373=EDGE_CURVE('',#10586,#10587,#6878,.T.);
#13374=EDGE_CURVE('',#10587,#10585,#6879,.T.);
#13375=EDGE_CURVE('',#10585,#10588,#5583,.T.);
#13376=EDGE_CURVE('',#10588,#10587,#6880,.T.);
#13377=EDGE_CURVE('',#10588,#10589,#6881,.T.);
#13378=EDGE_CURVE('',#10589,#10586,#6882,.T.);
#13379=EDGE_CURVE('',#10589,#10584,#5584,.T.);
#13380=EDGE_CURVE('',#10590,#10591,#6883,.T.);
#13381=EDGE_CURVE('',#10592,#10590,#6884,.T.);
#13382=EDGE_CURVE('',#10592,#10593,#6885,.T.);
#13383=EDGE_CURVE('',#10593,#10591,#6886,.T.);
#13384=EDGE_CURVE('',#10591,#10594,#5585,.T.);
#13385=EDGE_CURVE('',#10594,#10593,#6887,.T.);
#13386=EDGE_CURVE('',#10594,#10595,#6888,.T.);
#13387=EDGE_CURVE('',#10595,#10592,#6889,.T.);
#13388=EDGE_CURVE('',#10595,#10590,#5586,.T.);
#13389=EDGE_CURVE('',#10596,#10597,#6890,.T.);
#13390=EDGE_CURVE('',#10598,#10596,#6891,.T.);
#13391=EDGE_CURVE('',#10598,#10599,#6892,.T.);
#13392=EDGE_CURVE('',#10599,#10597,#6893,.T.);
#13393=EDGE_CURVE('',#10597,#10600,#5587,.T.);
#13394=EDGE_CURVE('',#10600,#10599,#6894,.T.);
#13395=EDGE_CURVE('',#10600,#10601,#6895,.T.);
#13396=EDGE_CURVE('',#10601,#10598,#6896,.T.);
#13397=EDGE_CURVE('',#10601,#10596,#5588,.T.);
#13398=EDGE_CURVE('',#10602,#10602,#5589,.T.);
#13399=EDGE_CURVE('',#10390,#10602,#6897,.T.);
#13400=EDGE_CURVE('',#10603,#10603,#5590,.T.);
#13401=EDGE_CURVE('',#10604,#10604,#5591,.T.);
#13402=EDGE_CURVE('',#10604,#10603,#6898,.T.);
#13403=EDGE_CURVE('',#10605,#10605,#5592,.T.);
#13404=EDGE_CURVE('',#10605,#10526,#6899,.T.);
#13405=EDGE_CURVE('',#10529,#10604,#6900,.T.);
#13406=EDGE_CURVE('',#10606,#10606,#5593,.T.);
#13407=EDGE_CURVE('',#10606,#10605,#6901,.T.);
#13408=EDGE_CURVE('',#10607,#10608,#6902,.T.);
#13409=EDGE_CURVE('',#10607,#10609,#489,.T.);
#13410=EDGE_CURVE('',#10609,#10610,#5594,.T.);
#13411=EDGE_CURVE('',#10610,#10611,#6903,.T.);
#13412=EDGE_CURVE('',#10611,#10611,#5595,.T.);
#13413=EDGE_CURVE('',#10610,#10612,#5596,.T.);
#13414=EDGE_CURVE('',#10612,#10608,#490,.T.);
#13415=EDGE_CURVE('',#10613,#10614,#6904,.T.);
#13416=EDGE_CURVE('',#10613,#10607,#491,.T.);
#13417=EDGE_CURVE('',#10608,#10614,#492,.T.);
#13418=EDGE_CURVE('',#10615,#10616,#6905,.T.);
#13419=EDGE_CURVE('',#10615,#10613,#493,.T.);
#13420=EDGE_CURVE('',#10614,#10616,#494,.T.);
#13421=EDGE_CURVE('',#10617,#10618,#6906,.T.);
#13422=EDGE_CURVE('',#10617,#10615,#495,.T.);
#13423=EDGE_CURVE('',#10616,#10618,#496,.T.);
#13424=EDGE_CURVE('',#10619,#10620,#6907,.T.);
#13425=EDGE_CURVE('',#10619,#10617,#497,.T.);
#13426=EDGE_CURVE('',#10618,#10620,#498,.T.);
#13427=EDGE_CURVE('',#10621,#10622,#6908,.T.);
#13428=EDGE_CURVE('',#10621,#10619,#499,.T.);
#13429=EDGE_CURVE('',#10620,#10622,#500,.T.);
#13430=EDGE_CURVE('',#10623,#10624,#6909,.T.);
#13431=EDGE_CURVE('',#10623,#10621,#501,.T.);
#13432=EDGE_CURVE('',#10622,#10624,#502,.T.);
#13433=EDGE_CURVE('',#10625,#10626,#6910,.T.);
#13434=EDGE_CURVE('',#10625,#10623,#503,.T.);
#13435=EDGE_CURVE('',#10624,#10626,#504,.T.);
#13436=EDGE_CURVE('',#10627,#10628,#6911,.T.);
#13437=EDGE_CURVE('',#10627,#10625,#505,.T.);
#13438=EDGE_CURVE('',#10626,#10628,#506,.T.);
#13439=EDGE_CURVE('',#10629,#10630,#6912,.T.);
#13440=EDGE_CURVE('',#10629,#10627,#507,.T.);
#13441=EDGE_CURVE('',#10628,#10630,#508,.T.);
#13442=EDGE_CURVE('',#10631,#10632,#6913,.T.);
#13443=EDGE_CURVE('',#10631,#10629,#509,.T.);
#13444=EDGE_CURVE('',#10630,#10632,#510,.T.);
#13445=EDGE_CURVE('',#10633,#10634,#6914,.T.);
#13446=EDGE_CURVE('',#10633,#10631,#511,.T.);
#13447=EDGE_CURVE('',#10632,#10634,#512,.T.);
#13448=EDGE_CURVE('',#10635,#10636,#6915,.T.);
#13449=EDGE_CURVE('',#10635,#10633,#513,.T.);
#13450=EDGE_CURVE('',#10634,#10636,#514,.T.);
#13451=EDGE_CURVE('',#10637,#10638,#6916,.T.);
#13452=EDGE_CURVE('',#10637,#10635,#515,.T.);
#13453=EDGE_CURVE('',#10636,#10638,#516,.T.);
#13454=EDGE_CURVE('',#10639,#10640,#6917,.T.);
#13455=EDGE_CURVE('',#10639,#10641,#517,.T.);
#13456=EDGE_CURVE('',#10642,#10641,#5597,.T.);
#13457=EDGE_CURVE('',#10640,#10642,#518,.T.);
#13458=EDGE_CURVE('',#10643,#10644,#6918,.T.);
#13459=EDGE_CURVE('',#10643,#10639,#519,.T.);
#13460=EDGE_CURVE('',#10644,#10640,#520,.T.);
#13461=EDGE_CURVE('',#10645,#10646,#6919,.T.);
#13462=EDGE_CURVE('',#10645,#10643,#521,.T.);
#13463=EDGE_CURVE('',#10646,#10644,#522,.T.);
#13464=EDGE_CURVE('',#10647,#10648,#6920,.T.);
#13465=EDGE_CURVE('',#10647,#10645,#523,.T.);
#13466=EDGE_CURVE('',#10648,#10646,#524,.T.);
#13467=EDGE_CURVE('',#10649,#10650,#6921,.T.);
#13468=EDGE_CURVE('',#10649,#10647,#525,.T.);
#13469=EDGE_CURVE('',#10650,#10648,#526,.T.);
#13470=EDGE_CURVE('',#10651,#10652,#6922,.T.);
#13471=EDGE_CURVE('',#10651,#10649,#527,.T.);
#13472=EDGE_CURVE('',#10652,#10650,#528,.T.);
#13473=EDGE_CURVE('',#10653,#10654,#6923,.T.);
#13474=EDGE_CURVE('',#10653,#10651,#529,.T.);
#13475=EDGE_CURVE('',#10654,#10652,#530,.T.);
#13476=EDGE_CURVE('',#10655,#10656,#6924,.T.);
#13477=EDGE_CURVE('',#10655,#10653,#531,.T.);
#13478=EDGE_CURVE('',#10656,#10654,#532,.T.);
#13479=EDGE_CURVE('',#10657,#10658,#6925,.T.);
#13480=EDGE_CURVE('',#10657,#10655,#533,.T.);
#13481=EDGE_CURVE('',#10658,#10656,#534,.T.);
#13482=EDGE_CURVE('',#10659,#10660,#6926,.T.);
#13483=EDGE_CURVE('',#10659,#10657,#535,.T.);
#13484=EDGE_CURVE('',#10660,#10658,#536,.T.);
#13485=EDGE_CURVE('',#10661,#10662,#6927,.T.);
#13486=EDGE_CURVE('',#10661,#10659,#537,.T.);
#13487=EDGE_CURVE('',#10662,#10660,#538,.T.);
#13488=EDGE_CURVE('',#10663,#10664,#6928,.T.);
#13489=EDGE_CURVE('',#10663,#10661,#539,.T.);
#13490=EDGE_CURVE('',#10664,#10662,#540,.T.);
#13491=EDGE_CURVE('',#10665,#10666,#6929,.T.);
#13492=EDGE_CURVE('',#10665,#10663,#541,.T.);
#13493=EDGE_CURVE('',#10666,#10664,#542,.T.);
#13494=EDGE_CURVE('',#10667,#10668,#6930,.T.);
#13495=EDGE_CURVE('',#10667,#10665,#543,.T.);
#13496=EDGE_CURVE('',#10668,#10666,#544,.T.);
#13497=EDGE_CURVE('',#10669,#10670,#6931,.T.);
#13498=EDGE_CURVE('',#10669,#10667,#545,.T.);
#13499=EDGE_CURVE('',#10670,#10668,#546,.T.);
#13500=EDGE_CURVE('',#10641,#10671,#547,.T.);
#13501=EDGE_CURVE('',#10672,#10671,#5598,.T.);
#13502=EDGE_CURVE('',#10673,#10672,#5599,.T.);
#13503=EDGE_CURVE('',#10673,#10642,#548,.T.);
#13504=EDGE_CURVE('',#10638,#10673,#549,.T.);
#13505=EDGE_CURVE('',#10674,#10612,#550,.T.);
#13506=EDGE_CURVE('',#10674,#10670,#551,.T.);
#13507=EDGE_CURVE('',#10609,#10675,#552,.T.);
#13508=EDGE_CURVE('',#10675,#10674,#5600,.T.);
#13509=EDGE_CURVE('',#10675,#10669,#553,.T.);
#13510=EDGE_CURVE('',#10671,#10637,#554,.T.);
#13511=EDGE_CURVE('',#10676,#10677,#5601,.T.);
#13512=EDGE_CURVE('',#10676,#10678,#6932,.T.);
#13513=EDGE_CURVE('',#10678,#10677,#6933,.T.);
#13514=EDGE_CURVE('',#10677,#10679,#6934,.T.);
#13515=EDGE_CURVE('',#10678,#10680,#6935,.T.);
#13516=EDGE_CURVE('',#10679,#10680,#147,.T.);
#13517=EDGE_CURVE('',#10681,#10676,#6936,.T.);
#13518=EDGE_CURVE('',#10680,#10681,#148,.T.);
#13519=EDGE_CURVE('',#10682,#10683,#5602,.T.);
#13520=EDGE_CURVE('',#10682,#10684,#6937,.T.);
#13521=EDGE_CURVE('',#10684,#10683,#6938,.T.);
#13522=EDGE_CURVE('',#10683,#10685,#6939,.T.);
#13523=EDGE_CURVE('',#10684,#10686,#6940,.T.);
#13524=EDGE_CURVE('',#10685,#10686,#149,.T.);
#13525=EDGE_CURVE('',#10687,#10682,#6941,.T.);
#13526=EDGE_CURVE('',#10686,#10687,#150,.T.);
#13527=EDGE_CURVE('',#10688,#10689,#5603,.T.);
#13528=EDGE_CURVE('',#10688,#10690,#6942,.T.);
#13529=EDGE_CURVE('',#10690,#10689,#6943,.T.);
#13530=EDGE_CURVE('',#10689,#10691,#6944,.T.);
#13531=EDGE_CURVE('',#10690,#10692,#6945,.T.);
#13532=EDGE_CURVE('',#10691,#10692,#151,.T.);
#13533=EDGE_CURVE('',#10693,#10688,#6946,.T.);
#13534=EDGE_CURVE('',#10692,#10693,#152,.T.);
#13535=EDGE_CURVE('',#10694,#10695,#5604,.T.);
#13536=EDGE_CURVE('',#10694,#10696,#6947,.T.);
#13537=EDGE_CURVE('',#10696,#10695,#6948,.T.);
#13538=EDGE_CURVE('',#10695,#10697,#6949,.T.);
#13539=EDGE_CURVE('',#10696,#10698,#6950,.T.);
#13540=EDGE_CURVE('',#10697,#10698,#153,.T.);
#13541=EDGE_CURVE('',#10699,#10694,#6951,.T.);
#13542=EDGE_CURVE('',#10698,#10699,#154,.T.);
#13543=EDGE_CURVE('',#10700,#10701,#5605,.T.);
#13544=EDGE_CURVE('',#10700,#10702,#6952,.T.);
#13545=EDGE_CURVE('',#10702,#10701,#6953,.T.);
#13546=EDGE_CURVE('',#10701,#10703,#6954,.T.);
#13547=EDGE_CURVE('',#10702,#10704,#6955,.T.);
#13548=EDGE_CURVE('',#10703,#10704,#155,.T.);
#13549=EDGE_CURVE('',#10705,#10700,#6956,.T.);
#13550=EDGE_CURVE('',#10704,#10705,#156,.T.);
#13551=EDGE_CURVE('',#10706,#10707,#5606,.T.);
#13552=EDGE_CURVE('',#10706,#10708,#6957,.T.);
#13553=EDGE_CURVE('',#10708,#10707,#6958,.T.);
#13554=EDGE_CURVE('',#10707,#10709,#6959,.T.);
#13555=EDGE_CURVE('',#10708,#10710,#6960,.T.);
#13556=EDGE_CURVE('',#10709,#10710,#157,.T.);
#13557=EDGE_CURVE('',#10711,#10706,#6961,.T.);
#13558=EDGE_CURVE('',#10710,#10711,#158,.T.);
#13559=EDGE_CURVE('',#10712,#10713,#5607,.T.);
#13560=EDGE_CURVE('',#10712,#10714,#6962,.T.);
#13561=EDGE_CURVE('',#10714,#10713,#6963,.T.);
#13562=EDGE_CURVE('',#10713,#10715,#6964,.T.);
#13563=EDGE_CURVE('',#10714,#10716,#6965,.T.);
#13564=EDGE_CURVE('',#10715,#10716,#159,.T.);
#13565=EDGE_CURVE('',#10717,#10712,#6966,.T.);
#13566=EDGE_CURVE('',#10716,#10717,#160,.T.);
#13567=EDGE_CURVE('',#10718,#10719,#5608,.T.);
#13568=EDGE_CURVE('',#10718,#10720,#6967,.T.);
#13569=EDGE_CURVE('',#10720,#10719,#6968,.T.);
#13570=EDGE_CURVE('',#10719,#10721,#6969,.T.);
#13571=EDGE_CURVE('',#10720,#10722,#6970,.T.);
#13572=EDGE_CURVE('',#10721,#10722,#161,.T.);
#13573=EDGE_CURVE('',#10723,#10718,#6971,.T.);
#13574=EDGE_CURVE('',#10722,#10723,#162,.T.);
#13575=EDGE_CURVE('',#10724,#10725,#5609,.T.);
#13576=EDGE_CURVE('',#10724,#10726,#6972,.T.);
#13577=EDGE_CURVE('',#10726,#10725,#6973,.T.);
#13578=EDGE_CURVE('',#10725,#10727,#6974,.T.);
#13579=EDGE_CURVE('',#10726,#10728,#6975,.T.);
#13580=EDGE_CURVE('',#10727,#10728,#163,.T.);
#13581=EDGE_CURVE('',#10729,#10724,#6976,.T.);
#13582=EDGE_CURVE('',#10728,#10729,#164,.T.);
#13583=EDGE_CURVE('',#10730,#10731,#5610,.T.);
#13584=EDGE_CURVE('',#10730,#10732,#6977,.T.);
#13585=EDGE_CURVE('',#10732,#10731,#6978,.T.);
#13586=EDGE_CURVE('',#10731,#10733,#6979,.T.);
#13587=EDGE_CURVE('',#10732,#10734,#6980,.T.);
#13588=EDGE_CURVE('',#10733,#10734,#165,.T.);
#13589=EDGE_CURVE('',#10735,#10730,#6981,.T.);
#13590=EDGE_CURVE('',#10734,#10735,#166,.T.);
#13591=EDGE_CURVE('',#10736,#10737,#5611,.T.);
#13592=EDGE_CURVE('',#10736,#10738,#6982,.T.);
#13593=EDGE_CURVE('',#10738,#10737,#6983,.T.);
#13594=EDGE_CURVE('',#10737,#10739,#6984,.T.);
#13595=EDGE_CURVE('',#10738,#10740,#6985,.T.);
#13596=EDGE_CURVE('',#10739,#10740,#167,.T.);
#13597=EDGE_CURVE('',#10741,#10736,#6986,.T.);
#13598=EDGE_CURVE('',#10740,#10741,#168,.T.);
#13599=EDGE_CURVE('',#10742,#10743,#5612,.T.);
#13600=EDGE_CURVE('',#10742,#10744,#6987,.T.);
#13601=EDGE_CURVE('',#10744,#10743,#6988,.T.);
#13602=EDGE_CURVE('',#10743,#10745,#6989,.T.);
#13603=EDGE_CURVE('',#10744,#10746,#6990,.T.);
#13604=EDGE_CURVE('',#10745,#10746,#169,.T.);
#13605=EDGE_CURVE('',#10747,#10742,#6991,.T.);
#13606=EDGE_CURVE('',#10746,#10747,#170,.T.);
#13607=EDGE_CURVE('',#10748,#10749,#5613,.T.);
#13608=EDGE_CURVE('',#10748,#10750,#6992,.T.);
#13609=EDGE_CURVE('',#10750,#10749,#6993,.T.);
#13610=EDGE_CURVE('',#10749,#10751,#6994,.T.);
#13611=EDGE_CURVE('',#10750,#10752,#6995,.T.);
#13612=EDGE_CURVE('',#10751,#10752,#171,.T.);
#13613=EDGE_CURVE('',#10753,#10748,#6996,.T.);
#13614=EDGE_CURVE('',#10752,#10753,#172,.T.);
#13615=EDGE_CURVE('',#10754,#10755,#5614,.T.);
#13616=EDGE_CURVE('',#10754,#10756,#6997,.T.);
#13617=EDGE_CURVE('',#10756,#10755,#6998,.T.);
#13618=EDGE_CURVE('',#10755,#10757,#6999,.T.);
#13619=EDGE_CURVE('',#10756,#10758,#7000,.T.);
#13620=EDGE_CURVE('',#10757,#10758,#173,.T.);
#13621=EDGE_CURVE('',#10759,#10754,#7001,.T.);
#13622=EDGE_CURVE('',#10758,#10759,#174,.T.);
#13623=EDGE_CURVE('',#10760,#10761,#5615,.T.);
#13624=EDGE_CURVE('',#10760,#10762,#7002,.T.);
#13625=EDGE_CURVE('',#10762,#10761,#7003,.T.);
#13626=EDGE_CURVE('',#10761,#10763,#7004,.T.);
#13627=EDGE_CURVE('',#10762,#10764,#7005,.T.);
#13628=EDGE_CURVE('',#10763,#10764,#175,.T.);
#13629=EDGE_CURVE('',#10765,#10760,#7006,.T.);
#13630=EDGE_CURVE('',#10764,#10765,#176,.T.);
#13631=EDGE_CURVE('',#10766,#10767,#5616,.T.);
#13632=EDGE_CURVE('',#10766,#10768,#7007,.T.);
#13633=EDGE_CURVE('',#10768,#10767,#7008,.T.);
#13634=EDGE_CURVE('',#10767,#10769,#7009,.T.);
#13635=EDGE_CURVE('',#10768,#10770,#7010,.T.);
#13636=EDGE_CURVE('',#10769,#10770,#177,.T.);
#13637=EDGE_CURVE('',#10771,#10766,#7011,.T.);
#13638=EDGE_CURVE('',#10770,#10771,#178,.T.);
#13639=EDGE_CURVE('',#10772,#10773,#5617,.T.);
#13640=EDGE_CURVE('',#10772,#10774,#7012,.T.);
#13641=EDGE_CURVE('',#10774,#10773,#7013,.T.);
#13642=EDGE_CURVE('',#10773,#10775,#7014,.T.);
#13643=EDGE_CURVE('',#10774,#10776,#7015,.T.);
#13644=EDGE_CURVE('',#10775,#10776,#179,.T.);
#13645=EDGE_CURVE('',#10777,#10772,#7016,.T.);
#13646=EDGE_CURVE('',#10776,#10777,#180,.T.);
#13647=EDGE_CURVE('',#10778,#10779,#5618,.T.);
#13648=EDGE_CURVE('',#10778,#10780,#7017,.T.);
#13649=EDGE_CURVE('',#10780,#10781,#7018,.T.);
#13650=EDGE_CURVE('',#10779,#10781,#5619,.T.);
#13651=EDGE_CURVE('',#10781,#10782,#7019,.T.);
#13652=EDGE_CURVE('',#10780,#10783,#7020,.T.);
#13653=EDGE_CURVE('',#10782,#10783,#181,.T.);
#13654=EDGE_CURVE('',#10784,#10778,#7021,.T.);
#13655=EDGE_CURVE('',#10783,#10784,#182,.T.);
#13656=EDGE_CURVE('',#10785,#10786,#5620,.T.);
#13657=EDGE_CURVE('',#10785,#10787,#7022,.T.);
#13658=EDGE_CURVE('',#10787,#10786,#7023,.T.);
#13659=EDGE_CURVE('',#10786,#10788,#7024,.T.);
#13660=EDGE_CURVE('',#10787,#10789,#7025,.T.);
#13661=EDGE_CURVE('',#10788,#10789,#183,.T.);
#13662=EDGE_CURVE('',#10790,#10785,#7026,.T.);
#13663=EDGE_CURVE('',#10789,#10790,#184,.T.);
#13664=EDGE_CURVE('',#10791,#10792,#5621,.T.);
#13665=EDGE_CURVE('',#10791,#10793,#7027,.T.);
#13666=EDGE_CURVE('',#10793,#10792,#7028,.T.);
#13667=EDGE_CURVE('',#10792,#10794,#7029,.T.);
#13668=EDGE_CURVE('',#10793,#10795,#7030,.T.);
#13669=EDGE_CURVE('',#10794,#10795,#185,.T.);
#13670=EDGE_CURVE('',#10796,#10791,#7031,.T.);
#13671=EDGE_CURVE('',#10795,#10796,#186,.T.);
#13672=EDGE_CURVE('',#10797,#10798,#5622,.T.);
#13673=EDGE_CURVE('',#10797,#10799,#7032,.T.);
#13674=EDGE_CURVE('',#10799,#10798,#7033,.T.);
#13675=EDGE_CURVE('',#10798,#10800,#7034,.T.);
#13676=EDGE_CURVE('',#10799,#10801,#7035,.T.);
#13677=EDGE_CURVE('',#10800,#10801,#187,.T.);
#13678=EDGE_CURVE('',#10802,#10797,#7036,.T.);
#13679=EDGE_CURVE('',#10801,#10802,#188,.T.);
#13680=EDGE_CURVE('',#10803,#10804,#5623,.T.);
#13681=EDGE_CURVE('',#10803,#10805,#7037,.T.);
#13682=EDGE_CURVE('',#10805,#10804,#7038,.T.);
#13683=EDGE_CURVE('',#10804,#10806,#7039,.T.);
#13684=EDGE_CURVE('',#10805,#10807,#7040,.T.);
#13685=EDGE_CURVE('',#10806,#10807,#189,.T.);
#13686=EDGE_CURVE('',#10808,#10803,#7041,.T.);
#13687=EDGE_CURVE('',#10807,#10808,#190,.T.);
#13688=EDGE_CURVE('',#10809,#10810,#5624,.T.);
#13689=EDGE_CURVE('',#10809,#10811,#7042,.T.);
#13690=EDGE_CURVE('',#10811,#10810,#7043,.T.);
#13691=EDGE_CURVE('',#10810,#10812,#7044,.T.);
#13692=EDGE_CURVE('',#10811,#10813,#7045,.T.);
#13693=EDGE_CURVE('',#10812,#10813,#191,.T.);
#13694=EDGE_CURVE('',#10814,#10809,#7046,.T.);
#13695=EDGE_CURVE('',#10813,#10814,#192,.T.);
#13696=EDGE_CURVE('',#10815,#10816,#5625,.T.);
#13697=EDGE_CURVE('',#10815,#10817,#7047,.T.);
#13698=EDGE_CURVE('',#10817,#10816,#7048,.T.);
#13699=EDGE_CURVE('',#10816,#10818,#7049,.T.);
#13700=EDGE_CURVE('',#10817,#10819,#7050,.T.);
#13701=EDGE_CURVE('',#10818,#10819,#193,.T.);
#13702=EDGE_CURVE('',#10820,#10815,#7051,.T.);
#13703=EDGE_CURVE('',#10819,#10820,#194,.T.);
#13704=EDGE_CURVE('',#10821,#10822,#5626,.T.);
#13705=EDGE_CURVE('',#10821,#10823,#7052,.T.);
#13706=EDGE_CURVE('',#10823,#10822,#7053,.T.);
#13707=EDGE_CURVE('',#10822,#10824,#7054,.T.);
#13708=EDGE_CURVE('',#10823,#10825,#7055,.T.);
#13709=EDGE_CURVE('',#10824,#10825,#195,.T.);
#13710=EDGE_CURVE('',#10826,#10821,#7056,.T.);
#13711=EDGE_CURVE('',#10825,#10826,#196,.T.);
#13712=EDGE_CURVE('',#10827,#10828,#5627,.T.);
#13713=EDGE_CURVE('',#10827,#10829,#7057,.T.);
#13714=EDGE_CURVE('',#10829,#10828,#7058,.T.);
#13715=EDGE_CURVE('',#10828,#10830,#7059,.T.);
#13716=EDGE_CURVE('',#10829,#10831,#7060,.T.);
#13717=EDGE_CURVE('',#10830,#10831,#197,.T.);
#13718=EDGE_CURVE('',#10832,#10827,#7061,.T.);
#13719=EDGE_CURVE('',#10831,#10832,#198,.T.);
#13720=EDGE_CURVE('',#10833,#10834,#5628,.T.);
#13721=EDGE_CURVE('',#10833,#10835,#7062,.T.);
#13722=EDGE_CURVE('',#10835,#10834,#7063,.T.);
#13723=EDGE_CURVE('',#10834,#10836,#7064,.T.);
#13724=EDGE_CURVE('',#10835,#10837,#7065,.T.);
#13725=EDGE_CURVE('',#10836,#10837,#199,.T.);
#13726=EDGE_CURVE('',#10838,#10833,#7066,.T.);
#13727=EDGE_CURVE('',#10837,#10838,#200,.T.);
#13728=EDGE_CURVE('',#10839,#10840,#5629,.T.);
#13729=EDGE_CURVE('',#10839,#10841,#7067,.T.);
#13730=EDGE_CURVE('',#10841,#10840,#7068,.T.);
#13731=EDGE_CURVE('',#10840,#10842,#7069,.T.);
#13732=EDGE_CURVE('',#10841,#10843,#7070,.T.);
#13733=EDGE_CURVE('',#10842,#10843,#201,.T.);
#13734=EDGE_CURVE('',#10844,#10839,#7071,.T.);
#13735=EDGE_CURVE('',#10843,#10844,#202,.T.);
#13736=EDGE_CURVE('',#10845,#10846,#5630,.T.);
#13737=EDGE_CURVE('',#10845,#10847,#7072,.T.);
#13738=EDGE_CURVE('',#10847,#10846,#7073,.T.);
#13739=EDGE_CURVE('',#10846,#10848,#7074,.T.);
#13740=EDGE_CURVE('',#10847,#10849,#7075,.T.);
#13741=EDGE_CURVE('',#10848,#10849,#203,.T.);
#13742=EDGE_CURVE('',#10850,#10845,#7076,.T.);
#13743=EDGE_CURVE('',#10849,#10850,#204,.T.);
#13744=EDGE_CURVE('',#10851,#10852,#5631,.T.);
#13745=EDGE_CURVE('',#10851,#10853,#7077,.T.);
#13746=EDGE_CURVE('',#10853,#10852,#7078,.T.);
#13747=EDGE_CURVE('',#10852,#10854,#7079,.T.);
#13748=EDGE_CURVE('',#10853,#10855,#7080,.T.);
#13749=EDGE_CURVE('',#10854,#10855,#205,.T.);
#13750=EDGE_CURVE('',#10856,#10851,#7081,.T.);
#13751=EDGE_CURVE('',#10855,#10856,#206,.T.);
#13752=EDGE_CURVE('',#10857,#10858,#5632,.T.);
#13753=EDGE_CURVE('',#10857,#10859,#7082,.T.);
#13754=EDGE_CURVE('',#10859,#10858,#7083,.T.);
#13755=EDGE_CURVE('',#10858,#10860,#7084,.T.);
#13756=EDGE_CURVE('',#10859,#10861,#7085,.T.);
#13757=EDGE_CURVE('',#10860,#10861,#207,.T.);
#13758=EDGE_CURVE('',#10862,#10857,#7086,.T.);
#13759=EDGE_CURVE('',#10861,#10862,#208,.T.);
#13760=EDGE_CURVE('',#10863,#10864,#5633,.T.);
#13761=EDGE_CURVE('',#10863,#10865,#7087,.T.);
#13762=EDGE_CURVE('',#10865,#10864,#7088,.T.);
#13763=EDGE_CURVE('',#10864,#10866,#7089,.T.);
#13764=EDGE_CURVE('',#10865,#10867,#7090,.T.);
#13765=EDGE_CURVE('',#10866,#10867,#209,.T.);
#13766=EDGE_CURVE('',#10868,#10863,#7091,.T.);
#13767=EDGE_CURVE('',#10867,#10868,#210,.T.);
#13768=EDGE_CURVE('',#10869,#10870,#5634,.T.);
#13769=EDGE_CURVE('',#10869,#10871,#7092,.T.);
#13770=EDGE_CURVE('',#10871,#10870,#7093,.T.);
#13771=EDGE_CURVE('',#10870,#10872,#7094,.T.);
#13772=EDGE_CURVE('',#10871,#10873,#7095,.T.);
#13773=EDGE_CURVE('',#10872,#10873,#211,.T.);
#13774=EDGE_CURVE('',#10874,#10869,#7096,.T.);
#13775=EDGE_CURVE('',#10873,#10874,#212,.T.);
#13776=EDGE_CURVE('',#10875,#10876,#5635,.T.);
#13777=EDGE_CURVE('',#10875,#10877,#7097,.T.);
#13778=EDGE_CURVE('',#10877,#10876,#7098,.T.);
#13779=EDGE_CURVE('',#10876,#10878,#7099,.T.);
#13780=EDGE_CURVE('',#10877,#10879,#7100,.T.);
#13781=EDGE_CURVE('',#10878,#10879,#213,.T.);
#13782=EDGE_CURVE('',#10880,#10875,#7101,.T.);
#13783=EDGE_CURVE('',#10879,#10880,#214,.T.);
#13784=EDGE_CURVE('',#10881,#10882,#5636,.T.);
#13785=EDGE_CURVE('',#10881,#10883,#7102,.T.);
#13786=EDGE_CURVE('',#10883,#10882,#7103,.T.);
#13787=EDGE_CURVE('',#10882,#10884,#7104,.T.);
#13788=EDGE_CURVE('',#10883,#10885,#7105,.T.);
#13789=EDGE_CURVE('',#10884,#10885,#215,.T.);
#13790=EDGE_CURVE('',#10886,#10881,#7106,.T.);
#13791=EDGE_CURVE('',#10885,#10886,#216,.T.);
#13792=EDGE_CURVE('',#10687,#10679,#5637,.T.);
#13793=EDGE_CURVE('',#10693,#10685,#5638,.T.);
#13794=EDGE_CURVE('',#10699,#10691,#5639,.T.);
#13795=EDGE_CURVE('',#10705,#10697,#5640,.T.);
#13796=EDGE_CURVE('',#10711,#10703,#5641,.T.);
#13797=EDGE_CURVE('',#10717,#10709,#5642,.T.);
#13798=EDGE_CURVE('',#10723,#10715,#5643,.T.);
#13799=EDGE_CURVE('',#10729,#10721,#5644,.T.);
#13800=EDGE_CURVE('',#10735,#10727,#5645,.T.);
#13801=EDGE_CURVE('',#10741,#10733,#5646,.T.);
#13802=EDGE_CURVE('',#10747,#10739,#5647,.T.);
#13803=EDGE_CURVE('',#10753,#10745,#5648,.T.);
#13804=EDGE_CURVE('',#10759,#10751,#5649,.T.);
#13805=EDGE_CURVE('',#10765,#10757,#5650,.T.);
#13806=EDGE_CURVE('',#10771,#10763,#5651,.T.);
#13807=EDGE_CURVE('',#10777,#10769,#5652,.T.);
#13808=EDGE_CURVE('',#10784,#10775,#5653,.T.);
#13809=EDGE_CURVE('',#10779,#10887,#7107,.T.);
#13810=EDGE_CURVE('',#10887,#10887,#5654,.T.);
#13811=EDGE_CURVE('',#10790,#10782,#5655,.T.);
#13812=EDGE_CURVE('',#10796,#10788,#5656,.T.);
#13813=EDGE_CURVE('',#10802,#10794,#5657,.T.);
#13814=EDGE_CURVE('',#10808,#10800,#5658,.T.);
#13815=EDGE_CURVE('',#10814,#10806,#5659,.T.);
#13816=EDGE_CURVE('',#10820,#10812,#5660,.T.);
#13817=EDGE_CURVE('',#10826,#10818,#5661,.T.);
#13818=EDGE_CURVE('',#10832,#10824,#5662,.T.);
#13819=EDGE_CURVE('',#10838,#10830,#5663,.T.);
#13820=EDGE_CURVE('',#10844,#10836,#5664,.T.);
#13821=EDGE_CURVE('',#10850,#10842,#5665,.T.);
#13822=EDGE_CURVE('',#10856,#10848,#5666,.T.);
#13823=EDGE_CURVE('',#10862,#10854,#5667,.T.);
#13824=EDGE_CURVE('',#10868,#10860,#5668,.T.);
#13825=EDGE_CURVE('',#10874,#10866,#5669,.T.);
#13826=EDGE_CURVE('',#10880,#10872,#5670,.T.);
#13827=EDGE_CURVE('',#10886,#10878,#5671,.T.);
#13828=EDGE_CURVE('',#10888,#10884,#5672,.T.);
#13829=EDGE_CURVE('',#10888,#10889,#7108,.T.);
#13830=EDGE_CURVE('',#10889,#10890,#5673,.T.);
#13831=EDGE_CURVE('',#10890,#10891,#7109,.T.);
#13832=EDGE_CURVE('',#10681,#10891,#5674,.T.);
#13833=EDGE_CURVE('',#10892,#10890,#7110,.T.);
#13834=EDGE_CURVE('',#10892,#10893,#7111,.T.);
#13835=EDGE_CURVE('',#10891,#10893,#217,.T.);
#13836=EDGE_CURVE('',#10893,#10888,#218,.T.);
#13837=EDGE_CURVE('',#10889,#10892,#7112,.T.);
#13838=EDGE_CURVE('',#10894,#10894,#5675,.T.);
#13839=EDGE_CURVE('',#10894,#10783,#7113,.T.);
#13840=EDGE_CURVE('',#10895,#10896,#7114,.T.);
#13841=EDGE_CURVE('',#10896,#10896,#5676,.T.);
#13842=EDGE_CURVE('',#10897,#10898,#7115,.T.);
#13843=EDGE_CURVE('',#10897,#10899,#7116,.T.);
#13844=EDGE_CURVE('',#10899,#10900,#7117,.T.);
#13845=EDGE_CURVE('',#10898,#10900,#7118,.T.);
#13846=EDGE_CURVE('',#10901,#10897,#7119,.T.);
#13847=EDGE_CURVE('',#10901,#10902,#7120,.T.);
#13848=EDGE_CURVE('',#10902,#10899,#7121,.T.);
#13849=EDGE_CURVE('',#10903,#10901,#7122,.T.);
#13850=EDGE_CURVE('',#10903,#10904,#7123,.T.);
#13851=EDGE_CURVE('',#10904,#10902,#7124,.T.);
#13852=EDGE_CURVE('',#10905,#10903,#7125,.T.);
#13853=EDGE_CURVE('',#10905,#10906,#7126,.T.);
#13854=EDGE_CURVE('',#10906,#10904,#7127,.T.);
#13855=EDGE_CURVE('',#10907,#10905,#7128,.T.);
#13856=EDGE_CURVE('',#10907,#10908,#7129,.T.);
#13857=EDGE_CURVE('',#10908,#10906,#7130,.T.);
#13858=EDGE_CURVE('',#10898,#10907,#7131,.T.);
#13859=EDGE_CURVE('',#10900,#10908,#7132,.T.);
#13860=EDGE_CURVE('',#10909,#10909,#5677,.T.);
#13861=EDGE_CURVE('',#10611,#10909,#7133,.T.);
#13862=EDGE_CURVE('',#10671,#10673,#5678,.T.);
#13863=EDGE_CURVE('',#10910,#10910,#5679,.T.);
#13864=EDGE_CURVE('',#10910,#10672,#7134,.T.);
#13865=EDGE_CURVE('',#10911,#10912,#7135,.T.);
#13866=EDGE_CURVE('',#10911,#10913,#555,.T.);
#13867=EDGE_CURVE('',#10913,#10914,#5680,.T.);
#13868=EDGE_CURVE('',#10914,#10915,#7136,.T.);
#13869=EDGE_CURVE('',#10915,#10915,#5681,.T.);
#13870=EDGE_CURVE('',#10914,#10916,#5682,.T.);
#13871=EDGE_CURVE('',#10916,#10912,#556,.T.);
#13872=EDGE_CURVE('',#10917,#10918,#7137,.T.);
#13873=EDGE_CURVE('',#10917,#10911,#557,.T.);
#13874=EDGE_CURVE('',#10912,#10918,#558,.T.);
#13875=EDGE_CURVE('',#10919,#10920,#7138,.T.);
#13876=EDGE_CURVE('',#10919,#10917,#559,.T.);
#13877=EDGE_CURVE('',#10918,#10920,#560,.T.);
#13878=EDGE_CURVE('',#10921,#10922,#7139,.T.);
#13879=EDGE_CURVE('',#10921,#10919,#561,.T.);
#13880=EDGE_CURVE('',#10920,#10922,#562,.T.);
#13881=EDGE_CURVE('',#10923,#10924,#7140,.T.);
#13882=EDGE_CURVE('',#10923,#10921,#563,.T.);
#13883=EDGE_CURVE('',#10922,#10924,#564,.T.);
#13884=EDGE_CURVE('',#10925,#10926,#7141,.T.);
#13885=EDGE_CURVE('',#10925,#10923,#565,.T.);
#13886=EDGE_CURVE('',#10924,#10926,#566,.T.);
#13887=EDGE_CURVE('',#10927,#10928,#7142,.T.);
#13888=EDGE_CURVE('',#10927,#10925,#567,.T.);
#13889=EDGE_CURVE('',#10926,#10928,#568,.T.);
#13890=EDGE_CURVE('',#10929,#10930,#7143,.T.);
#13891=EDGE_CURVE('',#10929,#10927,#569,.T.);
#13892=EDGE_CURVE('',#10928,#10930,#570,.T.);
#13893=EDGE_CURVE('',#10931,#10932,#7144,.T.);
#13894=EDGE_CURVE('',#10931,#10929,#571,.T.);
#13895=EDGE_CURVE('',#10930,#10932,#572,.T.);
#13896=EDGE_CURVE('',#10933,#10934,#7145,.T.);
#13897=EDGE_CURVE('',#10933,#10931,#573,.T.);
#13898=EDGE_CURVE('',#10932,#10934,#574,.T.);
#13899=EDGE_CURVE('',#10935,#10936,#7146,.T.);
#13900=EDGE_CURVE('',#10935,#10933,#575,.T.);
#13901=EDGE_CURVE('',#10934,#10936,#576,.T.);
#13902=EDGE_CURVE('',#10937,#10938,#7147,.T.);
#13903=EDGE_CURVE('',#10937,#10935,#577,.T.);
#13904=EDGE_CURVE('',#10936,#10938,#578,.T.);
#13905=EDGE_CURVE('',#10939,#10940,#7148,.T.);
#13906=EDGE_CURVE('',#10939,#10937,#579,.T.);
#13907=EDGE_CURVE('',#10938,#10940,#580,.T.);
#13908=EDGE_CURVE('',#10941,#10942,#7149,.T.);
#13909=EDGE_CURVE('',#10941,#10939,#581,.T.);
#13910=EDGE_CURVE('',#10940,#10942,#582,.T.);
#13911=EDGE_CURVE('',#10943,#10944,#7150,.T.);
#13912=EDGE_CURVE('',#10943,#10941,#583,.T.);
#13913=EDGE_CURVE('',#10942,#10944,#584,.T.);
#13914=EDGE_CURVE('',#10945,#10946,#7151,.T.);
#13915=EDGE_CURVE('',#10945,#10943,#585,.T.);
#13916=EDGE_CURVE('',#10944,#10946,#586,.T.);
#13917=EDGE_CURVE('',#10947,#10948,#7152,.T.);
#13918=EDGE_CURVE('',#10947,#10945,#587,.T.);
#13919=EDGE_CURVE('',#10946,#10948,#588,.T.);
#13920=EDGE_CURVE('',#10949,#10950,#7153,.T.);
#13921=EDGE_CURVE('',#10949,#10947,#589,.T.);
#13922=EDGE_CURVE('',#10948,#10950,#590,.T.);
#13923=EDGE_CURVE('',#10951,#10952,#7154,.T.);
#13924=EDGE_CURVE('',#10951,#10949,#591,.T.);
#13925=EDGE_CURVE('',#10950,#10952,#592,.T.);
#13926=EDGE_CURVE('',#10953,#10954,#7155,.T.);
#13927=EDGE_CURVE('',#10953,#10951,#593,.T.);
#13928=EDGE_CURVE('',#10952,#10954,#594,.T.);
#13929=EDGE_CURVE('',#10955,#10956,#7156,.T.);
#13930=EDGE_CURVE('',#10955,#10953,#595,.T.);
#13931=EDGE_CURVE('',#10954,#10956,#596,.T.);
#13932=EDGE_CURVE('',#10957,#10958,#7157,.T.);
#13933=EDGE_CURVE('',#10957,#10955,#597,.T.);
#13934=EDGE_CURVE('',#10956,#10958,#598,.T.);
#13935=EDGE_CURVE('',#10959,#10960,#7158,.T.);
#13936=EDGE_CURVE('',#10959,#10957,#599,.T.);
#13937=EDGE_CURVE('',#10958,#10960,#600,.T.);
#13938=EDGE_CURVE('',#10961,#10962,#7159,.T.);
#13939=EDGE_CURVE('',#10961,#10959,#601,.T.);
#13940=EDGE_CURVE('',#10960,#10962,#602,.T.);
#13941=EDGE_CURVE('',#10963,#10964,#7160,.T.);
#13942=EDGE_CURVE('',#10963,#10961,#603,.T.);
#13943=EDGE_CURVE('',#10962,#10964,#604,.T.);
#13944=EDGE_CURVE('',#10965,#10966,#7161,.T.);
#13945=EDGE_CURVE('',#10965,#10963,#605,.T.);
#13946=EDGE_CURVE('',#10964,#10966,#606,.T.);
#13947=EDGE_CURVE('',#10967,#10968,#7162,.T.);
#13948=EDGE_CURVE('',#10967,#10965,#607,.T.);
#13949=EDGE_CURVE('',#10966,#10968,#608,.T.);
#13950=EDGE_CURVE('',#10969,#10970,#7163,.T.);
#13951=EDGE_CURVE('',#10969,#10967,#609,.T.);
#13952=EDGE_CURVE('',#10968,#10970,#610,.T.);
#13953=EDGE_CURVE('',#10971,#10972,#7164,.T.);
#13954=EDGE_CURVE('',#10971,#10969,#611,.T.);
#13955=EDGE_CURVE('',#10970,#10972,#612,.T.);
#13956=EDGE_CURVE('',#10973,#10974,#7165,.T.);
#13957=EDGE_CURVE('',#10973,#10971,#613,.T.);
#13958=EDGE_CURVE('',#10972,#10974,#614,.T.);
#13959=EDGE_CURVE('',#10975,#10976,#7166,.T.);
#13960=EDGE_CURVE('',#10975,#10973,#615,.T.);
#13961=EDGE_CURVE('',#10974,#10976,#616,.T.);
#13962=EDGE_CURVE('',#10977,#10978,#7167,.T.);
#13963=EDGE_CURVE('',#10977,#10975,#617,.T.);
#13964=EDGE_CURVE('',#10976,#10978,#618,.T.);
#13965=EDGE_CURVE('',#10979,#10980,#7168,.T.);
#13966=EDGE_CURVE('',#10979,#10977,#619,.T.);
#13967=EDGE_CURVE('',#10978,#10980,#620,.T.);
#13968=EDGE_CURVE('',#10981,#10982,#7169,.T.);
#13969=EDGE_CURVE('',#10981,#10979,#621,.T.);
#13970=EDGE_CURVE('',#10980,#10982,#622,.T.);
#13971=EDGE_CURVE('',#10983,#10984,#7170,.T.);
#13972=EDGE_CURVE('',#10983,#10981,#623,.T.);
#13973=EDGE_CURVE('',#10982,#10984,#624,.T.);
#13974=EDGE_CURVE('',#10985,#10986,#7171,.T.);
#13975=EDGE_CURVE('',#10985,#10983,#625,.T.);
#13976=EDGE_CURVE('',#10984,#10986,#626,.T.);
#13977=EDGE_CURVE('',#10987,#10988,#7172,.T.);
#13978=EDGE_CURVE('',#10987,#10985,#627,.T.);
#13979=EDGE_CURVE('',#10986,#10988,#628,.T.);
#13980=EDGE_CURVE('',#10989,#10990,#7173,.T.);
#13981=EDGE_CURVE('',#10989,#10987,#629,.T.);
#13982=EDGE_CURVE('',#10988,#10990,#630,.T.);
#13983=EDGE_CURVE('',#10991,#10992,#7174,.T.);
#13984=EDGE_CURVE('',#10991,#10989,#631,.T.);
#13985=EDGE_CURVE('',#10990,#10992,#632,.T.);
#13986=EDGE_CURVE('',#10993,#10994,#7175,.T.);
#13987=EDGE_CURVE('',#10993,#10991,#633,.T.);
#13988=EDGE_CURVE('',#10992,#10994,#634,.T.);
#13989=EDGE_CURVE('',#10995,#10996,#7176,.T.);
#13990=EDGE_CURVE('',#10995,#10993,#635,.T.);
#13991=EDGE_CURVE('',#10994,#10996,#636,.T.);
#13992=EDGE_CURVE('',#10997,#10998,#7177,.T.);
#13993=EDGE_CURVE('',#10997,#10995,#637,.T.);
#13994=EDGE_CURVE('',#10996,#10998,#638,.T.);
#13995=EDGE_CURVE('',#10999,#11000,#7178,.T.);
#13996=EDGE_CURVE('',#10999,#10997,#639,.T.);
#13997=EDGE_CURVE('',#10998,#11000,#640,.T.);
#13998=EDGE_CURVE('',#11001,#11002,#7179,.T.);
#13999=EDGE_CURVE('',#11001,#10999,#641,.T.);
#14000=EDGE_CURVE('',#11000,#11002,#642,.T.);
#14001=EDGE_CURVE('',#11003,#11004,#7180,.T.);
#14002=EDGE_CURVE('',#11003,#11001,#643,.T.);
#14003=EDGE_CURVE('',#11002,#11004,#644,.T.);
#14004=EDGE_CURVE('',#11005,#11006,#7181,.T.);
#14005=EDGE_CURVE('',#11005,#11003,#645,.T.);
#14006=EDGE_CURVE('',#11004,#11006,#646,.T.);
#14007=EDGE_CURVE('',#11007,#11008,#7182,.T.);
#14008=EDGE_CURVE('',#11007,#11005,#647,.T.);
#14009=EDGE_CURVE('',#11006,#11008,#648,.T.);
#14010=EDGE_CURVE('',#11009,#11010,#7183,.T.);
#14011=EDGE_CURVE('',#11009,#11007,#649,.T.);
#14012=EDGE_CURVE('',#11008,#11010,#650,.T.);
#14013=EDGE_CURVE('',#11011,#11012,#7184,.T.);
#14014=EDGE_CURVE('',#11011,#11009,#651,.T.);
#14015=EDGE_CURVE('',#11010,#11012,#652,.T.);
#14016=EDGE_CURVE('',#11013,#11014,#7185,.T.);
#14017=EDGE_CURVE('',#11013,#11011,#653,.T.);
#14018=EDGE_CURVE('',#11012,#11014,#654,.T.);
#14019=EDGE_CURVE('',#11015,#11016,#7186,.T.);
#14020=EDGE_CURVE('',#11015,#11013,#655,.T.);
#14021=EDGE_CURVE('',#11014,#11016,#656,.T.);
#14022=EDGE_CURVE('',#11017,#11018,#7187,.T.);
#14023=EDGE_CURVE('',#11017,#11015,#657,.T.);
#14024=EDGE_CURVE('',#11016,#11018,#658,.T.);
#14025=EDGE_CURVE('',#11019,#11020,#7188,.T.);
#14026=EDGE_CURVE('',#11019,#11017,#659,.T.);
#14027=EDGE_CURVE('',#11018,#11020,#660,.T.);
#14028=EDGE_CURVE('',#11021,#11022,#7189,.T.);
#14029=EDGE_CURVE('',#11021,#11019,#661,.T.);
#14030=EDGE_CURVE('',#11020,#11022,#662,.T.);
#14031=EDGE_CURVE('',#11023,#11024,#7190,.T.);
#14032=EDGE_CURVE('',#11023,#11021,#663,.T.);
#14033=EDGE_CURVE('',#11022,#11024,#664,.T.);
#14034=EDGE_CURVE('',#11025,#11026,#7191,.T.);
#14035=EDGE_CURVE('',#11025,#11023,#665,.T.);
#14036=EDGE_CURVE('',#11024,#11026,#666,.T.);
#14037=EDGE_CURVE('',#11027,#11028,#7192,.T.);
#14038=EDGE_CURVE('',#11027,#11025,#667,.T.);
#14039=EDGE_CURVE('',#11026,#11028,#668,.T.);
#14040=EDGE_CURVE('',#11029,#11030,#7193,.T.);
#14041=EDGE_CURVE('',#11029,#11027,#669,.T.);
#14042=EDGE_CURVE('',#11028,#11030,#670,.T.);
#14043=EDGE_CURVE('',#11031,#11032,#7194,.T.);
#14044=EDGE_CURVE('',#11031,#11033,#671,.T.);
#14045=EDGE_CURVE('',#11034,#11033,#5683,.T.);
#14046=EDGE_CURVE('',#11032,#11034,#672,.T.);
#14047=EDGE_CURVE('',#11035,#11036,#7195,.T.);
#14048=EDGE_CURVE('',#11035,#11031,#673,.T.);
#14049=EDGE_CURVE('',#11036,#11032,#674,.T.);
#14050=EDGE_CURVE('',#11037,#11038,#7196,.T.);
#14051=EDGE_CURVE('',#11037,#11035,#675,.T.);
#14052=EDGE_CURVE('',#11038,#11036,#676,.T.);
#14053=EDGE_CURVE('',#11039,#11040,#7197,.T.);
#14054=EDGE_CURVE('',#11039,#11037,#677,.T.);
#14055=EDGE_CURVE('',#11040,#11038,#678,.T.);
#14056=EDGE_CURVE('',#11041,#11042,#7198,.T.);
#14057=EDGE_CURVE('',#11041,#11039,#679,.T.);
#14058=EDGE_CURVE('',#11042,#11040,#680,.T.);
#14059=EDGE_CURVE('',#11043,#11044,#7199,.T.);
#14060=EDGE_CURVE('',#11043,#11041,#681,.T.);
#14061=EDGE_CURVE('',#11044,#11042,#682,.T.);
#14062=EDGE_CURVE('',#11045,#11046,#7200,.T.);
#14063=EDGE_CURVE('',#11045,#11043,#683,.T.);
#14064=EDGE_CURVE('',#11046,#11044,#684,.T.);
#14065=EDGE_CURVE('',#11047,#11048,#7201,.T.);
#14066=EDGE_CURVE('',#11047,#11045,#685,.T.);
#14067=EDGE_CURVE('',#11048,#11046,#686,.T.);
#14068=EDGE_CURVE('',#11049,#11050,#7202,.T.);
#14069=EDGE_CURVE('',#11049,#11047,#687,.T.);
#14070=EDGE_CURVE('',#11050,#11048,#688,.T.);
#14071=EDGE_CURVE('',#11051,#11052,#7203,.T.);
#14072=EDGE_CURVE('',#11051,#11049,#689,.T.);
#14073=EDGE_CURVE('',#11052,#11050,#690,.T.);
#14074=EDGE_CURVE('',#11053,#11054,#7204,.T.);
#14075=EDGE_CURVE('',#11053,#11051,#691,.T.);
#14076=EDGE_CURVE('',#11054,#11052,#692,.T.);
#14077=EDGE_CURVE('',#11055,#11056,#7205,.T.);
#14078=EDGE_CURVE('',#11055,#11053,#693,.T.);
#14079=EDGE_CURVE('',#11056,#11054,#694,.T.);
#14080=EDGE_CURVE('',#11057,#11058,#7206,.T.);
#14081=EDGE_CURVE('',#11057,#11055,#695,.T.);
#14082=EDGE_CURVE('',#11058,#11056,#696,.T.);
#14083=EDGE_CURVE('',#11059,#11060,#7207,.T.);
#14084=EDGE_CURVE('',#11059,#11057,#697,.T.);
#14085=EDGE_CURVE('',#11060,#11058,#698,.T.);
#14086=EDGE_CURVE('',#11061,#11062,#7208,.T.);
#14087=EDGE_CURVE('',#11061,#11059,#699,.T.);
#14088=EDGE_CURVE('',#11062,#11060,#700,.T.);
#14089=EDGE_CURVE('',#11063,#11064,#7209,.T.);
#14090=EDGE_CURVE('',#11063,#11061,#701,.T.);
#14091=EDGE_CURVE('',#11064,#11062,#702,.T.);
#14092=EDGE_CURVE('',#11065,#11066,#7210,.T.);
#14093=EDGE_CURVE('',#11065,#11063,#703,.T.);
#14094=EDGE_CURVE('',#11066,#11064,#704,.T.);
#14095=EDGE_CURVE('',#11067,#11068,#7211,.T.);
#14096=EDGE_CURVE('',#11067,#11065,#705,.T.);
#14097=EDGE_CURVE('',#11068,#11066,#706,.T.);
#14098=EDGE_CURVE('',#11069,#11070,#7212,.T.);
#14099=EDGE_CURVE('',#11069,#11067,#707,.T.);
#14100=EDGE_CURVE('',#11070,#11068,#708,.T.);
#14101=EDGE_CURVE('',#11071,#11072,#7213,.T.);
#14102=EDGE_CURVE('',#11071,#11069,#709,.T.);
#14103=EDGE_CURVE('',#11072,#11070,#710,.T.);
#14104=EDGE_CURVE('',#11073,#11074,#7214,.T.);
#14105=EDGE_CURVE('',#11073,#11071,#711,.T.);
#14106=EDGE_CURVE('',#11074,#11072,#712,.T.);
#14107=EDGE_CURVE('',#11075,#11076,#7215,.T.);
#14108=EDGE_CURVE('',#11075,#11073,#713,.T.);
#14109=EDGE_CURVE('',#11076,#11074,#714,.T.);
#14110=EDGE_CURVE('',#11077,#11078,#7216,.T.);
#14111=EDGE_CURVE('',#11077,#11075,#715,.T.);
#14112=EDGE_CURVE('',#11078,#11076,#716,.T.);
#14113=EDGE_CURVE('',#11079,#11080,#7217,.T.);
#14114=EDGE_CURVE('',#11079,#11077,#717,.T.);
#14115=EDGE_CURVE('',#11080,#11078,#718,.T.);
#14116=EDGE_CURVE('',#11081,#11082,#7218,.T.);
#14117=EDGE_CURVE('',#11081,#11079,#719,.T.);
#14118=EDGE_CURVE('',#11082,#11080,#720,.T.);
#14119=EDGE_CURVE('',#11083,#11084,#7219,.T.);
#14120=EDGE_CURVE('',#11083,#11081,#721,.T.);
#14121=EDGE_CURVE('',#11084,#11082,#722,.T.);
#14122=EDGE_CURVE('',#11085,#11086,#7220,.T.);
#14123=EDGE_CURVE('',#11085,#11083,#723,.T.);
#14124=EDGE_CURVE('',#11086,#11084,#724,.T.);
#14125=EDGE_CURVE('',#11087,#11088,#7221,.T.);
#14126=EDGE_CURVE('',#11087,#11085,#725,.T.);
#14127=EDGE_CURVE('',#11088,#11086,#726,.T.);
#14128=EDGE_CURVE('',#11089,#11090,#7222,.T.);
#14129=EDGE_CURVE('',#11089,#11087,#727,.T.);
#14130=EDGE_CURVE('',#11090,#11088,#728,.T.);
#14131=EDGE_CURVE('',#11091,#11092,#7223,.T.);
#14132=EDGE_CURVE('',#11091,#11089,#729,.T.);
#14133=EDGE_CURVE('',#11092,#11090,#730,.T.);
#14134=EDGE_CURVE('',#11093,#11094,#7224,.T.);
#14135=EDGE_CURVE('',#11093,#11091,#731,.T.);
#14136=EDGE_CURVE('',#11094,#11092,#732,.T.);
#14137=EDGE_CURVE('',#11095,#11096,#7225,.T.);
#14138=EDGE_CURVE('',#11095,#11093,#733,.T.);
#14139=EDGE_CURVE('',#11096,#11094,#734,.T.);
#14140=EDGE_CURVE('',#11097,#11098,#7226,.T.);
#14141=EDGE_CURVE('',#11097,#11095,#735,.T.);
#14142=EDGE_CURVE('',#11098,#11096,#736,.T.);
#14143=EDGE_CURVE('',#11099,#11100,#7227,.T.);
#14144=EDGE_CURVE('',#11099,#11097,#737,.T.);
#14145=EDGE_CURVE('',#11100,#11098,#738,.T.);
#14146=EDGE_CURVE('',#11101,#11102,#7228,.T.);
#14147=EDGE_CURVE('',#11101,#11099,#739,.T.);
#14148=EDGE_CURVE('',#11102,#11100,#740,.T.);
#14149=EDGE_CURVE('',#11103,#11104,#7229,.T.);
#14150=EDGE_CURVE('',#11103,#11101,#741,.T.);
#14151=EDGE_CURVE('',#11104,#11102,#742,.T.);
#14152=EDGE_CURVE('',#11105,#11106,#7230,.T.);
#14153=EDGE_CURVE('',#11105,#11103,#743,.T.);
#14154=EDGE_CURVE('',#11106,#11104,#744,.T.);
#14155=EDGE_CURVE('',#11107,#11108,#7231,.T.);
#14156=EDGE_CURVE('',#11107,#11105,#745,.T.);
#14157=EDGE_CURVE('',#11108,#11106,#746,.T.);
#14158=EDGE_CURVE('',#11109,#11110,#7232,.T.);
#14159=EDGE_CURVE('',#11109,#11107,#747,.T.);
#14160=EDGE_CURVE('',#11110,#11108,#748,.T.);
#14161=EDGE_CURVE('',#11111,#11112,#7233,.T.);
#14162=EDGE_CURVE('',#11111,#11109,#749,.T.);
#14163=EDGE_CURVE('',#11112,#11110,#750,.T.);
#14164=EDGE_CURVE('',#11113,#11114,#7234,.T.);
#14165=EDGE_CURVE('',#11113,#11111,#751,.T.);
#14166=EDGE_CURVE('',#11114,#11112,#752,.T.);
#14167=EDGE_CURVE('',#11115,#11116,#7235,.T.);
#14168=EDGE_CURVE('',#11115,#11113,#753,.T.);
#14169=EDGE_CURVE('',#11116,#11114,#754,.T.);
#14170=EDGE_CURVE('',#11117,#11118,#7236,.T.);
#14171=EDGE_CURVE('',#11117,#11115,#755,.T.);
#14172=EDGE_CURVE('',#11118,#11116,#756,.T.);
#14173=EDGE_CURVE('',#11119,#11120,#7237,.T.);
#14174=EDGE_CURVE('',#11119,#11117,#757,.T.);
#14175=EDGE_CURVE('',#11120,#11118,#758,.T.);
#14176=EDGE_CURVE('',#11121,#11122,#7238,.T.);
#14177=EDGE_CURVE('',#11121,#11119,#759,.T.);
#14178=EDGE_CURVE('',#11122,#11120,#760,.T.);
#14179=EDGE_CURVE('',#11123,#11124,#7239,.T.);
#14180=EDGE_CURVE('',#11123,#11121,#761,.T.);
#14181=EDGE_CURVE('',#11124,#11122,#762,.T.);
#14182=EDGE_CURVE('',#11125,#11126,#7240,.T.);
#14183=EDGE_CURVE('',#11125,#11123,#763,.T.);
#14184=EDGE_CURVE('',#11126,#11124,#764,.T.);
#14185=EDGE_CURVE('',#11127,#11128,#7241,.T.);
#14186=EDGE_CURVE('',#11127,#11125,#765,.T.);
#14187=EDGE_CURVE('',#11128,#11126,#766,.T.);
#14188=EDGE_CURVE('',#11129,#11130,#7242,.T.);
#14189=EDGE_CURVE('',#11129,#11127,#767,.T.);
#14190=EDGE_CURVE('',#11130,#11128,#768,.T.);
#14191=EDGE_CURVE('',#11131,#11132,#7243,.T.);
#14192=EDGE_CURVE('',#11131,#11129,#769,.T.);
#14193=EDGE_CURVE('',#11132,#11130,#770,.T.);
#14194=EDGE_CURVE('',#11133,#11134,#7244,.T.);
#14195=EDGE_CURVE('',#11133,#11131,#771,.T.);
#14196=EDGE_CURVE('',#11134,#11132,#772,.T.);
#14197=EDGE_CURVE('',#11135,#11136,#7245,.T.);
#14198=EDGE_CURVE('',#11135,#11133,#773,.T.);
#14199=EDGE_CURVE('',#11136,#11134,#774,.T.);
#14200=EDGE_CURVE('',#11137,#11138,#7246,.T.);
#14201=EDGE_CURVE('',#11137,#11135,#775,.T.);
#14202=EDGE_CURVE('',#11138,#11136,#776,.T.);
#14203=EDGE_CURVE('',#11139,#11140,#7247,.T.);
#14204=EDGE_CURVE('',#11139,#11137,#777,.T.);
#14205=EDGE_CURVE('',#11140,#11138,#778,.T.);
#14206=EDGE_CURVE('',#11141,#11142,#7248,.T.);
#14207=EDGE_CURVE('',#11141,#11139,#779,.T.);
#14208=EDGE_CURVE('',#11142,#11140,#780,.T.);
#14209=EDGE_CURVE('',#11143,#11144,#7249,.T.);
#14210=EDGE_CURVE('',#11143,#11141,#781,.T.);
#14211=EDGE_CURVE('',#11144,#11142,#782,.T.);
#14212=EDGE_CURVE('',#11145,#11146,#7250,.T.);
#14213=EDGE_CURVE('',#11145,#11143,#783,.T.);
#14214=EDGE_CURVE('',#11146,#11144,#784,.T.);
#14215=EDGE_CURVE('',#11147,#11148,#7251,.T.);
#14216=EDGE_CURVE('',#11147,#11145,#785,.T.);
#14217=EDGE_CURVE('',#11148,#11146,#786,.T.);
#14218=EDGE_CURVE('',#11149,#11150,#7252,.T.);
#14219=EDGE_CURVE('',#11149,#11147,#787,.T.);
#14220=EDGE_CURVE('',#11150,#11148,#788,.T.);
#14221=EDGE_CURVE('',#11033,#11151,#789,.T.);
#14222=EDGE_CURVE('',#11152,#11151,#5684,.T.);
#14223=EDGE_CURVE('',#11153,#11152,#5685,.T.);
#14224=EDGE_CURVE('',#11153,#11034,#790,.T.);
#14225=EDGE_CURVE('',#11030,#11153,#791,.T.);
#14226=EDGE_CURVE('',#11154,#10916,#792,.T.);
#14227=EDGE_CURVE('',#11154,#11150,#793,.T.);
#14228=EDGE_CURVE('',#10913,#11155,#794,.T.);
#14229=EDGE_CURVE('',#11155,#11154,#5686,.T.);
#14230=EDGE_CURVE('',#11155,#11149,#795,.T.);
#14231=EDGE_CURVE('',#11151,#11029,#796,.T.);
#14232=EDGE_CURVE('',#11156,#11157,#5687,.T.);
#14233=EDGE_CURVE('',#11156,#11158,#7253,.T.);
#14234=EDGE_CURVE('',#11158,#11157,#7254,.T.);
#14235=EDGE_CURVE('',#11157,#11159,#7255,.T.);
#14236=EDGE_CURVE('',#11158,#11160,#7256,.T.);
#14237=EDGE_CURVE('',#11159,#11160,#219,.T.);
#14238=EDGE_CURVE('',#11161,#11156,#7257,.T.);
#14239=EDGE_CURVE('',#11160,#11161,#220,.T.);
#14240=EDGE_CURVE('',#11162,#11163,#5688,.T.);
#14241=EDGE_CURVE('',#11162,#11164,#7258,.T.);
#14242=EDGE_CURVE('',#11164,#11163,#7259,.T.);
#14243=EDGE_CURVE('',#11163,#11165,#7260,.T.);
#14244=EDGE_CURVE('',#11164,#11166,#7261,.T.);
#14245=EDGE_CURVE('',#11165,#11166,#221,.T.);
#14246=EDGE_CURVE('',#11167,#11162,#7262,.T.);
#14247=EDGE_CURVE('',#11166,#11167,#222,.T.);
#14248=EDGE_CURVE('',#11168,#11169,#5689,.T.);
#14249=EDGE_CURVE('',#11168,#11170,#7263,.T.);
#14250=EDGE_CURVE('',#11170,#11169,#7264,.T.);
#14251=EDGE_CURVE('',#11169,#11171,#7265,.T.);
#14252=EDGE_CURVE('',#11170,#11172,#7266,.T.);
#14253=EDGE_CURVE('',#11171,#11172,#223,.T.);
#14254=EDGE_CURVE('',#11173,#11168,#7267,.T.);
#14255=EDGE_CURVE('',#11172,#11173,#224,.T.);
#14256=EDGE_CURVE('',#11174,#11175,#5690,.T.);
#14257=EDGE_CURVE('',#11174,#11176,#7268,.T.);
#14258=EDGE_CURVE('',#11176,#11175,#7269,.T.);
#14259=EDGE_CURVE('',#11175,#11177,#7270,.T.);
#14260=EDGE_CURVE('',#11176,#11178,#7271,.T.);
#14261=EDGE_CURVE('',#11177,#11178,#225,.T.);
#14262=EDGE_CURVE('',#11179,#11174,#7272,.T.);
#14263=EDGE_CURVE('',#11178,#11179,#226,.T.);
#14264=EDGE_CURVE('',#11180,#11181,#5691,.T.);
#14265=EDGE_CURVE('',#11180,#11182,#7273,.T.);
#14266=EDGE_CURVE('',#11182,#11181,#7274,.T.);
#14267=EDGE_CURVE('',#11181,#11183,#7275,.T.);
#14268=EDGE_CURVE('',#11182,#11184,#7276,.T.);
#14269=EDGE_CURVE('',#11183,#11184,#227,.T.);
#14270=EDGE_CURVE('',#11185,#11180,#7277,.T.);
#14271=EDGE_CURVE('',#11184,#11185,#228,.T.);
#14272=EDGE_CURVE('',#11186,#11187,#5692,.T.);
#14273=EDGE_CURVE('',#11186,#11188,#7278,.T.);
#14274=EDGE_CURVE('',#11188,#11187,#7279,.T.);
#14275=EDGE_CURVE('',#11187,#11189,#7280,.T.);
#14276=EDGE_CURVE('',#11188,#11190,#7281,.T.);
#14277=EDGE_CURVE('',#11189,#11190,#229,.T.);
#14278=EDGE_CURVE('',#11191,#11186,#7282,.T.);
#14279=EDGE_CURVE('',#11190,#11191,#230,.T.);
#14280=EDGE_CURVE('',#11192,#11193,#5693,.T.);
#14281=EDGE_CURVE('',#11192,#11194,#7283,.T.);
#14282=EDGE_CURVE('',#11194,#11193,#7284,.T.);
#14283=EDGE_CURVE('',#11193,#11195,#7285,.T.);
#14284=EDGE_CURVE('',#11194,#11196,#7286,.T.);
#14285=EDGE_CURVE('',#11195,#11196,#231,.T.);
#14286=EDGE_CURVE('',#11197,#11192,#7287,.T.);
#14287=EDGE_CURVE('',#11196,#11197,#232,.T.);
#14288=EDGE_CURVE('',#11198,#11199,#5694,.T.);
#14289=EDGE_CURVE('',#11198,#11200,#7288,.T.);
#14290=EDGE_CURVE('',#11200,#11199,#7289,.T.);
#14291=EDGE_CURVE('',#11199,#11201,#7290,.T.);
#14292=EDGE_CURVE('',#11200,#11202,#7291,.T.);
#14293=EDGE_CURVE('',#11201,#11202,#233,.T.);
#14294=EDGE_CURVE('',#11203,#11198,#7292,.T.);
#14295=EDGE_CURVE('',#11202,#11203,#234,.T.);
#14296=EDGE_CURVE('',#11204,#11205,#5695,.T.);
#14297=EDGE_CURVE('',#11204,#11206,#7293,.T.);
#14298=EDGE_CURVE('',#11206,#11205,#7294,.T.);
#14299=EDGE_CURVE('',#11205,#11207,#7295,.T.);
#14300=EDGE_CURVE('',#11206,#11208,#7296,.T.);
#14301=EDGE_CURVE('',#11207,#11208,#235,.T.);
#14302=EDGE_CURVE('',#11209,#11204,#7297,.T.);
#14303=EDGE_CURVE('',#11208,#11209,#236,.T.);
#14304=EDGE_CURVE('',#11210,#11211,#5696,.T.);
#14305=EDGE_CURVE('',#11210,#11212,#7298,.T.);
#14306=EDGE_CURVE('',#11212,#11211,#7299,.T.);
#14307=EDGE_CURVE('',#11211,#11213,#7300,.T.);
#14308=EDGE_CURVE('',#11212,#11214,#7301,.T.);
#14309=EDGE_CURVE('',#11213,#11214,#237,.T.);
#14310=EDGE_CURVE('',#11215,#11210,#7302,.T.);
#14311=EDGE_CURVE('',#11214,#11215,#238,.T.);
#14312=EDGE_CURVE('',#11216,#11217,#5697,.T.);
#14313=EDGE_CURVE('',#11216,#11218,#7303,.T.);
#14314=EDGE_CURVE('',#11218,#11217,#7304,.T.);
#14315=EDGE_CURVE('',#11217,#11219,#7305,.T.);
#14316=EDGE_CURVE('',#11218,#11220,#7306,.T.);
#14317=EDGE_CURVE('',#11219,#11220,#239,.T.);
#14318=EDGE_CURVE('',#11221,#11216,#7307,.T.);
#14319=EDGE_CURVE('',#11220,#11221,#240,.T.);
#14320=EDGE_CURVE('',#11222,#11223,#5698,.T.);
#14321=EDGE_CURVE('',#11222,#11224,#7308,.T.);
#14322=EDGE_CURVE('',#11224,#11223,#7309,.T.);
#14323=EDGE_CURVE('',#11223,#11225,#7310,.T.);
#14324=EDGE_CURVE('',#11224,#11226,#7311,.T.);
#14325=EDGE_CURVE('',#11225,#11226,#241,.T.);
#14326=EDGE_CURVE('',#11227,#11222,#7312,.T.);
#14327=EDGE_CURVE('',#11226,#11227,#242,.T.);
#14328=EDGE_CURVE('',#11228,#11229,#5699,.T.);
#14329=EDGE_CURVE('',#11228,#11230,#7313,.T.);
#14330=EDGE_CURVE('',#11230,#11229,#7314,.T.);
#14331=EDGE_CURVE('',#11229,#11231,#7315,.T.);
#14332=EDGE_CURVE('',#11230,#11232,#7316,.T.);
#14333=EDGE_CURVE('',#11231,#11232,#243,.T.);
#14334=EDGE_CURVE('',#11233,#11228,#7317,.T.);
#14335=EDGE_CURVE('',#11232,#11233,#244,.T.);
#14336=EDGE_CURVE('',#11234,#11235,#5700,.T.);
#14337=EDGE_CURVE('',#11234,#11236,#7318,.T.);
#14338=EDGE_CURVE('',#11236,#11235,#7319,.T.);
#14339=EDGE_CURVE('',#11235,#11237,#7320,.T.);
#14340=EDGE_CURVE('',#11236,#11238,#7321,.T.);
#14341=EDGE_CURVE('',#11237,#11238,#245,.T.);
#14342=EDGE_CURVE('',#11239,#11234,#7322,.T.);
#14343=EDGE_CURVE('',#11238,#11239,#246,.T.);
#14344=EDGE_CURVE('',#11240,#11241,#5701,.T.);
#14345=EDGE_CURVE('',#11240,#11242,#7323,.T.);
#14346=EDGE_CURVE('',#11242,#11241,#7324,.T.);
#14347=EDGE_CURVE('',#11241,#11243,#7325,.T.);
#14348=EDGE_CURVE('',#11242,#11244,#7326,.T.);
#14349=EDGE_CURVE('',#11243,#11244,#247,.T.);
#14350=EDGE_CURVE('',#11245,#11240,#7327,.T.);
#14351=EDGE_CURVE('',#11244,#11245,#248,.T.);
#14352=EDGE_CURVE('',#11246,#11247,#5702,.T.);
#14353=EDGE_CURVE('',#11246,#11248,#7328,.T.);
#14354=EDGE_CURVE('',#11248,#11247,#7329,.T.);
#14355=EDGE_CURVE('',#11247,#11249,#7330,.T.);
#14356=EDGE_CURVE('',#11248,#11250,#7331,.T.);
#14357=EDGE_CURVE('',#11249,#11250,#249,.T.);
#14358=EDGE_CURVE('',#11251,#11246,#7332,.T.);
#14359=EDGE_CURVE('',#11250,#11251,#250,.T.);
#14360=EDGE_CURVE('',#11252,#11253,#5703,.T.);
#14361=EDGE_CURVE('',#11252,#11254,#7333,.T.);
#14362=EDGE_CURVE('',#11254,#11253,#7334,.T.);
#14363=EDGE_CURVE('',#11253,#11255,#7335,.T.);
#14364=EDGE_CURVE('',#11254,#11256,#7336,.T.);
#14365=EDGE_CURVE('',#11255,#11256,#251,.T.);
#14366=EDGE_CURVE('',#11257,#11252,#7337,.T.);
#14367=EDGE_CURVE('',#11256,#11257,#252,.T.);
#14368=EDGE_CURVE('',#11258,#11259,#5704,.T.);
#14369=EDGE_CURVE('',#11258,#11260,#7338,.T.);
#14370=EDGE_CURVE('',#11260,#11261,#7339,.T.);
#14371=EDGE_CURVE('',#11259,#11261,#5705,.T.);
#14372=EDGE_CURVE('',#11261,#11262,#7340,.T.);
#14373=EDGE_CURVE('',#11260,#11263,#7341,.T.);
#14374=EDGE_CURVE('',#11262,#11263,#253,.T.);
#14375=EDGE_CURVE('',#11264,#11258,#7342,.T.);
#14376=EDGE_CURVE('',#11263,#11264,#254,.T.);
#14377=EDGE_CURVE('',#11265,#11266,#5706,.T.);
#14378=EDGE_CURVE('',#11265,#11267,#7343,.T.);
#14379=EDGE_CURVE('',#11267,#11266,#7344,.T.);
#14380=EDGE_CURVE('',#11266,#11268,#7345,.T.);
#14381=EDGE_CURVE('',#11267,#11269,#7346,.T.);
#14382=EDGE_CURVE('',#11268,#11269,#255,.T.);
#14383=EDGE_CURVE('',#11270,#11265,#7347,.T.);
#14384=EDGE_CURVE('',#11269,#11270,#256,.T.);
#14385=EDGE_CURVE('',#11271,#11272,#5707,.T.);
#14386=EDGE_CURVE('',#11271,#11273,#7348,.T.);
#14387=EDGE_CURVE('',#11273,#11272,#7349,.T.);
#14388=EDGE_CURVE('',#11272,#11274,#7350,.T.);
#14389=EDGE_CURVE('',#11273,#11275,#7351,.T.);
#14390=EDGE_CURVE('',#11274,#11275,#257,.T.);
#14391=EDGE_CURVE('',#11276,#11271,#7352,.T.);
#14392=EDGE_CURVE('',#11275,#11276,#258,.T.);
#14393=EDGE_CURVE('',#11277,#11278,#5708,.T.);
#14394=EDGE_CURVE('',#11277,#11279,#7353,.T.);
#14395=EDGE_CURVE('',#11279,#11278,#7354,.T.);
#14396=EDGE_CURVE('',#11278,#11280,#7355,.T.);
#14397=EDGE_CURVE('',#11279,#11281,#7356,.T.);
#14398=EDGE_CURVE('',#11280,#11281,#259,.T.);
#14399=EDGE_CURVE('',#11282,#11277,#7357,.T.);
#14400=EDGE_CURVE('',#11281,#11282,#260,.T.);
#14401=EDGE_CURVE('',#11283,#11284,#5709,.T.);
#14402=EDGE_CURVE('',#11283,#11285,#7358,.T.);
#14403=EDGE_CURVE('',#11285,#11284,#7359,.T.);
#14404=EDGE_CURVE('',#11284,#11286,#7360,.T.);
#14405=EDGE_CURVE('',#11285,#11287,#7361,.T.);
#14406=EDGE_CURVE('',#11286,#11287,#261,.T.);
#14407=EDGE_CURVE('',#11288,#11283,#7362,.T.);
#14408=EDGE_CURVE('',#11287,#11288,#262,.T.);
#14409=EDGE_CURVE('',#11289,#11290,#5710,.T.);
#14410=EDGE_CURVE('',#11289,#11291,#7363,.T.);
#14411=EDGE_CURVE('',#11291,#11290,#7364,.T.);
#14412=EDGE_CURVE('',#11290,#11292,#7365,.T.);
#14413=EDGE_CURVE('',#11291,#11293,#7366,.T.);
#14414=EDGE_CURVE('',#11292,#11293,#263,.T.);
#14415=EDGE_CURVE('',#11294,#11289,#7367,.T.);
#14416=EDGE_CURVE('',#11293,#11294,#264,.T.);
#14417=EDGE_CURVE('',#11295,#11296,#5711,.T.);
#14418=EDGE_CURVE('',#11295,#11297,#7368,.T.);
#14419=EDGE_CURVE('',#11297,#11296,#7369,.T.);
#14420=EDGE_CURVE('',#11296,#11298,#7370,.T.);
#14421=EDGE_CURVE('',#11297,#11299,#7371,.T.);
#14422=EDGE_CURVE('',#11298,#11299,#265,.T.);
#14423=EDGE_CURVE('',#11300,#11295,#7372,.T.);
#14424=EDGE_CURVE('',#11299,#11300,#266,.T.);
#14425=EDGE_CURVE('',#11301,#11302,#5712,.T.);
#14426=EDGE_CURVE('',#11301,#11303,#7373,.T.);
#14427=EDGE_CURVE('',#11303,#11302,#7374,.T.);
#14428=EDGE_CURVE('',#11302,#11304,#7375,.T.);
#14429=EDGE_CURVE('',#11303,#11305,#7376,.T.);
#14430=EDGE_CURVE('',#11304,#11305,#267,.T.);
#14431=EDGE_CURVE('',#11306,#11301,#7377,.T.);
#14432=EDGE_CURVE('',#11305,#11306,#268,.T.);
#14433=EDGE_CURVE('',#11307,#11308,#5713,.T.);
#14434=EDGE_CURVE('',#11307,#11309,#7378,.T.);
#14435=EDGE_CURVE('',#11309,#11308,#7379,.T.);
#14436=EDGE_CURVE('',#11308,#11310,#7380,.T.);
#14437=EDGE_CURVE('',#11309,#11311,#7381,.T.);
#14438=EDGE_CURVE('',#11310,#11311,#269,.T.);
#14439=EDGE_CURVE('',#11312,#11307,#7382,.T.);
#14440=EDGE_CURVE('',#11311,#11312,#270,.T.);
#14441=EDGE_CURVE('',#11313,#11314,#5714,.T.);
#14442=EDGE_CURVE('',#11313,#11315,#7383,.T.);
#14443=EDGE_CURVE('',#11315,#11314,#7384,.T.);
#14444=EDGE_CURVE('',#11314,#11316,#7385,.T.);
#14445=EDGE_CURVE('',#11315,#11317,#7386,.T.);
#14446=EDGE_CURVE('',#11316,#11317,#271,.T.);
#14447=EDGE_CURVE('',#11318,#11313,#7387,.T.);
#14448=EDGE_CURVE('',#11317,#11318,#272,.T.);
#14449=EDGE_CURVE('',#11319,#11320,#5715,.T.);
#14450=EDGE_CURVE('',#11319,#11321,#7388,.T.);
#14451=EDGE_CURVE('',#11321,#11320,#7389,.T.);
#14452=EDGE_CURVE('',#11320,#11322,#7390,.T.);
#14453=EDGE_CURVE('',#11321,#11323,#7391,.T.);
#14454=EDGE_CURVE('',#11322,#11323,#273,.T.);
#14455=EDGE_CURVE('',#11324,#11319,#7392,.T.);
#14456=EDGE_CURVE('',#11323,#11324,#274,.T.);
#14457=EDGE_CURVE('',#11325,#11326,#5716,.T.);
#14458=EDGE_CURVE('',#11325,#11327,#7393,.T.);
#14459=EDGE_CURVE('',#11327,#11326,#7394,.T.);
#14460=EDGE_CURVE('',#11326,#11328,#7395,.T.);
#14461=EDGE_CURVE('',#11327,#11329,#7396,.T.);
#14462=EDGE_CURVE('',#11328,#11329,#275,.T.);
#14463=EDGE_CURVE('',#11330,#11325,#7397,.T.);
#14464=EDGE_CURVE('',#11329,#11330,#276,.T.);
#14465=EDGE_CURVE('',#11331,#11332,#5717,.T.);
#14466=EDGE_CURVE('',#11331,#11333,#7398,.T.);
#14467=EDGE_CURVE('',#11333,#11332,#7399,.T.);
#14468=EDGE_CURVE('',#11332,#11334,#7400,.T.);
#14469=EDGE_CURVE('',#11333,#11335,#7401,.T.);
#14470=EDGE_CURVE('',#11334,#11335,#277,.T.);
#14471=EDGE_CURVE('',#11336,#11331,#7402,.T.);
#14472=EDGE_CURVE('',#11335,#11336,#278,.T.);
#14473=EDGE_CURVE('',#11337,#11338,#5718,.T.);
#14474=EDGE_CURVE('',#11337,#11339,#7403,.T.);
#14475=EDGE_CURVE('',#11339,#11338,#7404,.T.);
#14476=EDGE_CURVE('',#11338,#11340,#7405,.T.);
#14477=EDGE_CURVE('',#11339,#11341,#7406,.T.);
#14478=EDGE_CURVE('',#11340,#11341,#279,.T.);
#14479=EDGE_CURVE('',#11342,#11337,#7407,.T.);
#14480=EDGE_CURVE('',#11341,#11342,#280,.T.);
#14481=EDGE_CURVE('',#11343,#11344,#5719,.T.);
#14482=EDGE_CURVE('',#11343,#11345,#7408,.T.);
#14483=EDGE_CURVE('',#11345,#11344,#7409,.T.);
#14484=EDGE_CURVE('',#11344,#11346,#7410,.T.);
#14485=EDGE_CURVE('',#11345,#11347,#7411,.T.);
#14486=EDGE_CURVE('',#11346,#11347,#281,.T.);
#14487=EDGE_CURVE('',#11348,#11343,#7412,.T.);
#14488=EDGE_CURVE('',#11347,#11348,#282,.T.);
#14489=EDGE_CURVE('',#11349,#11350,#5720,.T.);
#14490=EDGE_CURVE('',#11349,#11351,#7413,.T.);
#14491=EDGE_CURVE('',#11351,#11350,#7414,.T.);
#14492=EDGE_CURVE('',#11350,#11352,#7415,.T.);
#14493=EDGE_CURVE('',#11351,#11353,#7416,.T.);
#14494=EDGE_CURVE('',#11352,#11353,#283,.T.);
#14495=EDGE_CURVE('',#11354,#11349,#7417,.T.);
#14496=EDGE_CURVE('',#11353,#11354,#284,.T.);
#14497=EDGE_CURVE('',#11355,#11356,#5721,.T.);
#14498=EDGE_CURVE('',#11355,#11357,#7418,.T.);
#14499=EDGE_CURVE('',#11357,#11356,#7419,.T.);
#14500=EDGE_CURVE('',#11356,#11358,#7420,.T.);
#14501=EDGE_CURVE('',#11357,#11359,#7421,.T.);
#14502=EDGE_CURVE('',#11358,#11359,#285,.T.);
#14503=EDGE_CURVE('',#11360,#11355,#7422,.T.);
#14504=EDGE_CURVE('',#11359,#11360,#286,.T.);
#14505=EDGE_CURVE('',#11361,#11362,#5722,.T.);
#14506=EDGE_CURVE('',#11361,#11363,#7423,.T.);
#14507=EDGE_CURVE('',#11363,#11362,#7424,.T.);
#14508=EDGE_CURVE('',#11362,#11364,#7425,.T.);
#14509=EDGE_CURVE('',#11363,#11365,#7426,.T.);
#14510=EDGE_CURVE('',#11364,#11365,#287,.T.);
#14511=EDGE_CURVE('',#11366,#11361,#7427,.T.);
#14512=EDGE_CURVE('',#11365,#11366,#288,.T.);
#14513=EDGE_CURVE('',#11167,#11159,#5723,.T.);
#14514=EDGE_CURVE('',#11173,#11165,#5724,.T.);
#14515=EDGE_CURVE('',#11179,#11171,#5725,.T.);
#14516=EDGE_CURVE('',#11185,#11177,#5726,.T.);
#14517=EDGE_CURVE('',#11191,#11183,#5727,.T.);
#14518=EDGE_CURVE('',#11197,#11189,#5728,.T.);
#14519=EDGE_CURVE('',#11203,#11195,#5729,.T.);
#14520=EDGE_CURVE('',#11209,#11201,#5730,.T.);
#14521=EDGE_CURVE('',#11215,#11207,#5731,.T.);
#14522=EDGE_CURVE('',#11221,#11213,#5732,.T.);
#14523=EDGE_CURVE('',#11227,#11219,#5733,.T.);
#14524=EDGE_CURVE('',#11233,#11225,#5734,.T.);
#14525=EDGE_CURVE('',#11239,#11231,#5735,.T.);
#14526=EDGE_CURVE('',#11245,#11237,#5736,.T.);
#14527=EDGE_CURVE('',#11251,#11243,#5737,.T.);
#14528=EDGE_CURVE('',#11257,#11249,#5738,.T.);
#14529=EDGE_CURVE('',#11264,#11255,#5739,.T.);
#14530=EDGE_CURVE('',#11259,#11367,#7428,.T.);
#14531=EDGE_CURVE('',#11367,#11367,#5740,.T.);
#14532=EDGE_CURVE('',#11270,#11262,#5741,.T.);
#14533=EDGE_CURVE('',#11276,#11268,#5742,.T.);
#14534=EDGE_CURVE('',#11282,#11274,#5743,.T.);
#14535=EDGE_CURVE('',#11288,#11280,#5744,.T.);
#14536=EDGE_CURVE('',#11294,#11286,#5745,.T.);
#14537=EDGE_CURVE('',#11300,#11292,#5746,.T.);
#14538=EDGE_CURVE('',#11306,#11298,#5747,.T.);
#14539=EDGE_CURVE('',#11312,#11304,#5748,.T.);
#14540=EDGE_CURVE('',#11318,#11310,#5749,.T.);
#14541=EDGE_CURVE('',#11324,#11316,#5750,.T.);
#14542=EDGE_CURVE('',#11330,#11322,#5751,.T.);
#14543=EDGE_CURVE('',#11336,#11328,#5752,.T.);
#14544=EDGE_CURVE('',#11342,#11334,#5753,.T.);
#14545=EDGE_CURVE('',#11348,#11340,#5754,.T.);
#14546=EDGE_CURVE('',#11354,#11346,#5755,.T.);
#14547=EDGE_CURVE('',#11360,#11352,#5756,.T.);
#14548=EDGE_CURVE('',#11366,#11358,#5757,.T.);
#14549=EDGE_CURVE('',#11368,#11364,#5758,.T.);
#14550=EDGE_CURVE('',#11368,#11369,#7429,.T.);
#14551=EDGE_CURVE('',#11369,#11370,#5759,.T.);
#14552=EDGE_CURVE('',#11370,#11371,#7430,.T.);
#14553=EDGE_CURVE('',#11161,#11371,#5760,.T.);
#14554=EDGE_CURVE('',#11372,#11370,#7431,.T.);
#14555=EDGE_CURVE('',#11372,#11373,#7432,.T.);
#14556=EDGE_CURVE('',#11371,#11373,#289,.T.);
#14557=EDGE_CURVE('',#11373,#11368,#290,.T.);
#14558=EDGE_CURVE('',#11369,#11372,#7433,.T.);
#14559=EDGE_CURVE('',#11374,#11374,#5761,.T.);
#14560=EDGE_CURVE('',#11374,#11263,#7434,.T.);
#14561=EDGE_CURVE('',#11375,#11376,#7435,.T.);
#14562=EDGE_CURVE('',#11376,#11376,#5762,.T.);
#14563=EDGE_CURVE('',#11377,#11378,#7436,.T.);
#14564=EDGE_CURVE('',#11377,#11379,#7437,.T.);
#14565=EDGE_CURVE('',#11379,#11380,#7438,.T.);
#14566=EDGE_CURVE('',#11378,#11380,#7439,.T.);
#14567=EDGE_CURVE('',#11381,#11377,#7440,.T.);
#14568=EDGE_CURVE('',#11381,#11382,#7441,.T.);
#14569=EDGE_CURVE('',#11382,#11379,#7442,.T.);
#14570=EDGE_CURVE('',#11383,#11381,#7443,.T.);
#14571=EDGE_CURVE('',#11383,#11384,#7444,.T.);
#14572=EDGE_CURVE('',#11384,#11382,#7445,.T.);
#14573=EDGE_CURVE('',#11385,#11383,#7446,.T.);
#14574=EDGE_CURVE('',#11385,#11386,#7447,.T.);
#14575=EDGE_CURVE('',#11386,#11384,#7448,.T.);
#14576=EDGE_CURVE('',#11387,#11385,#7449,.T.);
#14577=EDGE_CURVE('',#11387,#11388,#7450,.T.);
#14578=EDGE_CURVE('',#11388,#11386,#7451,.T.);
#14579=EDGE_CURVE('',#11378,#11387,#7452,.T.);
#14580=EDGE_CURVE('',#11380,#11388,#7453,.T.);
#14581=EDGE_CURVE('',#11389,#11389,#5763,.T.);
#14582=EDGE_CURVE('',#10915,#11389,#7454,.T.);
#14583=EDGE_CURVE('',#11151,#11153,#5764,.T.);
#14584=EDGE_CURVE('',#11390,#11390,#5765,.T.);
#14585=EDGE_CURVE('',#11390,#11152,#7455,.T.);
#14586=EDGE_CURVE('',#11391,#11392,#7456,.T.);
#14587=EDGE_CURVE('',#11391,#11393,#797,.T.);
#14588=EDGE_CURVE('',#11393,#11394,#5766,.T.);
#14589=EDGE_CURVE('',#11394,#11395,#7457,.T.);
#14590=EDGE_CURVE('',#11395,#11395,#5767,.T.);
#14591=EDGE_CURVE('',#11394,#11396,#5768,.T.);
#14592=EDGE_CURVE('',#11396,#11392,#798,.T.);
#14593=EDGE_CURVE('',#11397,#11398,#7458,.T.);
#14594=EDGE_CURVE('',#11397,#11391,#799,.T.);
#14595=EDGE_CURVE('',#11392,#11398,#800,.T.);
#14596=EDGE_CURVE('',#11399,#11400,#7459,.T.);
#14597=EDGE_CURVE('',#11399,#11397,#801,.T.);
#14598=EDGE_CURVE('',#11398,#11400,#802,.T.);
#14599=EDGE_CURVE('',#11401,#11402,#7460,.T.);
#14600=EDGE_CURVE('',#11401,#11399,#803,.T.);
#14601=EDGE_CURVE('',#11400,#11402,#804,.T.);
#14602=EDGE_CURVE('',#11403,#11404,#7461,.T.);
#14603=EDGE_CURVE('',#11403,#11401,#805,.T.);
#14604=EDGE_CURVE('',#11402,#11404,#806,.T.);
#14605=EDGE_CURVE('',#11405,#11406,#7462,.T.);
#14606=EDGE_CURVE('',#11405,#11403,#807,.T.);
#14607=EDGE_CURVE('',#11404,#11406,#808,.T.);
#14608=EDGE_CURVE('',#11407,#11408,#7463,.T.);
#14609=EDGE_CURVE('',#11407,#11405,#809,.T.);
#14610=EDGE_CURVE('',#11406,#11408,#810,.T.);
#14611=EDGE_CURVE('',#11409,#11410,#7464,.T.);
#14612=EDGE_CURVE('',#11409,#11407,#811,.T.);
#14613=EDGE_CURVE('',#11408,#11410,#812,.T.);
#14614=EDGE_CURVE('',#11411,#11412,#7465,.T.);
#14615=EDGE_CURVE('',#11411,#11409,#813,.T.);
#14616=EDGE_CURVE('',#11410,#11412,#814,.T.);
#14617=EDGE_CURVE('',#11413,#11414,#7466,.T.);
#14618=EDGE_CURVE('',#11413,#11411,#815,.T.);
#14619=EDGE_CURVE('',#11412,#11414,#816,.T.);
#14620=EDGE_CURVE('',#11415,#11416,#7467,.T.);
#14621=EDGE_CURVE('',#11415,#11413,#817,.T.);
#14622=EDGE_CURVE('',#11414,#11416,#818,.T.);
#14623=EDGE_CURVE('',#11417,#11418,#7468,.T.);
#14624=EDGE_CURVE('',#11417,#11415,#819,.T.);
#14625=EDGE_CURVE('',#11416,#11418,#820,.T.);
#14626=EDGE_CURVE('',#11419,#11420,#7469,.T.);
#14627=EDGE_CURVE('',#11419,#11417,#821,.T.);
#14628=EDGE_CURVE('',#11418,#11420,#822,.T.);
#14629=EDGE_CURVE('',#11421,#11422,#7470,.T.);
#14630=EDGE_CURVE('',#11421,#11419,#823,.T.);
#14631=EDGE_CURVE('',#11420,#11422,#824,.T.);
#14632=EDGE_CURVE('',#11423,#11424,#7471,.T.);
#14633=EDGE_CURVE('',#11423,#11421,#825,.T.);
#14634=EDGE_CURVE('',#11422,#11424,#826,.T.);
#14635=EDGE_CURVE('',#11425,#11426,#7472,.T.);
#14636=EDGE_CURVE('',#11425,#11423,#827,.T.);
#14637=EDGE_CURVE('',#11424,#11426,#828,.T.);
#14638=EDGE_CURVE('',#11427,#11428,#7473,.T.);
#14639=EDGE_CURVE('',#11427,#11425,#829,.T.);
#14640=EDGE_CURVE('',#11426,#11428,#830,.T.);
#14641=EDGE_CURVE('',#11429,#11430,#7474,.T.);
#14642=EDGE_CURVE('',#11429,#11427,#831,.T.);
#14643=EDGE_CURVE('',#11428,#11430,#832,.T.);
#14644=EDGE_CURVE('',#11431,#11432,#7475,.T.);
#14645=EDGE_CURVE('',#11431,#11433,#833,.T.);
#14646=EDGE_CURVE('',#11434,#11433,#5769,.T.);
#14647=EDGE_CURVE('',#11432,#11434,#834,.T.);
#14648=EDGE_CURVE('',#11435,#11436,#7476,.T.);
#14649=EDGE_CURVE('',#11435,#11431,#835,.T.);
#14650=EDGE_CURVE('',#11436,#11432,#836,.T.);
#14651=EDGE_CURVE('',#11437,#11438,#7477,.T.);
#14652=EDGE_CURVE('',#11437,#11435,#837,.T.);
#14653=EDGE_CURVE('',#11438,#11436,#838,.T.);
#14654=EDGE_CURVE('',#11439,#11440,#7478,.T.);
#14655=EDGE_CURVE('',#11439,#11437,#839,.T.);
#14656=EDGE_CURVE('',#11440,#11438,#840,.T.);
#14657=EDGE_CURVE('',#11441,#11442,#7479,.T.);
#14658=EDGE_CURVE('',#11441,#11439,#841,.T.);
#14659=EDGE_CURVE('',#11442,#11440,#842,.T.);
#14660=EDGE_CURVE('',#11443,#11444,#7480,.T.);
#14661=EDGE_CURVE('',#11443,#11441,#843,.T.);
#14662=EDGE_CURVE('',#11444,#11442,#844,.T.);
#14663=EDGE_CURVE('',#11445,#11446,#7481,.T.);
#14664=EDGE_CURVE('',#11445,#11443,#845,.T.);
#14665=EDGE_CURVE('',#11446,#11444,#846,.T.);
#14666=EDGE_CURVE('',#11447,#11448,#7482,.T.);
#14667=EDGE_CURVE('',#11447,#11445,#847,.T.);
#14668=EDGE_CURVE('',#11448,#11446,#848,.T.);
#14669=EDGE_CURVE('',#11449,#11450,#7483,.T.);
#14670=EDGE_CURVE('',#11449,#11447,#849,.T.);
#14671=EDGE_CURVE('',#11450,#11448,#850,.T.);
#14672=EDGE_CURVE('',#11451,#11452,#7484,.T.);
#14673=EDGE_CURVE('',#11451,#11449,#851,.T.);
#14674=EDGE_CURVE('',#11452,#11450,#852,.T.);
#14675=EDGE_CURVE('',#11453,#11454,#7485,.T.);
#14676=EDGE_CURVE('',#11453,#11451,#853,.T.);
#14677=EDGE_CURVE('',#11454,#11452,#854,.T.);
#14678=EDGE_CURVE('',#11455,#11456,#7486,.T.);
#14679=EDGE_CURVE('',#11455,#11453,#855,.T.);
#14680=EDGE_CURVE('',#11456,#11454,#856,.T.);
#14681=EDGE_CURVE('',#11457,#11458,#7487,.T.);
#14682=EDGE_CURVE('',#11457,#11455,#857,.T.);
#14683=EDGE_CURVE('',#11458,#11456,#858,.T.);
#14684=EDGE_CURVE('',#11459,#11460,#7488,.T.);
#14685=EDGE_CURVE('',#11459,#11457,#859,.T.);
#14686=EDGE_CURVE('',#11460,#11458,#860,.T.);
#14687=EDGE_CURVE('',#11461,#11462,#7489,.T.);
#14688=EDGE_CURVE('',#11461,#11459,#861,.T.);
#14689=EDGE_CURVE('',#11462,#11460,#862,.T.);
#14690=EDGE_CURVE('',#11463,#11464,#7490,.T.);
#14691=EDGE_CURVE('',#11463,#11461,#863,.T.);
#14692=EDGE_CURVE('',#11464,#11462,#864,.T.);
#14693=EDGE_CURVE('',#11465,#11466,#7491,.T.);
#14694=EDGE_CURVE('',#11465,#11463,#865,.T.);
#14695=EDGE_CURVE('',#11466,#11464,#866,.T.);
#14696=EDGE_CURVE('',#11467,#11468,#7492,.T.);
#14697=EDGE_CURVE('',#11467,#11465,#867,.T.);
#14698=EDGE_CURVE('',#11468,#11466,#868,.T.);
#14699=EDGE_CURVE('',#11469,#11470,#7493,.T.);
#14700=EDGE_CURVE('',#11469,#11467,#869,.T.);
#14701=EDGE_CURVE('',#11470,#11468,#870,.T.);
#14702=EDGE_CURVE('',#11433,#11471,#871,.T.);
#14703=EDGE_CURVE('',#11472,#11471,#5770,.T.);
#14704=EDGE_CURVE('',#11473,#11472,#5771,.T.);
#14705=EDGE_CURVE('',#11473,#11434,#872,.T.);
#14706=EDGE_CURVE('',#11430,#11473,#873,.T.);
#14707=EDGE_CURVE('',#11474,#11396,#874,.T.);
#14708=EDGE_CURVE('',#11474,#11470,#875,.T.);
#14709=EDGE_CURVE('',#11393,#11475,#876,.T.);
#14710=EDGE_CURVE('',#11475,#11474,#5772,.T.);
#14711=EDGE_CURVE('',#11475,#11469,#877,.T.);
#14712=EDGE_CURVE('',#11471,#11429,#878,.T.);
#14713=EDGE_CURVE('',#11476,#11477,#5773,.T.);
#14714=EDGE_CURVE('',#11476,#11478,#7494,.T.);
#14715=EDGE_CURVE('',#11478,#11477,#7495,.T.);
#14716=EDGE_CURVE('',#11477,#11479,#7496,.T.);
#14717=EDGE_CURVE('',#11478,#11480,#7497,.T.);
#14718=EDGE_CURVE('',#11479,#11480,#291,.T.);
#14719=EDGE_CURVE('',#11481,#11476,#7498,.T.);
#14720=EDGE_CURVE('',#11480,#11481,#292,.T.);
#14721=EDGE_CURVE('',#11482,#11483,#5774,.T.);
#14722=EDGE_CURVE('',#11482,#11484,#7499,.T.);
#14723=EDGE_CURVE('',#11484,#11483,#7500,.T.);
#14724=EDGE_CURVE('',#11483,#11485,#7501,.T.);
#14725=EDGE_CURVE('',#11484,#11486,#7502,.T.);
#14726=EDGE_CURVE('',#11485,#11486,#293,.T.);
#14727=EDGE_CURVE('',#11487,#11482,#7503,.T.);
#14728=EDGE_CURVE('',#11486,#11487,#294,.T.);
#14729=EDGE_CURVE('',#11488,#11489,#5775,.T.);
#14730=EDGE_CURVE('',#11488,#11490,#7504,.T.);
#14731=EDGE_CURVE('',#11490,#11489,#7505,.T.);
#14732=EDGE_CURVE('',#11489,#11491,#7506,.T.);
#14733=EDGE_CURVE('',#11490,#11492,#7507,.T.);
#14734=EDGE_CURVE('',#11491,#11492,#295,.T.);
#14735=EDGE_CURVE('',#11493,#11488,#7508,.T.);
#14736=EDGE_CURVE('',#11492,#11493,#296,.T.);
#14737=EDGE_CURVE('',#11494,#11495,#5776,.T.);
#14738=EDGE_CURVE('',#11494,#11496,#7509,.T.);
#14739=EDGE_CURVE('',#11496,#11495,#7510,.T.);
#14740=EDGE_CURVE('',#11495,#11497,#7511,.T.);
#14741=EDGE_CURVE('',#11496,#11498,#7512,.T.);
#14742=EDGE_CURVE('',#11497,#11498,#297,.T.);
#14743=EDGE_CURVE('',#11499,#11494,#7513,.T.);
#14744=EDGE_CURVE('',#11498,#11499,#298,.T.);
#14745=EDGE_CURVE('',#11500,#11501,#5777,.T.);
#14746=EDGE_CURVE('',#11500,#11502,#7514,.T.);
#14747=EDGE_CURVE('',#11502,#11501,#7515,.T.);
#14748=EDGE_CURVE('',#11501,#11503,#7516,.T.);
#14749=EDGE_CURVE('',#11502,#11504,#7517,.T.);
#14750=EDGE_CURVE('',#11503,#11504,#299,.T.);
#14751=EDGE_CURVE('',#11505,#11500,#7518,.T.);
#14752=EDGE_CURVE('',#11504,#11505,#300,.T.);
#14753=EDGE_CURVE('',#11506,#11507,#5778,.T.);
#14754=EDGE_CURVE('',#11506,#11508,#7519,.T.);
#14755=EDGE_CURVE('',#11508,#11507,#7520,.T.);
#14756=EDGE_CURVE('',#11507,#11509,#7521,.T.);
#14757=EDGE_CURVE('',#11508,#11510,#7522,.T.);
#14758=EDGE_CURVE('',#11509,#11510,#301,.T.);
#14759=EDGE_CURVE('',#11511,#11506,#7523,.T.);
#14760=EDGE_CURVE('',#11510,#11511,#302,.T.);
#14761=EDGE_CURVE('',#11512,#11513,#5779,.T.);
#14762=EDGE_CURVE('',#11512,#11514,#7524,.T.);
#14763=EDGE_CURVE('',#11514,#11513,#7525,.T.);
#14764=EDGE_CURVE('',#11513,#11515,#7526,.T.);
#14765=EDGE_CURVE('',#11514,#11516,#7527,.T.);
#14766=EDGE_CURVE('',#11515,#11516,#303,.T.);
#14767=EDGE_CURVE('',#11517,#11512,#7528,.T.);
#14768=EDGE_CURVE('',#11516,#11517,#304,.T.);
#14769=EDGE_CURVE('',#11518,#11519,#5780,.T.);
#14770=EDGE_CURVE('',#11518,#11520,#7529,.T.);
#14771=EDGE_CURVE('',#11520,#11519,#7530,.T.);
#14772=EDGE_CURVE('',#11519,#11521,#7531,.T.);
#14773=EDGE_CURVE('',#11520,#11522,#7532,.T.);
#14774=EDGE_CURVE('',#11521,#11522,#305,.T.);
#14775=EDGE_CURVE('',#11523,#11518,#7533,.T.);
#14776=EDGE_CURVE('',#11522,#11523,#306,.T.);
#14777=EDGE_CURVE('',#11524,#11525,#5781,.T.);
#14778=EDGE_CURVE('',#11524,#11526,#7534,.T.);
#14779=EDGE_CURVE('',#11526,#11525,#7535,.T.);
#14780=EDGE_CURVE('',#11525,#11527,#7536,.T.);
#14781=EDGE_CURVE('',#11526,#11528,#7537,.T.);
#14782=EDGE_CURVE('',#11527,#11528,#307,.T.);
#14783=EDGE_CURVE('',#11529,#11524,#7538,.T.);
#14784=EDGE_CURVE('',#11528,#11529,#308,.T.);
#14785=EDGE_CURVE('',#11530,#11531,#5782,.T.);
#14786=EDGE_CURVE('',#11530,#11532,#7539,.T.);
#14787=EDGE_CURVE('',#11532,#11531,#7540,.T.);
#14788=EDGE_CURVE('',#11531,#11533,#7541,.T.);
#14789=EDGE_CURVE('',#11532,#11534,#7542,.T.);
#14790=EDGE_CURVE('',#11533,#11534,#309,.T.);
#14791=EDGE_CURVE('',#11535,#11530,#7543,.T.);
#14792=EDGE_CURVE('',#11534,#11535,#310,.T.);
#14793=EDGE_CURVE('',#11536,#11537,#5783,.T.);
#14794=EDGE_CURVE('',#11536,#11538,#7544,.T.);
#14795=EDGE_CURVE('',#11538,#11537,#7545,.T.);
#14796=EDGE_CURVE('',#11537,#11539,#7546,.T.);
#14797=EDGE_CURVE('',#11538,#11540,#7547,.T.);
#14798=EDGE_CURVE('',#11539,#11540,#311,.T.);
#14799=EDGE_CURVE('',#11541,#11536,#7548,.T.);
#14800=EDGE_CURVE('',#11540,#11541,#312,.T.);
#14801=EDGE_CURVE('',#11542,#11543,#5784,.T.);
#14802=EDGE_CURVE('',#11542,#11544,#7549,.T.);
#14803=EDGE_CURVE('',#11544,#11543,#7550,.T.);
#14804=EDGE_CURVE('',#11543,#11545,#7551,.T.);
#14805=EDGE_CURVE('',#11544,#11546,#7552,.T.);
#14806=EDGE_CURVE('',#11545,#11546,#313,.T.);
#14807=EDGE_CURVE('',#11547,#11542,#7553,.T.);
#14808=EDGE_CURVE('',#11546,#11547,#314,.T.);
#14809=EDGE_CURVE('',#11548,#11549,#5785,.T.);
#14810=EDGE_CURVE('',#11548,#11550,#7554,.T.);
#14811=EDGE_CURVE('',#11550,#11549,#7555,.T.);
#14812=EDGE_CURVE('',#11549,#11551,#7556,.T.);
#14813=EDGE_CURVE('',#11550,#11552,#7557,.T.);
#14814=EDGE_CURVE('',#11551,#11552,#315,.T.);
#14815=EDGE_CURVE('',#11553,#11548,#7558,.T.);
#14816=EDGE_CURVE('',#11552,#11553,#316,.T.);
#14817=EDGE_CURVE('',#11554,#11555,#5786,.T.);
#14818=EDGE_CURVE('',#11554,#11556,#7559,.T.);
#14819=EDGE_CURVE('',#11556,#11555,#7560,.T.);
#14820=EDGE_CURVE('',#11555,#11557,#7561,.T.);
#14821=EDGE_CURVE('',#11556,#11558,#7562,.T.);
#14822=EDGE_CURVE('',#11557,#11558,#317,.T.);
#14823=EDGE_CURVE('',#11559,#11554,#7563,.T.);
#14824=EDGE_CURVE('',#11558,#11559,#318,.T.);
#14825=EDGE_CURVE('',#11560,#11561,#5787,.T.);
#14826=EDGE_CURVE('',#11560,#11562,#7564,.T.);
#14827=EDGE_CURVE('',#11562,#11561,#7565,.T.);
#14828=EDGE_CURVE('',#11561,#11563,#7566,.T.);
#14829=EDGE_CURVE('',#11562,#11564,#7567,.T.);
#14830=EDGE_CURVE('',#11563,#11564,#319,.T.);
#14831=EDGE_CURVE('',#11565,#11560,#7568,.T.);
#14832=EDGE_CURVE('',#11564,#11565,#320,.T.);
#14833=EDGE_CURVE('',#11566,#11567,#5788,.T.);
#14834=EDGE_CURVE('',#11566,#11568,#7569,.T.);
#14835=EDGE_CURVE('',#11568,#11567,#7570,.T.);
#14836=EDGE_CURVE('',#11567,#11569,#7571,.T.);
#14837=EDGE_CURVE('',#11568,#11570,#7572,.T.);
#14838=EDGE_CURVE('',#11569,#11570,#321,.T.);
#14839=EDGE_CURVE('',#11571,#11566,#7573,.T.);
#14840=EDGE_CURVE('',#11570,#11571,#322,.T.);
#14841=EDGE_CURVE('',#11572,#11573,#5789,.T.);
#14842=EDGE_CURVE('',#11572,#11574,#7574,.T.);
#14843=EDGE_CURVE('',#11574,#11573,#7575,.T.);
#14844=EDGE_CURVE('',#11573,#11575,#7576,.T.);
#14845=EDGE_CURVE('',#11574,#11576,#7577,.T.);
#14846=EDGE_CURVE('',#11575,#11576,#323,.T.);
#14847=EDGE_CURVE('',#11577,#11572,#7578,.T.);
#14848=EDGE_CURVE('',#11576,#11577,#324,.T.);
#14849=EDGE_CURVE('',#11578,#11579,#5790,.T.);
#14850=EDGE_CURVE('',#11578,#11580,#7579,.T.);
#14851=EDGE_CURVE('',#11580,#11581,#7580,.T.);
#14852=EDGE_CURVE('',#11579,#11581,#5791,.T.);
#14853=EDGE_CURVE('',#11581,#11582,#7581,.T.);
#14854=EDGE_CURVE('',#11580,#11583,#7582,.T.);
#14855=EDGE_CURVE('',#11582,#11583,#325,.T.);
#14856=EDGE_CURVE('',#11584,#11578,#7583,.T.);
#14857=EDGE_CURVE('',#11583,#11584,#326,.T.);
#14858=EDGE_CURVE('',#11585,#11586,#5792,.T.);
#14859=EDGE_CURVE('',#11585,#11587,#7584,.T.);
#14860=EDGE_CURVE('',#11587,#11586,#7585,.T.);
#14861=EDGE_CURVE('',#11586,#11588,#7586,.T.);
#14862=EDGE_CURVE('',#11587,#11589,#7587,.T.);
#14863=EDGE_CURVE('',#11588,#11589,#327,.T.);
#14864=EDGE_CURVE('',#11590,#11585,#7588,.T.);
#14865=EDGE_CURVE('',#11589,#11590,#328,.T.);
#14866=EDGE_CURVE('',#11591,#11592,#5793,.T.);
#14867=EDGE_CURVE('',#11591,#11593,#7589,.T.);
#14868=EDGE_CURVE('',#11593,#11592,#7590,.T.);
#14869=EDGE_CURVE('',#11592,#11594,#7591,.T.);
#14870=EDGE_CURVE('',#11593,#11595,#7592,.T.);
#14871=EDGE_CURVE('',#11594,#11595,#329,.T.);
#14872=EDGE_CURVE('',#11596,#11591,#7593,.T.);
#14873=EDGE_CURVE('',#11595,#11596,#330,.T.);
#14874=EDGE_CURVE('',#11597,#11598,#5794,.T.);
#14875=EDGE_CURVE('',#11597,#11599,#7594,.T.);
#14876=EDGE_CURVE('',#11599,#11598,#7595,.T.);
#14877=EDGE_CURVE('',#11598,#11600,#7596,.T.);
#14878=EDGE_CURVE('',#11599,#11601,#7597,.T.);
#14879=EDGE_CURVE('',#11600,#11601,#331,.T.);
#14880=EDGE_CURVE('',#11602,#11597,#7598,.T.);
#14881=EDGE_CURVE('',#11601,#11602,#332,.T.);
#14882=EDGE_CURVE('',#11603,#11604,#5795,.T.);
#14883=EDGE_CURVE('',#11603,#11605,#7599,.T.);
#14884=EDGE_CURVE('',#11605,#11604,#7600,.T.);
#14885=EDGE_CURVE('',#11604,#11606,#7601,.T.);
#14886=EDGE_CURVE('',#11605,#11607,#7602,.T.);
#14887=EDGE_CURVE('',#11606,#11607,#333,.T.);
#14888=EDGE_CURVE('',#11608,#11603,#7603,.T.);
#14889=EDGE_CURVE('',#11607,#11608,#334,.T.);
#14890=EDGE_CURVE('',#11609,#11610,#5796,.T.);
#14891=EDGE_CURVE('',#11609,#11611,#7604,.T.);
#14892=EDGE_CURVE('',#11611,#11610,#7605,.T.);
#14893=EDGE_CURVE('',#11610,#11612,#7606,.T.);
#14894=EDGE_CURVE('',#11611,#11613,#7607,.T.);
#14895=EDGE_CURVE('',#11612,#11613,#335,.T.);
#14896=EDGE_CURVE('',#11614,#11609,#7608,.T.);
#14897=EDGE_CURVE('',#11613,#11614,#336,.T.);
#14898=EDGE_CURVE('',#11615,#11616,#5797,.T.);
#14899=EDGE_CURVE('',#11615,#11617,#7609,.T.);
#14900=EDGE_CURVE('',#11617,#11616,#7610,.T.);
#14901=EDGE_CURVE('',#11616,#11618,#7611,.T.);
#14902=EDGE_CURVE('',#11617,#11619,#7612,.T.);
#14903=EDGE_CURVE('',#11618,#11619,#337,.T.);
#14904=EDGE_CURVE('',#11620,#11615,#7613,.T.);
#14905=EDGE_CURVE('',#11619,#11620,#338,.T.);
#14906=EDGE_CURVE('',#11621,#11622,#5798,.T.);
#14907=EDGE_CURVE('',#11621,#11623,#7614,.T.);
#14908=EDGE_CURVE('',#11623,#11622,#7615,.T.);
#14909=EDGE_CURVE('',#11622,#11624,#7616,.T.);
#14910=EDGE_CURVE('',#11623,#11625,#7617,.T.);
#14911=EDGE_CURVE('',#11624,#11625,#339,.T.);
#14912=EDGE_CURVE('',#11626,#11621,#7618,.T.);
#14913=EDGE_CURVE('',#11625,#11626,#340,.T.);
#14914=EDGE_CURVE('',#11627,#11628,#5799,.T.);
#14915=EDGE_CURVE('',#11627,#11629,#7619,.T.);
#14916=EDGE_CURVE('',#11629,#11628,#7620,.T.);
#14917=EDGE_CURVE('',#11628,#11630,#7621,.T.);
#14918=EDGE_CURVE('',#11629,#11631,#7622,.T.);
#14919=EDGE_CURVE('',#11630,#11631,#341,.T.);
#14920=EDGE_CURVE('',#11632,#11627,#7623,.T.);
#14921=EDGE_CURVE('',#11631,#11632,#342,.T.);
#14922=EDGE_CURVE('',#11633,#11634,#5800,.T.);
#14923=EDGE_CURVE('',#11633,#11635,#7624,.T.);
#14924=EDGE_CURVE('',#11635,#11634,#7625,.T.);
#14925=EDGE_CURVE('',#11634,#11636,#7626,.T.);
#14926=EDGE_CURVE('',#11635,#11637,#7627,.T.);
#14927=EDGE_CURVE('',#11636,#11637,#343,.T.);
#14928=EDGE_CURVE('',#11638,#11633,#7628,.T.);
#14929=EDGE_CURVE('',#11637,#11638,#344,.T.);
#14930=EDGE_CURVE('',#11639,#11640,#5801,.T.);
#14931=EDGE_CURVE('',#11639,#11641,#7629,.T.);
#14932=EDGE_CURVE('',#11641,#11640,#7630,.T.);
#14933=EDGE_CURVE('',#11640,#11642,#7631,.T.);
#14934=EDGE_CURVE('',#11641,#11643,#7632,.T.);
#14935=EDGE_CURVE('',#11642,#11643,#345,.T.);
#14936=EDGE_CURVE('',#11644,#11639,#7633,.T.);
#14937=EDGE_CURVE('',#11643,#11644,#346,.T.);
#14938=EDGE_CURVE('',#11645,#11646,#5802,.T.);
#14939=EDGE_CURVE('',#11645,#11647,#7634,.T.);
#14940=EDGE_CURVE('',#11647,#11646,#7635,.T.);
#14941=EDGE_CURVE('',#11646,#11648,#7636,.T.);
#14942=EDGE_CURVE('',#11647,#11649,#7637,.T.);
#14943=EDGE_CURVE('',#11648,#11649,#347,.T.);
#14944=EDGE_CURVE('',#11650,#11645,#7638,.T.);
#14945=EDGE_CURVE('',#11649,#11650,#348,.T.);
#14946=EDGE_CURVE('',#11651,#11652,#5803,.T.);
#14947=EDGE_CURVE('',#11651,#11653,#7639,.T.);
#14948=EDGE_CURVE('',#11653,#11652,#7640,.T.);
#14949=EDGE_CURVE('',#11652,#11654,#7641,.T.);
#14950=EDGE_CURVE('',#11653,#11655,#7642,.T.);
#14951=EDGE_CURVE('',#11654,#11655,#349,.T.);
#14952=EDGE_CURVE('',#11656,#11651,#7643,.T.);
#14953=EDGE_CURVE('',#11655,#11656,#350,.T.);
#14954=EDGE_CURVE('',#11657,#11658,#5804,.T.);
#14955=EDGE_CURVE('',#11657,#11659,#7644,.T.);
#14956=EDGE_CURVE('',#11659,#11658,#7645,.T.);
#14957=EDGE_CURVE('',#11658,#11660,#7646,.T.);
#14958=EDGE_CURVE('',#11659,#11661,#7647,.T.);
#14959=EDGE_CURVE('',#11660,#11661,#351,.T.);
#14960=EDGE_CURVE('',#11662,#11657,#7648,.T.);
#14961=EDGE_CURVE('',#11661,#11662,#352,.T.);
#14962=EDGE_CURVE('',#11663,#11664,#5805,.T.);
#14963=EDGE_CURVE('',#11663,#11665,#7649,.T.);
#14964=EDGE_CURVE('',#11665,#11664,#7650,.T.);
#14965=EDGE_CURVE('',#11664,#11666,#7651,.T.);
#14966=EDGE_CURVE('',#11665,#11667,#7652,.T.);
#14967=EDGE_CURVE('',#11666,#11667,#353,.T.);
#14968=EDGE_CURVE('',#11668,#11663,#7653,.T.);
#14969=EDGE_CURVE('',#11667,#11668,#354,.T.);
#14970=EDGE_CURVE('',#11669,#11670,#5806,.T.);
#14971=EDGE_CURVE('',#11669,#11671,#7654,.T.);
#14972=EDGE_CURVE('',#11671,#11670,#7655,.T.);
#14973=EDGE_CURVE('',#11670,#11672,#7656,.T.);
#14974=EDGE_CURVE('',#11671,#11673,#7657,.T.);
#14975=EDGE_CURVE('',#11672,#11673,#355,.T.);
#14976=EDGE_CURVE('',#11674,#11669,#7658,.T.);
#14977=EDGE_CURVE('',#11673,#11674,#356,.T.);
#14978=EDGE_CURVE('',#11675,#11676,#5807,.T.);
#14979=EDGE_CURVE('',#11675,#11677,#7659,.T.);
#14980=EDGE_CURVE('',#11677,#11676,#7660,.T.);
#14981=EDGE_CURVE('',#11676,#11678,#7661,.T.);
#14982=EDGE_CURVE('',#11677,#11679,#7662,.T.);
#14983=EDGE_CURVE('',#11678,#11679,#357,.T.);
#14984=EDGE_CURVE('',#11680,#11675,#7663,.T.);
#14985=EDGE_CURVE('',#11679,#11680,#358,.T.);
#14986=EDGE_CURVE('',#11681,#11682,#5808,.T.);
#14987=EDGE_CURVE('',#11681,#11683,#7664,.T.);
#14988=EDGE_CURVE('',#11683,#11682,#7665,.T.);
#14989=EDGE_CURVE('',#11682,#11684,#7666,.T.);
#14990=EDGE_CURVE('',#11683,#11685,#7667,.T.);
#14991=EDGE_CURVE('',#11684,#11685,#359,.T.);
#14992=EDGE_CURVE('',#11686,#11681,#7668,.T.);
#14993=EDGE_CURVE('',#11685,#11686,#360,.T.);
#14994=EDGE_CURVE('',#11487,#11479,#5809,.T.);
#14995=EDGE_CURVE('',#11493,#11485,#5810,.T.);
#14996=EDGE_CURVE('',#11499,#11491,#5811,.T.);
#14997=EDGE_CURVE('',#11505,#11497,#5812,.T.);
#14998=EDGE_CURVE('',#11511,#11503,#5813,.T.);
#14999=EDGE_CURVE('',#11517,#11509,#5814,.T.);
#15000=EDGE_CURVE('',#11523,#11515,#5815,.T.);
#15001=EDGE_CURVE('',#11529,#11521,#5816,.T.);
#15002=EDGE_CURVE('',#11535,#11527,#5817,.T.);
#15003=EDGE_CURVE('',#11541,#11533,#5818,.T.);
#15004=EDGE_CURVE('',#11547,#11539,#5819,.T.);
#15005=EDGE_CURVE('',#11553,#11545,#5820,.T.);
#15006=EDGE_CURVE('',#11559,#11551,#5821,.T.);
#15007=EDGE_CURVE('',#11565,#11557,#5822,.T.);
#15008=EDGE_CURVE('',#11571,#11563,#5823,.T.);
#15009=EDGE_CURVE('',#11577,#11569,#5824,.T.);
#15010=EDGE_CURVE('',#11584,#11575,#5825,.T.);
#15011=EDGE_CURVE('',#11579,#11687,#7669,.T.);
#15012=EDGE_CURVE('',#11687,#11687,#5826,.T.);
#15013=EDGE_CURVE('',#11590,#11582,#5827,.T.);
#15014=EDGE_CURVE('',#11596,#11588,#5828,.T.);
#15015=EDGE_CURVE('',#11602,#11594,#5829,.T.);
#15016=EDGE_CURVE('',#11608,#11600,#5830,.T.);
#15017=EDGE_CURVE('',#11614,#11606,#5831,.T.);
#15018=EDGE_CURVE('',#11620,#11612,#5832,.T.);
#15019=EDGE_CURVE('',#11626,#11618,#5833,.T.);
#15020=EDGE_CURVE('',#11632,#11624,#5834,.T.);
#15021=EDGE_CURVE('',#11638,#11630,#5835,.T.);
#15022=EDGE_CURVE('',#11644,#11636,#5836,.T.);
#15023=EDGE_CURVE('',#11650,#11642,#5837,.T.);
#15024=EDGE_CURVE('',#11656,#11648,#5838,.T.);
#15025=EDGE_CURVE('',#11662,#11654,#5839,.T.);
#15026=EDGE_CURVE('',#11668,#11660,#5840,.T.);
#15027=EDGE_CURVE('',#11674,#11666,#5841,.T.);
#15028=EDGE_CURVE('',#11680,#11672,#5842,.T.);
#15029=EDGE_CURVE('',#11686,#11678,#5843,.T.);
#15030=EDGE_CURVE('',#11688,#11684,#5844,.T.);
#15031=EDGE_CURVE('',#11688,#11689,#7670,.T.);
#15032=EDGE_CURVE('',#11689,#11690,#5845,.T.);
#15033=EDGE_CURVE('',#11690,#11691,#7671,.T.);
#15034=EDGE_CURVE('',#11481,#11691,#5846,.T.);
#15035=EDGE_CURVE('',#11692,#11690,#7672,.T.);
#15036=EDGE_CURVE('',#11692,#11693,#7673,.T.);
#15037=EDGE_CURVE('',#11691,#11693,#361,.T.);
#15038=EDGE_CURVE('',#11693,#11688,#362,.T.);
#15039=EDGE_CURVE('',#11689,#11692,#7674,.T.);
#15040=EDGE_CURVE('',#11694,#11694,#5847,.T.);
#15041=EDGE_CURVE('',#11694,#11583,#7675,.T.);
#15042=EDGE_CURVE('',#11695,#11696,#7676,.T.);
#15043=EDGE_CURVE('',#11696,#11696,#5848,.T.);
#15044=EDGE_CURVE('',#11697,#11698,#7677,.T.);
#15045=EDGE_CURVE('',#11697,#11699,#7678,.T.);
#15046=EDGE_CURVE('',#11699,#11700,#7679,.T.);
#15047=EDGE_CURVE('',#11698,#11700,#7680,.T.);
#15048=EDGE_CURVE('',#11701,#11697,#7681,.T.);
#15049=EDGE_CURVE('',#11701,#11702,#7682,.T.);
#15050=EDGE_CURVE('',#11702,#11699,#7683,.T.);
#15051=EDGE_CURVE('',#11703,#11701,#7684,.T.);
#15052=EDGE_CURVE('',#11703,#11704,#7685,.T.);
#15053=EDGE_CURVE('',#11704,#11702,#7686,.T.);
#15054=EDGE_CURVE('',#11705,#11703,#7687,.T.);
#15055=EDGE_CURVE('',#11705,#11706,#7688,.T.);
#15056=EDGE_CURVE('',#11706,#11704,#7689,.T.);
#15057=EDGE_CURVE('',#11707,#11705,#7690,.T.);
#15058=EDGE_CURVE('',#11707,#11708,#7691,.T.);
#15059=EDGE_CURVE('',#11708,#11706,#7692,.T.);
#15060=EDGE_CURVE('',#11698,#11707,#7693,.T.);
#15061=EDGE_CURVE('',#11700,#11708,#7694,.T.);
#15062=EDGE_CURVE('',#11709,#11709,#5849,.T.);
#15063=EDGE_CURVE('',#11395,#11709,#7695,.T.);
#15064=EDGE_CURVE('',#11471,#11473,#5850,.T.);
#15065=EDGE_CURVE('',#11710,#11710,#5851,.T.);
#15066=EDGE_CURVE('',#11710,#11472,#7696,.T.);
#15067=ORIENTED_EDGE('',*,*,#11711,.T.);
#15068=ORIENTED_EDGE('',*,*,#11712,.T.);
#15069=ORIENTED_EDGE('',*,*,#11713,.T.);
#15070=ORIENTED_EDGE('',*,*,#11714,.T.);
#15071=ORIENTED_EDGE('',*,*,#11715,.T.);
#15072=ORIENTED_EDGE('',*,*,#11716,.T.);
#15073=ORIENTED_EDGE('',*,*,#11711,.F.);
#15074=ORIENTED_EDGE('',*,*,#11717,.T.);
#15075=ORIENTED_EDGE('',*,*,#11718,.T.);
#15076=ORIENTED_EDGE('',*,*,#11719,.T.);
#15077=ORIENTED_EDGE('',*,*,#11715,.F.);
#15078=ORIENTED_EDGE('',*,*,#11720,.T.);
#15079=ORIENTED_EDGE('',*,*,#11721,.T.);
#15080=ORIENTED_EDGE('',*,*,#11722,.T.);
#15081=ORIENTED_EDGE('',*,*,#11718,.F.);
#15082=ORIENTED_EDGE('',*,*,#11723,.T.);
#15083=ORIENTED_EDGE('',*,*,#11724,.T.);
#15084=ORIENTED_EDGE('',*,*,#11725,.T.);
#15085=ORIENTED_EDGE('',*,*,#11721,.F.);
#15086=ORIENTED_EDGE('',*,*,#11726,.T.);
#15087=ORIENTED_EDGE('',*,*,#11727,.T.);
#15088=ORIENTED_EDGE('',*,*,#11728,.T.);
#15089=ORIENTED_EDGE('',*,*,#11724,.F.);
#15090=ORIENTED_EDGE('',*,*,#11729,.T.);
#15091=ORIENTED_EDGE('',*,*,#11730,.T.);
#15092=ORIENTED_EDGE('',*,*,#11731,.T.);
#15093=ORIENTED_EDGE('',*,*,#11727,.F.);
#15094=ORIENTED_EDGE('',*,*,#11732,.T.);
#15095=ORIENTED_EDGE('',*,*,#11713,.F.);
#15096=ORIENTED_EDGE('',*,*,#11733,.T.);
#15097=ORIENTED_EDGE('',*,*,#11730,.F.);
#15098=ORIENTED_EDGE('',*,*,#11734,.T.);
#15099=ORIENTED_EDGE('',*,*,#11728,.F.);
#15100=ORIENTED_EDGE('',*,*,#11735,.T.);
#15101=ORIENTED_EDGE('',*,*,#11736,.F.);
#15102=ORIENTED_EDGE('',*,*,#11737,.F.);
#15103=ORIENTED_EDGE('',*,*,#11731,.F.);
#15104=ORIENTED_EDGE('',*,*,#11738,.T.);
#15105=ORIENTED_EDGE('',*,*,#11739,.F.);
#15106=ORIENTED_EDGE('',*,*,#11735,.F.);
#15107=ORIENTED_EDGE('',*,*,#11733,.F.);
#15108=ORIENTED_EDGE('',*,*,#11740,.F.);
#15109=ORIENTED_EDGE('',*,*,#11741,.F.);
#15110=ORIENTED_EDGE('',*,*,#11738,.F.);
#15111=ORIENTED_EDGE('',*,*,#11712,.F.);
#15112=ORIENTED_EDGE('',*,*,#11742,.T.);
#15113=ORIENTED_EDGE('',*,*,#11743,.F.);
#15114=ORIENTED_EDGE('',*,*,#11740,.T.);
#15115=ORIENTED_EDGE('',*,*,#11714,.F.);
#15116=ORIENTED_EDGE('',*,*,#11734,.F.);
#15117=ORIENTED_EDGE('',*,*,#11732,.F.);
#15118=ORIENTED_EDGE('',*,*,#11729,.F.);
#15119=ORIENTED_EDGE('',*,*,#11726,.F.);
#15120=ORIENTED_EDGE('',*,*,#11723,.F.);
#15121=ORIENTED_EDGE('',*,*,#11720,.F.);
#15122=ORIENTED_EDGE('',*,*,#11717,.F.);
#15123=ORIENTED_EDGE('',*,*,#11744,.F.);
#15124=ORIENTED_EDGE('',*,*,#11745,.F.);
#15125=ORIENTED_EDGE('',*,*,#11746,.T.);
#15126=ORIENTED_EDGE('',*,*,#11747,.T.);
#15127=ORIENTED_EDGE('',*,*,#11748,.T.);
#15128=ORIENTED_EDGE('',*,*,#11749,.F.);
#15129=ORIENTED_EDGE('',*,*,#11750,.F.);
#15130=ORIENTED_EDGE('',*,*,#11751,.T.);
#15131=ORIENTED_EDGE('',*,*,#11743,.T.);
#15132=ORIENTED_EDGE('',*,*,#11752,.T.);
#15133=ORIENTED_EDGE('',*,*,#11753,.T.);
#15134=ORIENTED_EDGE('',*,*,#11754,.T.);
#15135=ORIENTED_EDGE('',*,*,#11741,.T.);
#15136=ORIENTED_EDGE('',*,*,#11751,.F.);
#15137=ORIENTED_EDGE('',*,*,#11755,.T.);
#15138=ORIENTED_EDGE('',*,*,#11756,.T.);
#15139=ORIENTED_EDGE('',*,*,#11739,.T.);
#15140=ORIENTED_EDGE('',*,*,#11754,.F.);
#15141=ORIENTED_EDGE('',*,*,#11757,.T.);
#15142=ORIENTED_EDGE('',*,*,#11758,.T.);
#15143=ORIENTED_EDGE('',*,*,#11736,.T.);
#15144=ORIENTED_EDGE('',*,*,#11756,.F.);
#15145=ORIENTED_EDGE('',*,*,#11759,.T.);
#15146=ORIENTED_EDGE('',*,*,#11760,.T.);
#15147=ORIENTED_EDGE('',*,*,#11761,.T.);
#15148=ORIENTED_EDGE('',*,*,#11758,.F.);
#15149=ORIENTED_EDGE('',*,*,#11762,.T.);
#15150=ORIENTED_EDGE('',*,*,#11763,.T.);
#15151=ORIENTED_EDGE('',*,*,#11764,.T.);
#15152=ORIENTED_EDGE('',*,*,#11760,.F.);
#15153=ORIENTED_EDGE('',*,*,#11765,.T.);
#15154=ORIENTED_EDGE('',*,*,#11766,.T.);
#15155=ORIENTED_EDGE('',*,*,#11767,.T.);
#15156=ORIENTED_EDGE('',*,*,#11763,.F.);
#15157=ORIENTED_EDGE('',*,*,#11768,.T.);
#15158=ORIENTED_EDGE('',*,*,#11752,.F.);
#15159=ORIENTED_EDGE('',*,*,#11769,.T.);
#15160=ORIENTED_EDGE('',*,*,#11766,.F.);
#15161=ORIENTED_EDGE('',*,*,#11770,.T.);
#15162=ORIENTED_EDGE('',*,*,#11759,.F.);
#15163=ORIENTED_EDGE('',*,*,#11771,.F.);
#15164=ORIENTED_EDGE('',*,*,#11772,.F.);
#15165=ORIENTED_EDGE('',*,*,#11773,.F.);
#15166=ORIENTED_EDGE('',*,*,#11757,.F.);
#15167=ORIENTED_EDGE('',*,*,#11774,.T.);
#15168=ORIENTED_EDGE('',*,*,#11775,.F.);
#15169=ORIENTED_EDGE('',*,*,#11771,.T.);
#15170=ORIENTED_EDGE('',*,*,#11755,.F.);
#15171=ORIENTED_EDGE('',*,*,#11776,.F.);
#15172=ORIENTED_EDGE('',*,*,#11777,.F.);
#15173=ORIENTED_EDGE('',*,*,#11774,.F.);
#15174=ORIENTED_EDGE('',*,*,#11753,.F.);
#15175=ORIENTED_EDGE('',*,*,#11778,.T.);
#15176=ORIENTED_EDGE('',*,*,#11779,.F.);
#15177=ORIENTED_EDGE('',*,*,#11776,.T.);
#15178=ORIENTED_EDGE('',*,*,#11722,.F.);
#15179=ORIENTED_EDGE('',*,*,#11780,.T.);
#15180=ORIENTED_EDGE('',*,*,#11764,.F.);
#15181=ORIENTED_EDGE('',*,*,#11781,.F.);
#15182=ORIENTED_EDGE('',*,*,#11719,.F.);
#15183=ORIENTED_EDGE('',*,*,#11781,.T.);
#15184=ORIENTED_EDGE('',*,*,#11767,.F.);
#15185=ORIENTED_EDGE('',*,*,#11782,.F.);
#15186=ORIENTED_EDGE('',*,*,#11716,.F.);
#15187=ORIENTED_EDGE('',*,*,#11782,.T.);
#15188=ORIENTED_EDGE('',*,*,#11769,.F.);
#15189=ORIENTED_EDGE('',*,*,#11742,.F.);
#15190=ORIENTED_EDGE('',*,*,#11783,.T.);
#15191=ORIENTED_EDGE('',*,*,#11784,.T.);
#15192=ORIENTED_EDGE('',*,*,#11785,.T.);
#15193=ORIENTED_EDGE('',*,*,#11786,.T.);
#15194=ORIENTED_EDGE('',*,*,#11787,.T.);
#15195=ORIENTED_EDGE('',*,*,#11788,.T.);
#15196=ORIENTED_EDGE('',*,*,#11783,.F.);
#15197=ORIENTED_EDGE('',*,*,#11789,.T.);
#15198=ORIENTED_EDGE('',*,*,#11790,.T.);
#15199=ORIENTED_EDGE('',*,*,#11791,.T.);
#15200=ORIENTED_EDGE('',*,*,#11787,.F.);
#15201=ORIENTED_EDGE('',*,*,#11792,.T.);
#15202=ORIENTED_EDGE('',*,*,#11793,.T.);
#15203=ORIENTED_EDGE('',*,*,#11794,.T.);
#15204=ORIENTED_EDGE('',*,*,#11790,.F.);
#15205=ORIENTED_EDGE('',*,*,#11795,.T.);
#15206=ORIENTED_EDGE('',*,*,#11796,.T.);
#15207=ORIENTED_EDGE('',*,*,#11797,.T.);
#15208=ORIENTED_EDGE('',*,*,#11793,.F.);
#15209=ORIENTED_EDGE('',*,*,#11798,.T.);
#15210=ORIENTED_EDGE('',*,*,#11799,.T.);
#15211=ORIENTED_EDGE('',*,*,#11800,.T.);
#15212=ORIENTED_EDGE('',*,*,#11796,.F.);
#15213=ORIENTED_EDGE('',*,*,#11801,.T.);
#15214=ORIENTED_EDGE('',*,*,#11802,.T.);
#15215=ORIENTED_EDGE('',*,*,#11803,.T.);
#15216=ORIENTED_EDGE('',*,*,#11799,.F.);
#15217=ORIENTED_EDGE('',*,*,#11804,.T.);
#15218=ORIENTED_EDGE('',*,*,#11785,.F.);
#15219=ORIENTED_EDGE('',*,*,#11805,.T.);
#15220=ORIENTED_EDGE('',*,*,#11802,.F.);
#15221=ORIENTED_EDGE('',*,*,#11806,.T.);
#15222=ORIENTED_EDGE('',*,*,#11800,.F.);
#15223=ORIENTED_EDGE('',*,*,#11807,.T.);
#15224=ORIENTED_EDGE('',*,*,#11808,.F.);
#15225=ORIENTED_EDGE('',*,*,#11809,.F.);
#15226=ORIENTED_EDGE('',*,*,#11803,.F.);
#15227=ORIENTED_EDGE('',*,*,#11810,.T.);
#15228=ORIENTED_EDGE('',*,*,#11811,.F.);
#15229=ORIENTED_EDGE('',*,*,#11807,.F.);
#15230=ORIENTED_EDGE('',*,*,#11805,.F.);
#15231=ORIENTED_EDGE('',*,*,#11812,.F.);
#15232=ORIENTED_EDGE('',*,*,#11813,.F.);
#15233=ORIENTED_EDGE('',*,*,#11810,.F.);
#15234=ORIENTED_EDGE('',*,*,#11784,.F.);
#15235=ORIENTED_EDGE('',*,*,#11814,.T.);
#15236=ORIENTED_EDGE('',*,*,#11815,.F.);
#15237=ORIENTED_EDGE('',*,*,#11812,.T.);
#15238=ORIENTED_EDGE('',*,*,#11786,.F.);
#15239=ORIENTED_EDGE('',*,*,#11806,.F.);
#15240=ORIENTED_EDGE('',*,*,#11804,.F.);
#15241=ORIENTED_EDGE('',*,*,#11801,.F.);
#15242=ORIENTED_EDGE('',*,*,#11798,.F.);
#15243=ORIENTED_EDGE('',*,*,#11795,.F.);
#15244=ORIENTED_EDGE('',*,*,#11792,.F.);
#15245=ORIENTED_EDGE('',*,*,#11789,.F.);
#15246=ORIENTED_EDGE('',*,*,#11816,.F.);
#15247=ORIENTED_EDGE('',*,*,#11817,.F.);
#15248=ORIENTED_EDGE('',*,*,#11818,.T.);
#15249=ORIENTED_EDGE('',*,*,#11819,.T.);
#15250=ORIENTED_EDGE('',*,*,#11820,.T.);
#15251=ORIENTED_EDGE('',*,*,#11821,.T.);
#15252=ORIENTED_EDGE('',*,*,#11822,.F.);
#15253=ORIENTED_EDGE('',*,*,#11823,.T.);
#15254=ORIENTED_EDGE('',*,*,#11815,.T.);
#15255=ORIENTED_EDGE('',*,*,#11824,.T.);
#15256=ORIENTED_EDGE('',*,*,#11772,.T.);
#15257=ORIENTED_EDGE('',*,*,#11825,.T.);
#15258=ORIENTED_EDGE('',*,*,#11813,.T.);
#15259=ORIENTED_EDGE('',*,*,#11823,.F.);
#15260=ORIENTED_EDGE('',*,*,#11775,.T.);
#15261=ORIENTED_EDGE('',*,*,#11826,.T.);
#15262=ORIENTED_EDGE('',*,*,#11811,.T.);
#15263=ORIENTED_EDGE('',*,*,#11825,.F.);
#15264=ORIENTED_EDGE('',*,*,#11777,.T.);
#15265=ORIENTED_EDGE('',*,*,#11827,.T.);
#15266=ORIENTED_EDGE('',*,*,#11808,.T.);
#15267=ORIENTED_EDGE('',*,*,#11826,.F.);
#15268=ORIENTED_EDGE('',*,*,#11779,.T.);
#15269=ORIENTED_EDGE('',*,*,#11828,.T.);
#15270=ORIENTED_EDGE('',*,*,#11829,.T.);
#15271=ORIENTED_EDGE('',*,*,#11827,.F.);
#15272=ORIENTED_EDGE('',*,*,#11830,.T.);
#15273=ORIENTED_EDGE('',*,*,#11831,.T.);
#15274=ORIENTED_EDGE('',*,*,#11832,.T.);
#15275=ORIENTED_EDGE('',*,*,#11828,.F.);
#15276=ORIENTED_EDGE('',*,*,#11833,.T.);
#15277=ORIENTED_EDGE('',*,*,#11834,.T.);
#15278=ORIENTED_EDGE('',*,*,#11835,.T.);
#15279=ORIENTED_EDGE('',*,*,#11831,.F.);
#15280=ORIENTED_EDGE('',*,*,#11836,.T.);
#15281=ORIENTED_EDGE('',*,*,#11824,.F.);
#15282=ORIENTED_EDGE('',*,*,#11837,.T.);
#15283=ORIENTED_EDGE('',*,*,#11834,.F.);
#15284=ORIENTED_EDGE('',*,*,#11838,.T.);
#15285=ORIENTED_EDGE('',*,*,#11794,.F.);
#15286=ORIENTED_EDGE('',*,*,#11839,.T.);
#15287=ORIENTED_EDGE('',*,*,#11832,.F.);
#15288=ORIENTED_EDGE('',*,*,#11840,.F.);
#15289=ORIENTED_EDGE('',*,*,#11791,.F.);
#15290=ORIENTED_EDGE('',*,*,#11840,.T.);
#15291=ORIENTED_EDGE('',*,*,#11835,.F.);
#15292=ORIENTED_EDGE('',*,*,#11841,.F.);
#15293=ORIENTED_EDGE('',*,*,#11788,.F.);
#15294=ORIENTED_EDGE('',*,*,#11841,.T.);
#15295=ORIENTED_EDGE('',*,*,#11837,.F.);
#15296=ORIENTED_EDGE('',*,*,#11814,.F.);
#15297=ORIENTED_EDGE('',*,*,#11744,.T.);
#15298=ORIENTED_EDGE('',*,*,#11842,.T.);
#15299=ORIENTED_EDGE('',*,*,#11843,.T.);
#15300=ORIENTED_EDGE('',*,*,#11844,.T.);
#15301=ORIENTED_EDGE('',*,*,#11842,.F.);
#15302=ORIENTED_EDGE('',*,*,#11845,.F.);
#15303=ORIENTED_EDGE('',*,*,#11846,.T.);
#15304=ORIENTED_EDGE('',*,*,#11843,.F.);
#15305=ORIENTED_EDGE('',*,*,#11844,.F.);
#15306=ORIENTED_EDGE('',*,*,#11846,.F.);
#15307=ORIENTED_EDGE('',*,*,#11750,.T.);
#15308=ORIENTED_EDGE('',*,*,#11847,.T.);
#15309=ORIENTED_EDGE('',*,*,#11848,.T.);
#15310=ORIENTED_EDGE('',*,*,#11849,.T.);
#15311=ORIENTED_EDGE('',*,*,#11847,.F.);
#15312=ORIENTED_EDGE('',*,*,#11850,.F.);
#15313=ORIENTED_EDGE('',*,*,#11851,.T.);
#15314=ORIENTED_EDGE('',*,*,#11848,.F.);
#15315=ORIENTED_EDGE('',*,*,#11849,.F.);
#15316=ORIENTED_EDGE('',*,*,#11851,.F.);
#15317=ORIENTED_EDGE('',*,*,#11745,.T.);
#15318=ORIENTED_EDGE('',*,*,#11852,.T.);
#15319=ORIENTED_EDGE('',*,*,#11853,.T.);
#15320=ORIENTED_EDGE('',*,*,#11854,.T.);
#15321=ORIENTED_EDGE('',*,*,#11852,.F.);
#15322=ORIENTED_EDGE('',*,*,#11855,.F.);
#15323=ORIENTED_EDGE('',*,*,#11856,.T.);
#15324=ORIENTED_EDGE('',*,*,#11853,.F.);
#15325=ORIENTED_EDGE('',*,*,#11854,.F.);
#15326=ORIENTED_EDGE('',*,*,#11856,.F.);
#15327=ORIENTED_EDGE('',*,*,#11749,.T.);
#15328=ORIENTED_EDGE('',*,*,#11857,.T.);
#15329=ORIENTED_EDGE('',*,*,#11858,.T.);
#15330=ORIENTED_EDGE('',*,*,#11859,.T.);
#15331=ORIENTED_EDGE('',*,*,#11857,.F.);
#15332=ORIENTED_EDGE('',*,*,#11860,.F.);
#15333=ORIENTED_EDGE('',*,*,#11861,.T.);
#15334=ORIENTED_EDGE('',*,*,#11858,.F.);
#15335=ORIENTED_EDGE('',*,*,#11859,.F.);
#15336=ORIENTED_EDGE('',*,*,#11861,.F.);
#15337=ORIENTED_EDGE('',*,*,#11816,.T.);
#15338=ORIENTED_EDGE('',*,*,#11862,.T.);
#15339=ORIENTED_EDGE('',*,*,#11863,.T.);
#15340=ORIENTED_EDGE('',*,*,#11864,.T.);
#15341=ORIENTED_EDGE('',*,*,#11862,.F.);
#15342=ORIENTED_EDGE('',*,*,#11865,.F.);
#15343=ORIENTED_EDGE('',*,*,#11866,.T.);
#15344=ORIENTED_EDGE('',*,*,#11863,.F.);
#15345=ORIENTED_EDGE('',*,*,#11864,.F.);
#15346=ORIENTED_EDGE('',*,*,#11866,.F.);
#15347=ORIENTED_EDGE('',*,*,#11822,.T.);
#15348=ORIENTED_EDGE('',*,*,#11867,.T.);
#15349=ORIENTED_EDGE('',*,*,#11868,.T.);
#15350=ORIENTED_EDGE('',*,*,#11869,.T.);
#15351=ORIENTED_EDGE('',*,*,#11867,.F.);
#15352=ORIENTED_EDGE('',*,*,#11870,.F.);
#15353=ORIENTED_EDGE('',*,*,#11871,.T.);
#15354=ORIENTED_EDGE('',*,*,#11868,.F.);
#15355=ORIENTED_EDGE('',*,*,#11869,.F.);
#15356=ORIENTED_EDGE('',*,*,#11871,.F.);
#15357=ORIENTED_EDGE('',*,*,#11817,.T.);
#15358=ORIENTED_EDGE('',*,*,#11872,.T.);
#15359=ORIENTED_EDGE('',*,*,#11873,.T.);
#15360=ORIENTED_EDGE('',*,*,#11874,.T.);
#15361=ORIENTED_EDGE('',*,*,#11872,.F.);
#15362=ORIENTED_EDGE('',*,*,#11875,.F.);
#15363=ORIENTED_EDGE('',*,*,#11876,.T.);
#15364=ORIENTED_EDGE('',*,*,#11873,.F.);
#15365=ORIENTED_EDGE('',*,*,#11874,.F.);
#15366=ORIENTED_EDGE('',*,*,#11876,.F.);
#15367=ORIENTED_EDGE('',*,*,#11748,.F.);
#15368=ORIENTED_EDGE('',*,*,#11877,.T.);
#15369=ORIENTED_EDGE('',*,*,#11878,.T.);
#15370=ORIENTED_EDGE('',*,*,#11877,.F.);
#15371=ORIENTED_EDGE('',*,*,#11878,.F.);
#15372=ORIENTED_EDGE('',*,*,#11879,.T.);
#15373=ORIENTED_EDGE('',*,*,#11880,.T.);
#15374=ORIENTED_EDGE('',*,*,#11879,.F.);
#15375=ORIENTED_EDGE('',*,*,#11880,.F.);
#15376=ORIENTED_EDGE('',*,*,#11881,.T.);
#15377=ORIENTED_EDGE('',*,*,#11882,.T.);
#15378=ORIENTED_EDGE('',*,*,#11881,.F.);
#15379=ORIENTED_EDGE('',*,*,#11875,.T.);
#15380=ORIENTED_EDGE('',*,*,#11882,.F.);
#15381=ORIENTED_EDGE('',*,*,#11747,.F.);
#15382=ORIENTED_EDGE('',*,*,#11883,.T.);
#15383=ORIENTED_EDGE('',*,*,#11884,.T.);
#15384=ORIENTED_EDGE('',*,*,#11883,.F.);
#15385=ORIENTED_EDGE('',*,*,#11884,.F.);
#15386=ORIENTED_EDGE('',*,*,#11885,.T.);
#15387=ORIENTED_EDGE('',*,*,#11886,.T.);
#15388=ORIENTED_EDGE('',*,*,#11885,.F.);
#15389=ORIENTED_EDGE('',*,*,#11886,.F.);
#15390=ORIENTED_EDGE('',*,*,#11887,.T.);
#15391=ORIENTED_EDGE('',*,*,#11888,.T.);
#15392=ORIENTED_EDGE('',*,*,#11887,.F.);
#15393=ORIENTED_EDGE('',*,*,#11870,.T.);
#15394=ORIENTED_EDGE('',*,*,#11888,.F.);
#15395=ORIENTED_EDGE('',*,*,#11746,.F.);
#15396=ORIENTED_EDGE('',*,*,#11889,.T.);
#15397=ORIENTED_EDGE('',*,*,#11890,.T.);
#15398=ORIENTED_EDGE('',*,*,#11889,.F.);
#15399=ORIENTED_EDGE('',*,*,#11890,.F.);
#15400=ORIENTED_EDGE('',*,*,#11891,.T.);
#15401=ORIENTED_EDGE('',*,*,#11892,.T.);
#15402=ORIENTED_EDGE('',*,*,#11891,.F.);
#15403=ORIENTED_EDGE('',*,*,#11892,.F.);
#15404=ORIENTED_EDGE('',*,*,#11893,.T.);
#15405=ORIENTED_EDGE('',*,*,#11894,.T.);
#15406=ORIENTED_EDGE('',*,*,#11893,.F.);
#15407=ORIENTED_EDGE('',*,*,#11865,.T.);
#15408=ORIENTED_EDGE('',*,*,#11894,.F.);
#15409=ORIENTED_EDGE('',*,*,#11818,.F.);
#15410=ORIENTED_EDGE('',*,*,#11895,.T.);
#15411=ORIENTED_EDGE('',*,*,#11896,.T.);
#15412=ORIENTED_EDGE('',*,*,#11895,.F.);
#15413=ORIENTED_EDGE('',*,*,#11896,.F.);
#15414=ORIENTED_EDGE('',*,*,#11897,.T.);
#15415=ORIENTED_EDGE('',*,*,#11898,.T.);
#15416=ORIENTED_EDGE('',*,*,#11897,.F.);
#15417=ORIENTED_EDGE('',*,*,#11898,.F.);
#15418=ORIENTED_EDGE('',*,*,#11899,.T.);
#15419=ORIENTED_EDGE('',*,*,#11900,.T.);
#15420=ORIENTED_EDGE('',*,*,#11899,.F.);
#15421=ORIENTED_EDGE('',*,*,#11860,.T.);
#15422=ORIENTED_EDGE('',*,*,#11900,.F.);
#15423=ORIENTED_EDGE('',*,*,#11819,.F.);
#15424=ORIENTED_EDGE('',*,*,#11901,.T.);
#15425=ORIENTED_EDGE('',*,*,#11902,.T.);
#15426=ORIENTED_EDGE('',*,*,#11901,.F.);
#15427=ORIENTED_EDGE('',*,*,#11902,.F.);
#15428=ORIENTED_EDGE('',*,*,#11903,.T.);
#15429=ORIENTED_EDGE('',*,*,#11904,.T.);
#15430=ORIENTED_EDGE('',*,*,#11903,.F.);
#15431=ORIENTED_EDGE('',*,*,#11904,.F.);
#15432=ORIENTED_EDGE('',*,*,#11905,.T.);
#15433=ORIENTED_EDGE('',*,*,#11906,.T.);
#15434=ORIENTED_EDGE('',*,*,#11905,.F.);
#15435=ORIENTED_EDGE('',*,*,#11855,.T.);
#15436=ORIENTED_EDGE('',*,*,#11906,.F.);
#15437=ORIENTED_EDGE('',*,*,#11820,.F.);
#15438=ORIENTED_EDGE('',*,*,#11907,.T.);
#15439=ORIENTED_EDGE('',*,*,#11908,.T.);
#15440=ORIENTED_EDGE('',*,*,#11907,.F.);
#15441=ORIENTED_EDGE('',*,*,#11908,.F.);
#15442=ORIENTED_EDGE('',*,*,#11909,.T.);
#15443=ORIENTED_EDGE('',*,*,#11910,.T.);
#15444=ORIENTED_EDGE('',*,*,#11909,.F.);
#15445=ORIENTED_EDGE('',*,*,#11910,.F.);
#15446=ORIENTED_EDGE('',*,*,#11911,.T.);
#15447=ORIENTED_EDGE('',*,*,#11912,.T.);
#15448=ORIENTED_EDGE('',*,*,#11911,.F.);
#15449=ORIENTED_EDGE('',*,*,#11850,.T.);
#15450=ORIENTED_EDGE('',*,*,#11912,.F.);
#15451=ORIENTED_EDGE('',*,*,#11821,.F.);
#15452=ORIENTED_EDGE('',*,*,#11913,.T.);
#15453=ORIENTED_EDGE('',*,*,#11914,.T.);
#15454=ORIENTED_EDGE('',*,*,#11913,.F.);
#15455=ORIENTED_EDGE('',*,*,#11914,.F.);
#15456=ORIENTED_EDGE('',*,*,#11915,.T.);
#15457=ORIENTED_EDGE('',*,*,#11916,.T.);
#15458=ORIENTED_EDGE('',*,*,#11915,.F.);
#15459=ORIENTED_EDGE('',*,*,#11916,.F.);
#15460=ORIENTED_EDGE('',*,*,#11917,.T.);
#15461=ORIENTED_EDGE('',*,*,#11918,.T.);
#15462=ORIENTED_EDGE('',*,*,#11917,.F.);
#15463=ORIENTED_EDGE('',*,*,#11845,.T.);
#15464=ORIENTED_EDGE('',*,*,#11918,.F.);
#15465=ORIENTED_EDGE('',*,*,#11797,.F.);
#15466=ORIENTED_EDGE('',*,*,#11809,.T.);
#15467=ORIENTED_EDGE('',*,*,#11829,.F.);
#15468=ORIENTED_EDGE('',*,*,#11839,.F.);
#15469=ORIENTED_EDGE('',*,*,#11725,.F.);
#15470=ORIENTED_EDGE('',*,*,#11737,.T.);
#15471=ORIENTED_EDGE('',*,*,#11761,.F.);
#15472=ORIENTED_EDGE('',*,*,#11780,.F.);
#15473=ORIENTED_EDGE('',*,*,#11770,.F.);
#15474=ORIENTED_EDGE('',*,*,#11919,.F.);
#15475=ORIENTED_EDGE('',*,*,#11830,.F.);
#15476=ORIENTED_EDGE('',*,*,#11778,.F.);
#15477=ORIENTED_EDGE('',*,*,#11762,.F.);
#15478=ORIENTED_EDGE('',*,*,#11773,.T.);
#15479=ORIENTED_EDGE('',*,*,#11838,.F.);
#15480=ORIENTED_EDGE('',*,*,#11920,.T.);
#15481=ORIENTED_EDGE('',*,*,#11768,.F.);
#15482=ORIENTED_EDGE('',*,*,#11921,.T.);
#15483=ORIENTED_EDGE('',*,*,#11833,.F.);
#15484=ORIENTED_EDGE('',*,*,#11919,.T.);
#15485=ORIENTED_EDGE('',*,*,#11765,.F.);
#15486=ORIENTED_EDGE('',*,*,#11920,.F.);
#15487=ORIENTED_EDGE('',*,*,#11836,.F.);
#15488=ORIENTED_EDGE('',*,*,#11921,.F.);
#15489=ORIENTED_EDGE('',*,*,#11922,.T.);
#15490=ORIENTED_EDGE('',*,*,#11923,.T.);
#15491=ORIENTED_EDGE('',*,*,#11924,.T.);
#15492=ORIENTED_EDGE('',*,*,#11925,.T.);
#15493=ORIENTED_EDGE('',*,*,#11926,.T.);
#15494=ORIENTED_EDGE('',*,*,#11927,.T.);
#15495=ORIENTED_EDGE('',*,*,#11928,.T.);
#15496=ORIENTED_EDGE('',*,*,#11923,.F.);
#15497=ORIENTED_EDGE('',*,*,#11929,.T.);
#15498=ORIENTED_EDGE('',*,*,#11930,.T.);
#15499=ORIENTED_EDGE('',*,*,#11927,.F.);
#15500=ORIENTED_EDGE('',*,*,#11931,.T.);
#15501=ORIENTED_EDGE('',*,*,#11932,.T.);
#15502=ORIENTED_EDGE('',*,*,#11933,.T.);
#15503=ORIENTED_EDGE('',*,*,#11929,.F.);
#15504=ORIENTED_EDGE('',*,*,#11934,.T.);
#15505=ORIENTED_EDGE('',*,*,#11935,.T.);
#15506=ORIENTED_EDGE('',*,*,#11936,.T.);
#15507=ORIENTED_EDGE('',*,*,#11932,.F.);
#15508=ORIENTED_EDGE('',*,*,#11937,.T.);
#15509=ORIENTED_EDGE('',*,*,#11938,.T.);
#15510=ORIENTED_EDGE('',*,*,#11935,.F.);
#15511=ORIENTED_EDGE('',*,*,#11939,.T.);
#15512=ORIENTED_EDGE('',*,*,#11925,.F.);
#15513=ORIENTED_EDGE('',*,*,#11936,.F.);
#15514=ORIENTED_EDGE('',*,*,#11940,.F.);
#15515=ORIENTED_EDGE('',*,*,#11941,.F.);
#15516=ORIENTED_EDGE('',*,*,#11942,.T.);
#15517=ORIENTED_EDGE('',*,*,#11938,.F.);
#15518=ORIENTED_EDGE('',*,*,#11943,.T.);
#15519=ORIENTED_EDGE('',*,*,#11944,.F.);
#15520=ORIENTED_EDGE('',*,*,#11940,.T.);
#15521=ORIENTED_EDGE('',*,*,#11924,.F.);
#15522=ORIENTED_EDGE('',*,*,#11945,.T.);
#15523=ORIENTED_EDGE('',*,*,#11946,.F.);
#15524=ORIENTED_EDGE('',*,*,#11943,.F.);
#15525=ORIENTED_EDGE('',*,*,#11922,.F.);
#15526=ORIENTED_EDGE('',*,*,#11939,.F.);
#15527=ORIENTED_EDGE('',*,*,#11937,.F.);
#15528=ORIENTED_EDGE('',*,*,#11934,.F.);
#15529=ORIENTED_EDGE('',*,*,#11931,.F.);
#15530=ORIENTED_EDGE('',*,*,#11926,.F.);
#15531=ORIENTED_EDGE('',*,*,#11947,.F.);
#15532=ORIENTED_EDGE('',*,*,#11948,.F.);
#15533=ORIENTED_EDGE('',*,*,#11949,.F.);
#15534=ORIENTED_EDGE('',*,*,#11950,.F.);
#15535=ORIENTED_EDGE('',*,*,#11951,.F.);
#15536=ORIENTED_EDGE('',*,*,#11952,.F.);
#15537=ORIENTED_EDGE('',*,*,#11953,.F.);
#15538=ORIENTED_EDGE('',*,*,#11954,.T.);
#15539=ORIENTED_EDGE('',*,*,#11946,.T.);
#15540=ORIENTED_EDGE('',*,*,#11955,.T.);
#15541=ORIENTED_EDGE('',*,*,#11956,.T.);
#15542=ORIENTED_EDGE('',*,*,#11957,.T.);
#15543=ORIENTED_EDGE('',*,*,#11958,.T.);
#15544=ORIENTED_EDGE('',*,*,#11957,.F.);
#15545=ORIENTED_EDGE('',*,*,#11959,.F.);
#15546=ORIENTED_EDGE('',*,*,#11960,.F.);
#15547=ORIENTED_EDGE('',*,*,#11961,.F.);
#15548=ORIENTED_EDGE('',*,*,#11962,.T.);
#15549=ORIENTED_EDGE('',*,*,#11963,.T.);
#15550=ORIENTED_EDGE('',*,*,#11964,.T.);
#15551=ORIENTED_EDGE('',*,*,#11956,.F.);
#15552=ORIENTED_EDGE('',*,*,#11965,.F.);
#15553=ORIENTED_EDGE('',*,*,#11966,.T.);
#15554=ORIENTED_EDGE('',*,*,#11967,.T.);
#15555=ORIENTED_EDGE('',*,*,#11968,.T.);
#15556=ORIENTED_EDGE('',*,*,#11959,.T.);
#15557=ORIENTED_EDGE('',*,*,#11955,.F.);
#15558=ORIENTED_EDGE('',*,*,#11969,.T.);
#15559=ORIENTED_EDGE('',*,*,#11970,.F.);
#15560=ORIENTED_EDGE('',*,*,#11971,.T.);
#15561=ORIENTED_EDGE('',*,*,#11965,.T.);
#15562=ORIENTED_EDGE('',*,*,#11954,.F.);
#15563=ORIENTED_EDGE('',*,*,#11972,.T.);
#15564=ORIENTED_EDGE('',*,*,#11973,.T.);
#15565=ORIENTED_EDGE('',*,*,#11974,.T.);
#15566=ORIENTED_EDGE('',*,*,#11944,.T.);
#15567=ORIENTED_EDGE('',*,*,#11975,.T.);
#15568=ORIENTED_EDGE('',*,*,#11941,.T.);
#15569=ORIENTED_EDGE('',*,*,#11974,.F.);
#15570=ORIENTED_EDGE('',*,*,#11976,.T.);
#15571=ORIENTED_EDGE('',*,*,#11977,.T.);
#15572=ORIENTED_EDGE('',*,*,#11978,.T.);
#15573=ORIENTED_EDGE('',*,*,#11975,.F.);
#15574=ORIENTED_EDGE('',*,*,#11979,.T.);
#15575=ORIENTED_EDGE('',*,*,#11970,.T.);
#15576=ORIENTED_EDGE('',*,*,#11980,.T.);
#15577=ORIENTED_EDGE('',*,*,#11977,.F.);
#15578=ORIENTED_EDGE('',*,*,#11981,.T.);
#15579=ORIENTED_EDGE('',*,*,#11933,.F.);
#15580=ORIENTED_EDGE('',*,*,#11942,.F.);
#15581=ORIENTED_EDGE('',*,*,#11978,.F.);
#15582=ORIENTED_EDGE('',*,*,#11982,.T.);
#15583=ORIENTED_EDGE('',*,*,#11930,.F.);
#15584=ORIENTED_EDGE('',*,*,#11982,.F.);
#15585=ORIENTED_EDGE('',*,*,#11980,.F.);
#15586=ORIENTED_EDGE('',*,*,#11983,.T.);
#15587=ORIENTED_EDGE('',*,*,#11928,.F.);
#15588=ORIENTED_EDGE('',*,*,#11983,.F.);
#15589=ORIENTED_EDGE('',*,*,#11969,.F.);
#15590=ORIENTED_EDGE('',*,*,#11945,.F.);
#15591=ORIENTED_EDGE('',*,*,#11968,.F.);
#15592=ORIENTED_EDGE('',*,*,#11984,.T.);
#15593=ORIENTED_EDGE('',*,*,#11985,.T.);
#15594=ORIENTED_EDGE('',*,*,#11986,.T.);
#15595=ORIENTED_EDGE('',*,*,#11987,.F.);
#15596=ORIENTED_EDGE('',*,*,#11960,.T.);
#15597=ORIENTED_EDGE('',*,*,#11958,.F.);
#15598=ORIENTED_EDGE('',*,*,#11961,.T.);
#15599=ORIENTED_EDGE('',*,*,#11987,.T.);
#15600=ORIENTED_EDGE('',*,*,#11988,.T.);
#15601=ORIENTED_EDGE('',*,*,#11989,.T.);
#15602=ORIENTED_EDGE('',*,*,#11972,.F.);
#15603=ORIENTED_EDGE('',*,*,#11973,.F.);
#15604=ORIENTED_EDGE('',*,*,#11989,.F.);
#15605=ORIENTED_EDGE('',*,*,#11990,.F.);
#15606=ORIENTED_EDGE('',*,*,#11991,.F.);
#15607=ORIENTED_EDGE('',*,*,#11988,.F.);
#15608=ORIENTED_EDGE('',*,*,#11986,.F.);
#15609=ORIENTED_EDGE('',*,*,#11992,.T.);
#15610=ORIENTED_EDGE('',*,*,#11993,.F.);
#15611=ORIENTED_EDGE('',*,*,#11990,.T.);
#15612=ORIENTED_EDGE('',*,*,#11967,.F.);
#15613=ORIENTED_EDGE('',*,*,#11994,.T.);
#15614=ORIENTED_EDGE('',*,*,#11995,.T.);
#15615=ORIENTED_EDGE('',*,*,#11996,.T.);
#15616=ORIENTED_EDGE('',*,*,#11984,.F.);
#15617=ORIENTED_EDGE('',*,*,#11997,.T.);
#15618=ORIENTED_EDGE('',*,*,#11998,.T.);
#15619=ORIENTED_EDGE('',*,*,#11995,.F.);
#15620=ORIENTED_EDGE('',*,*,#11999,.T.);
#15621=ORIENTED_EDGE('',*,*,#12000,.T.);
#15622=ORIENTED_EDGE('',*,*,#12001,.T.);
#15623=ORIENTED_EDGE('',*,*,#11997,.F.);
#15624=ORIENTED_EDGE('',*,*,#12002,.T.);
#15625=ORIENTED_EDGE('',*,*,#11993,.T.);
#15626=ORIENTED_EDGE('',*,*,#12003,.T.);
#15627=ORIENTED_EDGE('',*,*,#12000,.F.);
#15628=ORIENTED_EDGE('',*,*,#12004,.T.);
#15629=ORIENTED_EDGE('',*,*,#12003,.F.);
#15630=ORIENTED_EDGE('',*,*,#12005,.T.);
#15631=ORIENTED_EDGE('',*,*,#12006,.F.);
#15632=ORIENTED_EDGE('',*,*,#12007,.F.);
#15633=ORIENTED_EDGE('',*,*,#11992,.F.);
#15634=ORIENTED_EDGE('',*,*,#12008,.F.);
#15635=ORIENTED_EDGE('',*,*,#12009,.F.);
#15636=ORIENTED_EDGE('',*,*,#12005,.F.);
#15637=ORIENTED_EDGE('',*,*,#11985,.F.);
#15638=ORIENTED_EDGE('',*,*,#12010,.F.);
#15639=ORIENTED_EDGE('',*,*,#12011,.F.);
#15640=ORIENTED_EDGE('',*,*,#12008,.T.);
#15641=ORIENTED_EDGE('',*,*,#11981,.F.);
#15642=ORIENTED_EDGE('',*,*,#12012,.T.);
#15643=ORIENTED_EDGE('',*,*,#11999,.F.);
#15644=ORIENTED_EDGE('',*,*,#12013,.T.);
#15645=ORIENTED_EDGE('',*,*,#11971,.F.);
#15646=ORIENTED_EDGE('',*,*,#12013,.F.);
#15647=ORIENTED_EDGE('',*,*,#11994,.F.);
#15648=ORIENTED_EDGE('',*,*,#11966,.F.);
#15649=ORIENTED_EDGE('',*,*,#12014,.T.);
#15650=ORIENTED_EDGE('',*,*,#12015,.T.);
#15651=ORIENTED_EDGE('',*,*,#12011,.T.);
#15652=ORIENTED_EDGE('',*,*,#12016,.T.);
#15653=ORIENTED_EDGE('',*,*,#12017,.T.);
#15654=ORIENTED_EDGE('',*,*,#12018,.T.);
#15655=ORIENTED_EDGE('',*,*,#12009,.T.);
#15656=ORIENTED_EDGE('',*,*,#12015,.F.);
#15657=ORIENTED_EDGE('',*,*,#12019,.T.);
#15658=ORIENTED_EDGE('',*,*,#12006,.T.);
#15659=ORIENTED_EDGE('',*,*,#12018,.F.);
#15660=ORIENTED_EDGE('',*,*,#12020,.T.);
#15661=ORIENTED_EDGE('',*,*,#12021,.T.);
#15662=ORIENTED_EDGE('',*,*,#12022,.T.);
#15663=ORIENTED_EDGE('',*,*,#12019,.F.);
#15664=ORIENTED_EDGE('',*,*,#12023,.T.);
#15665=ORIENTED_EDGE('',*,*,#12024,.T.);
#15666=ORIENTED_EDGE('',*,*,#12025,.T.);
#15667=ORIENTED_EDGE('',*,*,#12021,.F.);
#15668=ORIENTED_EDGE('',*,*,#12026,.T.);
#15669=ORIENTED_EDGE('',*,*,#12027,.T.);
#15670=ORIENTED_EDGE('',*,*,#12024,.F.);
#15671=ORIENTED_EDGE('',*,*,#12028,.T.);
#15672=ORIENTED_EDGE('',*,*,#12016,.F.);
#15673=ORIENTED_EDGE('',*,*,#11998,.F.);
#15674=ORIENTED_EDGE('',*,*,#12029,.T.);
#15675=ORIENTED_EDGE('',*,*,#12025,.F.);
#15676=ORIENTED_EDGE('',*,*,#12030,.F.);
#15677=ORIENTED_EDGE('',*,*,#11996,.F.);
#15678=ORIENTED_EDGE('',*,*,#12030,.T.);
#15679=ORIENTED_EDGE('',*,*,#12027,.F.);
#15680=ORIENTED_EDGE('',*,*,#12010,.T.);
#15681=ORIENTED_EDGE('',*,*,#12014,.F.);
#15682=ORIENTED_EDGE('',*,*,#12028,.F.);
#15683=ORIENTED_EDGE('',*,*,#12026,.F.);
#15684=ORIENTED_EDGE('',*,*,#12023,.F.);
#15685=ORIENTED_EDGE('',*,*,#12020,.F.);
#15686=ORIENTED_EDGE('',*,*,#12017,.F.);
#15687=ORIENTED_EDGE('',*,*,#12031,.F.);
#15688=ORIENTED_EDGE('',*,*,#12032,.F.);
#15689=ORIENTED_EDGE('',*,*,#12033,.T.);
#15690=ORIENTED_EDGE('',*,*,#12034,.T.);
#15691=ORIENTED_EDGE('',*,*,#12035,.T.);
#15692=ORIENTED_EDGE('',*,*,#12036,.T.);
#15693=ORIENTED_EDGE('',*,*,#12037,.T.);
#15694=ORIENTED_EDGE('',*,*,#12038,.T.);
#15695=ORIENTED_EDGE('',*,*,#12039,.F.);
#15696=ORIENTED_EDGE('',*,*,#12040,.F.);
#15697=ORIENTED_EDGE('',*,*,#11947,.T.);
#15698=ORIENTED_EDGE('',*,*,#12041,.T.);
#15699=ORIENTED_EDGE('',*,*,#12042,.T.);
#15700=ORIENTED_EDGE('',*,*,#12041,.F.);
#15701=ORIENTED_EDGE('',*,*,#12042,.F.);
#15702=ORIENTED_EDGE('',*,*,#12043,.T.);
#15703=ORIENTED_EDGE('',*,*,#12044,.F.);
#15704=ORIENTED_EDGE('',*,*,#12043,.F.);
#15705=ORIENTED_EDGE('',*,*,#12031,.T.);
#15706=ORIENTED_EDGE('',*,*,#12045,.T.);
#15707=ORIENTED_EDGE('',*,*,#12046,.T.);
#15708=ORIENTED_EDGE('',*,*,#12047,.T.);
#15709=ORIENTED_EDGE('',*,*,#12045,.F.);
#15710=ORIENTED_EDGE('',*,*,#12048,.F.);
#15711=ORIENTED_EDGE('',*,*,#12049,.T.);
#15712=ORIENTED_EDGE('',*,*,#12046,.F.);
#15713=ORIENTED_EDGE('',*,*,#12047,.F.);
#15714=ORIENTED_EDGE('',*,*,#12049,.F.);
#15715=ORIENTED_EDGE('',*,*,#12044,.T.);
#15716=ORIENTED_EDGE('',*,*,#12050,.T.);
#15717=ORIENTED_EDGE('',*,*,#12051,.T.);
#15718=ORIENTED_EDGE('',*,*,#12050,.F.);
#15719=ORIENTED_EDGE('',*,*,#12048,.T.);
#15720=ORIENTED_EDGE('',*,*,#12051,.F.);
#15721=ORIENTED_EDGE('',*,*,#12040,.T.);
#15722=ORIENTED_EDGE('',*,*,#12052,.T.);
#15723=ORIENTED_EDGE('',*,*,#12053,.T.);
#15724=ORIENTED_EDGE('',*,*,#12054,.T.);
#15725=ORIENTED_EDGE('',*,*,#12052,.F.);
#15726=ORIENTED_EDGE('',*,*,#12055,.F.);
#15727=ORIENTED_EDGE('',*,*,#12056,.T.);
#15728=ORIENTED_EDGE('',*,*,#12053,.F.);
#15729=ORIENTED_EDGE('',*,*,#12054,.F.);
#15730=ORIENTED_EDGE('',*,*,#12056,.F.);
#15731=ORIENTED_EDGE('',*,*,#11953,.T.);
#15732=ORIENTED_EDGE('',*,*,#12057,.T.);
#15733=ORIENTED_EDGE('',*,*,#12055,.T.);
#15734=ORIENTED_EDGE('',*,*,#12057,.F.);
#15735=ORIENTED_EDGE('',*,*,#12032,.T.);
#15736=ORIENTED_EDGE('',*,*,#12058,.T.);
#15737=ORIENTED_EDGE('',*,*,#12059,.T.);
#15738=ORIENTED_EDGE('',*,*,#12060,.T.);
#15739=ORIENTED_EDGE('',*,*,#12058,.F.);
#15740=ORIENTED_EDGE('',*,*,#12061,.F.);
#15741=ORIENTED_EDGE('',*,*,#12062,.T.);
#15742=ORIENTED_EDGE('',*,*,#12059,.F.);
#15743=ORIENTED_EDGE('',*,*,#12060,.F.);
#15744=ORIENTED_EDGE('',*,*,#12062,.F.);
#15745=ORIENTED_EDGE('',*,*,#11948,.T.);
#15746=ORIENTED_EDGE('',*,*,#12063,.T.);
#15747=ORIENTED_EDGE('',*,*,#12061,.T.);
#15748=ORIENTED_EDGE('',*,*,#12063,.F.);
#15749=ORIENTED_EDGE('',*,*,#12039,.T.);
#15750=ORIENTED_EDGE('',*,*,#12064,.T.);
#15751=ORIENTED_EDGE('',*,*,#12065,.T.);
#15752=ORIENTED_EDGE('',*,*,#12066,.T.);
#15753=ORIENTED_EDGE('',*,*,#12064,.F.);
#15754=ORIENTED_EDGE('',*,*,#12067,.F.);
#15755=ORIENTED_EDGE('',*,*,#12068,.T.);
#15756=ORIENTED_EDGE('',*,*,#12065,.F.);
#15757=ORIENTED_EDGE('',*,*,#12066,.F.);
#15758=ORIENTED_EDGE('',*,*,#12068,.F.);
#15759=ORIENTED_EDGE('',*,*,#11952,.T.);
#15760=ORIENTED_EDGE('',*,*,#12069,.T.);
#15761=ORIENTED_EDGE('',*,*,#12067,.T.);
#15762=ORIENTED_EDGE('',*,*,#12069,.F.);
#15763=ORIENTED_EDGE('',*,*,#11949,.T.);
#15764=ORIENTED_EDGE('',*,*,#12070,.T.);
#15765=ORIENTED_EDGE('',*,*,#12071,.T.);
#15766=ORIENTED_EDGE('',*,*,#12070,.F.);
#15767=ORIENTED_EDGE('',*,*,#12071,.F.);
#15768=ORIENTED_EDGE('',*,*,#12072,.T.);
#15769=ORIENTED_EDGE('',*,*,#12073,.T.);
#15770=ORIENTED_EDGE('',*,*,#12072,.F.);
#15771=ORIENTED_EDGE('',*,*,#11951,.T.);
#15772=ORIENTED_EDGE('',*,*,#12074,.T.);
#15773=ORIENTED_EDGE('',*,*,#12075,.T.);
#15774=ORIENTED_EDGE('',*,*,#12074,.F.);
#15775=ORIENTED_EDGE('',*,*,#12075,.F.);
#15776=ORIENTED_EDGE('',*,*,#12076,.T.);
#15777=ORIENTED_EDGE('',*,*,#12077,.T.);
#15778=ORIENTED_EDGE('',*,*,#12076,.F.);
#15779=ORIENTED_EDGE('',*,*,#11950,.T.);
#15780=ORIENTED_EDGE('',*,*,#12078,.T.);
#15781=ORIENTED_EDGE('',*,*,#12079,.T.);
#15782=ORIENTED_EDGE('',*,*,#12078,.F.);
#15783=ORIENTED_EDGE('',*,*,#12079,.F.);
#15784=ORIENTED_EDGE('',*,*,#12080,.T.);
#15785=ORIENTED_EDGE('',*,*,#12081,.T.);
#15786=ORIENTED_EDGE('',*,*,#12080,.F.);
#15787=ORIENTED_EDGE('',*,*,#12082,.T.);
#15788=ORIENTED_EDGE('',*,*,#12083,.T.);
#15789=ORIENTED_EDGE('',*,*,#12084,.T.);
#15790=ORIENTED_EDGE('',*,*,#12083,.F.);
#15791=ORIENTED_EDGE('',*,*,#12085,.F.);
#15792=ORIENTED_EDGE('',*,*,#12086,.F.);
#15793=ORIENTED_EDGE('',*,*,#12087,.T.);
#15794=ORIENTED_EDGE('',*,*,#12084,.F.);
#15795=ORIENTED_EDGE('',*,*,#12087,.F.);
#15796=ORIENTED_EDGE('',*,*,#11979,.F.);
#15797=ORIENTED_EDGE('',*,*,#12088,.F.);
#15798=ORIENTED_EDGE('',*,*,#12002,.F.);
#15799=ORIENTED_EDGE('',*,*,#12012,.F.);
#15800=ORIENTED_EDGE('',*,*,#12082,.F.);
#15801=ORIENTED_EDGE('',*,*,#12089,.T.);
#15802=ORIENTED_EDGE('',*,*,#12090,.T.);
#15803=ORIENTED_EDGE('',*,*,#12091,.T.);
#15804=ORIENTED_EDGE('',*,*,#12085,.T.);
#15805=ORIENTED_EDGE('',*,*,#12086,.T.);
#15806=ORIENTED_EDGE('',*,*,#12091,.F.);
#15807=ORIENTED_EDGE('',*,*,#12092,.F.);
#15808=ORIENTED_EDGE('',*,*,#12093,.T.);
#15809=ORIENTED_EDGE('',*,*,#12089,.F.);
#15810=ORIENTED_EDGE('',*,*,#12090,.F.);
#15811=ORIENTED_EDGE('',*,*,#12093,.F.);
#15812=ORIENTED_EDGE('',*,*,#12094,.T.);
#15813=ORIENTED_EDGE('',*,*,#12092,.T.);
#15814=ORIENTED_EDGE('',*,*,#12094,.F.);
#15815=ORIENTED_EDGE('',*,*,#12095,.T.);
#15816=ORIENTED_EDGE('',*,*,#12096,.T.);
#15817=ORIENTED_EDGE('',*,*,#12095,.F.);
#15818=ORIENTED_EDGE('',*,*,#12096,.F.);
#15819=ORIENTED_EDGE('',*,*,#12097,.T.);
#15820=ORIENTED_EDGE('',*,*,#12098,.T.);
#15821=ORIENTED_EDGE('',*,*,#12097,.F.);
#15822=ORIENTED_EDGE('',*,*,#12098,.F.);
#15823=ORIENTED_EDGE('',*,*,#12099,.T.);
#15824=ORIENTED_EDGE('',*,*,#11964,.F.);
#15825=ORIENTED_EDGE('',*,*,#12099,.F.);
#15826=ORIENTED_EDGE('',*,*,#12100,.T.);
#15827=ORIENTED_EDGE('',*,*,#12101,.T.);
#15828=ORIENTED_EDGE('',*,*,#12100,.F.);
#15829=ORIENTED_EDGE('',*,*,#12101,.F.);
#15830=ORIENTED_EDGE('',*,*,#12102,.T.);
#15831=ORIENTED_EDGE('',*,*,#12103,.T.);
#15832=ORIENTED_EDGE('',*,*,#12102,.F.);
#15833=ORIENTED_EDGE('',*,*,#12103,.F.);
#15834=ORIENTED_EDGE('',*,*,#12104,.T.);
#15835=ORIENTED_EDGE('',*,*,#11963,.F.);
#15836=ORIENTED_EDGE('',*,*,#12104,.F.);
#15837=ORIENTED_EDGE('',*,*,#12105,.T.);
#15838=ORIENTED_EDGE('',*,*,#12106,.T.);
#15839=ORIENTED_EDGE('',*,*,#12105,.F.);
#15840=ORIENTED_EDGE('',*,*,#12106,.F.);
#15841=ORIENTED_EDGE('',*,*,#12107,.T.);
#15842=ORIENTED_EDGE('',*,*,#12108,.T.);
#15843=ORIENTED_EDGE('',*,*,#12107,.F.);
#15844=ORIENTED_EDGE('',*,*,#12108,.F.);
#15845=ORIENTED_EDGE('',*,*,#12109,.T.);
#15846=ORIENTED_EDGE('',*,*,#11962,.F.);
#15847=ORIENTED_EDGE('',*,*,#12109,.F.);
#15848=ORIENTED_EDGE('',*,*,#12081,.F.);
#15849=ORIENTED_EDGE('',*,*,#12110,.T.);
#15850=ORIENTED_EDGE('',*,*,#12033,.F.);
#15851=ORIENTED_EDGE('',*,*,#12110,.F.);
#15852=ORIENTED_EDGE('',*,*,#12077,.F.);
#15853=ORIENTED_EDGE('',*,*,#12111,.T.);
#15854=ORIENTED_EDGE('',*,*,#12038,.F.);
#15855=ORIENTED_EDGE('',*,*,#12111,.F.);
#15856=ORIENTED_EDGE('',*,*,#12073,.F.);
#15857=ORIENTED_EDGE('',*,*,#12112,.T.);
#15858=ORIENTED_EDGE('',*,*,#12034,.F.);
#15859=ORIENTED_EDGE('',*,*,#12112,.F.);
#15860=ORIENTED_EDGE('',*,*,#12113,.T.);
#15861=ORIENTED_EDGE('',*,*,#12114,.T.);
#15862=ORIENTED_EDGE('',*,*,#12113,.F.);
#15863=ORIENTED_EDGE('',*,*,#12114,.F.);
#15864=ORIENTED_EDGE('',*,*,#12115,.T.);
#15865=ORIENTED_EDGE('',*,*,#12116,.T.);
#15866=ORIENTED_EDGE('',*,*,#12115,.F.);
#15867=ORIENTED_EDGE('',*,*,#12116,.F.);
#15868=ORIENTED_EDGE('',*,*,#12117,.T.);
#15869=ORIENTED_EDGE('',*,*,#12035,.F.);
#15870=ORIENTED_EDGE('',*,*,#12117,.F.);
#15871=ORIENTED_EDGE('',*,*,#12118,.T.);
#15872=ORIENTED_EDGE('',*,*,#12119,.T.);
#15873=ORIENTED_EDGE('',*,*,#12118,.F.);
#15874=ORIENTED_EDGE('',*,*,#12119,.F.);
#15875=ORIENTED_EDGE('',*,*,#12120,.T.);
#15876=ORIENTED_EDGE('',*,*,#12121,.T.);
#15877=ORIENTED_EDGE('',*,*,#12120,.F.);
#15878=ORIENTED_EDGE('',*,*,#12121,.F.);
#15879=ORIENTED_EDGE('',*,*,#12122,.T.);
#15880=ORIENTED_EDGE('',*,*,#12036,.F.);
#15881=ORIENTED_EDGE('',*,*,#12122,.F.);
#15882=ORIENTED_EDGE('',*,*,#12123,.T.);
#15883=ORIENTED_EDGE('',*,*,#12124,.T.);
#15884=ORIENTED_EDGE('',*,*,#12123,.F.);
#15885=ORIENTED_EDGE('',*,*,#12124,.F.);
#15886=ORIENTED_EDGE('',*,*,#12125,.T.);
#15887=ORIENTED_EDGE('',*,*,#12126,.T.);
#15888=ORIENTED_EDGE('',*,*,#12125,.F.);
#15889=ORIENTED_EDGE('',*,*,#12126,.F.);
#15890=ORIENTED_EDGE('',*,*,#12127,.T.);
#15891=ORIENTED_EDGE('',*,*,#12037,.F.);
#15892=ORIENTED_EDGE('',*,*,#12127,.F.);
#15893=ORIENTED_EDGE('',*,*,#12001,.F.);
#15894=ORIENTED_EDGE('',*,*,#12007,.T.);
#15895=ORIENTED_EDGE('',*,*,#12022,.F.);
#15896=ORIENTED_EDGE('',*,*,#12029,.F.);
#15897=ORIENTED_EDGE('',*,*,#11976,.F.);
#15898=ORIENTED_EDGE('',*,*,#11991,.T.);
#15899=ORIENTED_EDGE('',*,*,#12004,.F.);
#15900=ORIENTED_EDGE('',*,*,#12088,.T.);
#15901=ORIENTED_EDGE('',*,*,#12128,.T.);
#15902=ORIENTED_EDGE('',*,*,#12129,.T.);
#15903=ORIENTED_EDGE('',*,*,#12130,.T.);
#15904=ORIENTED_EDGE('',*,*,#12131,.T.);
#15905=ORIENTED_EDGE('',*,*,#12132,.T.);
#15906=ORIENTED_EDGE('',*,*,#12133,.T.);
#15907=ORIENTED_EDGE('',*,*,#12128,.F.);
#15908=ORIENTED_EDGE('',*,*,#12134,.T.);
#15909=ORIENTED_EDGE('',*,*,#12135,.T.);
#15910=ORIENTED_EDGE('',*,*,#12136,.T.);
#15911=ORIENTED_EDGE('',*,*,#12132,.F.);
#15912=ORIENTED_EDGE('',*,*,#12137,.T.);
#15913=ORIENTED_EDGE('',*,*,#12138,.T.);
#15914=ORIENTED_EDGE('',*,*,#12139,.T.);
#15915=ORIENTED_EDGE('',*,*,#12135,.F.);
#15916=ORIENTED_EDGE('',*,*,#12140,.T.);
#15917=ORIENTED_EDGE('',*,*,#12141,.T.);
#15918=ORIENTED_EDGE('',*,*,#12142,.T.);
#15919=ORIENTED_EDGE('',*,*,#12138,.F.);
#15920=ORIENTED_EDGE('',*,*,#12143,.T.);
#15921=ORIENTED_EDGE('',*,*,#12144,.T.);
#15922=ORIENTED_EDGE('',*,*,#12145,.T.);
#15923=ORIENTED_EDGE('',*,*,#12141,.F.);
#15924=ORIENTED_EDGE('',*,*,#12146,.T.);
#15925=ORIENTED_EDGE('',*,*,#12147,.T.);
#15926=ORIENTED_EDGE('',*,*,#12148,.T.);
#15927=ORIENTED_EDGE('',*,*,#12144,.F.);
#15928=ORIENTED_EDGE('',*,*,#12149,.T.);
#15929=ORIENTED_EDGE('',*,*,#12130,.F.);
#15930=ORIENTED_EDGE('',*,*,#12150,.T.);
#15931=ORIENTED_EDGE('',*,*,#12147,.F.);
#15932=ORIENTED_EDGE('',*,*,#12151,.T.);
#15933=ORIENTED_EDGE('',*,*,#12145,.F.);
#15934=ORIENTED_EDGE('',*,*,#12152,.T.);
#15935=ORIENTED_EDGE('',*,*,#12153,.F.);
#15936=ORIENTED_EDGE('',*,*,#12154,.F.);
#15937=ORIENTED_EDGE('',*,*,#12148,.F.);
#15938=ORIENTED_EDGE('',*,*,#12155,.T.);
#15939=ORIENTED_EDGE('',*,*,#12156,.F.);
#15940=ORIENTED_EDGE('',*,*,#12152,.F.);
#15941=ORIENTED_EDGE('',*,*,#12150,.F.);
#15942=ORIENTED_EDGE('',*,*,#12157,.F.);
#15943=ORIENTED_EDGE('',*,*,#12158,.F.);
#15944=ORIENTED_EDGE('',*,*,#12155,.F.);
#15945=ORIENTED_EDGE('',*,*,#12129,.F.);
#15946=ORIENTED_EDGE('',*,*,#12159,.T.);
#15947=ORIENTED_EDGE('',*,*,#12160,.F.);
#15948=ORIENTED_EDGE('',*,*,#12157,.T.);
#15949=ORIENTED_EDGE('',*,*,#12131,.F.);
#15950=ORIENTED_EDGE('',*,*,#12151,.F.);
#15951=ORIENTED_EDGE('',*,*,#12149,.F.);
#15952=ORIENTED_EDGE('',*,*,#12146,.F.);
#15953=ORIENTED_EDGE('',*,*,#12143,.F.);
#15954=ORIENTED_EDGE('',*,*,#12140,.F.);
#15955=ORIENTED_EDGE('',*,*,#12137,.F.);
#15956=ORIENTED_EDGE('',*,*,#12134,.F.);
#15957=ORIENTED_EDGE('',*,*,#12161,.F.);
#15958=ORIENTED_EDGE('',*,*,#12162,.T.);
#15959=ORIENTED_EDGE('',*,*,#12163,.T.);
#15960=ORIENTED_EDGE('',*,*,#12164,.T.);
#15961=ORIENTED_EDGE('',*,*,#12165,.T.);
#15962=ORIENTED_EDGE('',*,*,#12166,.T.);
#15963=ORIENTED_EDGE('',*,*,#12167,.T.);
#15964=ORIENTED_EDGE('',*,*,#12168,.T.);
#15965=ORIENTED_EDGE('',*,*,#12169,.T.);
#15966=ORIENTED_EDGE('',*,*,#12170,.T.);
#15967=ORIENTED_EDGE('',*,*,#12165,.F.);
#15968=ORIENTED_EDGE('',*,*,#12171,.T.);
#15969=ORIENTED_EDGE('',*,*,#12172,.T.);
#15970=ORIENTED_EDGE('',*,*,#12173,.T.);
#15971=ORIENTED_EDGE('',*,*,#12169,.F.);
#15972=ORIENTED_EDGE('',*,*,#12174,.T.);
#15973=ORIENTED_EDGE('',*,*,#12175,.T.);
#15974=ORIENTED_EDGE('',*,*,#12160,.T.);
#15975=ORIENTED_EDGE('',*,*,#12172,.F.);
#15976=ORIENTED_EDGE('',*,*,#12176,.T.);
#15977=ORIENTED_EDGE('',*,*,#12177,.T.);
#15978=ORIENTED_EDGE('',*,*,#12158,.T.);
#15979=ORIENTED_EDGE('',*,*,#12175,.F.);
#15980=ORIENTED_EDGE('',*,*,#12178,.T.);
#15981=ORIENTED_EDGE('',*,*,#12179,.T.);
#15982=ORIENTED_EDGE('',*,*,#12156,.T.);
#15983=ORIENTED_EDGE('',*,*,#12177,.F.);
#15984=ORIENTED_EDGE('',*,*,#12180,.T.);
#15985=ORIENTED_EDGE('',*,*,#12181,.T.);
#15986=ORIENTED_EDGE('',*,*,#12153,.T.);
#15987=ORIENTED_EDGE('',*,*,#12179,.F.);
#15988=ORIENTED_EDGE('',*,*,#12182,.T.);
#15989=ORIENTED_EDGE('',*,*,#12167,.F.);
#15990=ORIENTED_EDGE('',*,*,#12183,.T.);
#15991=ORIENTED_EDGE('',*,*,#12181,.F.);
#15992=ORIENTED_EDGE('',*,*,#12184,.T.);
#15993=ORIENTED_EDGE('',*,*,#12176,.F.);
#15994=ORIENTED_EDGE('',*,*,#12185,.T.);
#15995=ORIENTED_EDGE('',*,*,#12186,.F.);
#15996=ORIENTED_EDGE('',*,*,#12187,.T.);
#15997=ORIENTED_EDGE('',*,*,#12174,.F.);
#15998=ORIENTED_EDGE('',*,*,#12188,.F.);
#15999=ORIENTED_EDGE('',*,*,#12189,.F.);
#16000=ORIENTED_EDGE('',*,*,#12185,.F.);
#16001=ORIENTED_EDGE('',*,*,#12171,.F.);
#16002=ORIENTED_EDGE('',*,*,#12190,.T.);
#16003=ORIENTED_EDGE('',*,*,#12191,.F.);
#16004=ORIENTED_EDGE('',*,*,#12188,.T.);
#16005=ORIENTED_EDGE('',*,*,#12168,.F.);
#16006=ORIENTED_EDGE('',*,*,#12192,.F.);
#16007=ORIENTED_EDGE('',*,*,#12193,.F.);
#16008=ORIENTED_EDGE('',*,*,#12190,.F.);
#16009=ORIENTED_EDGE('',*,*,#12142,.F.);
#16010=ORIENTED_EDGE('',*,*,#12154,.T.);
#16011=ORIENTED_EDGE('',*,*,#12183,.F.);
#16012=ORIENTED_EDGE('',*,*,#12194,.F.);
#16013=ORIENTED_EDGE('',*,*,#12139,.F.);
#16014=ORIENTED_EDGE('',*,*,#12194,.T.);
#16015=ORIENTED_EDGE('',*,*,#12166,.F.);
#16016=ORIENTED_EDGE('',*,*,#12195,.F.);
#16017=ORIENTED_EDGE('',*,*,#12196,.T.);
#16018=ORIENTED_EDGE('',*,*,#12197,.T.);
#16019=ORIENTED_EDGE('',*,*,#12198,.T.);
#16020=ORIENTED_EDGE('',*,*,#12186,.T.);
#16021=ORIENTED_EDGE('',*,*,#12199,.T.);
#16022=ORIENTED_EDGE('',*,*,#12200,.T.);
#16023=ORIENTED_EDGE('',*,*,#12196,.F.);
#16024=ORIENTED_EDGE('',*,*,#12189,.T.);
#16025=ORIENTED_EDGE('',*,*,#12201,.T.);
#16026=ORIENTED_EDGE('',*,*,#12202,.T.);
#16027=ORIENTED_EDGE('',*,*,#12199,.F.);
#16028=ORIENTED_EDGE('',*,*,#12191,.T.);
#16029=ORIENTED_EDGE('',*,*,#12203,.T.);
#16030=ORIENTED_EDGE('',*,*,#12204,.T.);
#16031=ORIENTED_EDGE('',*,*,#12201,.F.);
#16032=ORIENTED_EDGE('',*,*,#12193,.T.);
#16033=ORIENTED_EDGE('',*,*,#12205,.T.);
#16034=ORIENTED_EDGE('',*,*,#12206,.T.);
#16035=ORIENTED_EDGE('',*,*,#12203,.F.);
#16036=ORIENTED_EDGE('',*,*,#12207,.T.);
#16037=ORIENTED_EDGE('',*,*,#12208,.T.);
#16038=ORIENTED_EDGE('',*,*,#12209,.T.);
#16039=ORIENTED_EDGE('',*,*,#12205,.F.);
#16040=ORIENTED_EDGE('',*,*,#12210,.T.);
#16041=ORIENTED_EDGE('',*,*,#12211,.T.);
#16042=ORIENTED_EDGE('',*,*,#12212,.T.);
#16043=ORIENTED_EDGE('',*,*,#12208,.F.);
#16044=ORIENTED_EDGE('',*,*,#12213,.T.);
#16045=ORIENTED_EDGE('',*,*,#12198,.F.);
#16046=ORIENTED_EDGE('',*,*,#12214,.T.);
#16047=ORIENTED_EDGE('',*,*,#12211,.F.);
#16048=ORIENTED_EDGE('',*,*,#12215,.T.);
#16049=ORIENTED_EDGE('',*,*,#12209,.F.);
#16050=ORIENTED_EDGE('',*,*,#12216,.F.);
#16051=ORIENTED_EDGE('',*,*,#12217,.F.);
#16052=ORIENTED_EDGE('',*,*,#12218,.T.);
#16053=ORIENTED_EDGE('',*,*,#12212,.F.);
#16054=ORIENTED_EDGE('',*,*,#12219,.F.);
#16055=ORIENTED_EDGE('',*,*,#12220,.F.);
#16056=ORIENTED_EDGE('',*,*,#12216,.T.);
#16057=ORIENTED_EDGE('',*,*,#12214,.F.);
#16058=ORIENTED_EDGE('',*,*,#12221,.F.);
#16059=ORIENTED_EDGE('',*,*,#12222,.F.);
#16060=ORIENTED_EDGE('',*,*,#12219,.T.);
#16061=ORIENTED_EDGE('',*,*,#12197,.F.);
#16062=ORIENTED_EDGE('',*,*,#12223,.T.);
#16063=ORIENTED_EDGE('',*,*,#12224,.F.);
#16064=ORIENTED_EDGE('',*,*,#12221,.T.);
#16065=ORIENTED_EDGE('',*,*,#12161,.T.);
#16066=ORIENTED_EDGE('',*,*,#12225,.T.);
#16067=ORIENTED_EDGE('',*,*,#12226,.T.);
#16068=ORIENTED_EDGE('',*,*,#12227,.T.);
#16069=ORIENTED_EDGE('',*,*,#12225,.F.);
#16070=ORIENTED_EDGE('',*,*,#12228,.F.);
#16071=ORIENTED_EDGE('',*,*,#12229,.T.);
#16072=ORIENTED_EDGE('',*,*,#12226,.F.);
#16073=ORIENTED_EDGE('',*,*,#12227,.F.);
#16074=ORIENTED_EDGE('',*,*,#12229,.F.);
#16075=ORIENTED_EDGE('',*,*,#12230,.T.);
#16076=ORIENTED_EDGE('',*,*,#12224,.T.);
#16077=ORIENTED_EDGE('',*,*,#12231,.T.);
#16078=ORIENTED_EDGE('',*,*,#12232,.T.);
#16079=ORIENTED_EDGE('',*,*,#12233,.T.);
#16080=ORIENTED_EDGE('',*,*,#12222,.T.);
#16081=ORIENTED_EDGE('',*,*,#12230,.F.);
#16082=ORIENTED_EDGE('',*,*,#12234,.T.);
#16083=ORIENTED_EDGE('',*,*,#12235,.T.);
#16084=ORIENTED_EDGE('',*,*,#12220,.T.);
#16085=ORIENTED_EDGE('',*,*,#12233,.F.);
#16086=ORIENTED_EDGE('',*,*,#12236,.T.);
#16087=ORIENTED_EDGE('',*,*,#12237,.T.);
#16088=ORIENTED_EDGE('',*,*,#12217,.T.);
#16089=ORIENTED_EDGE('',*,*,#12235,.F.);
#16090=ORIENTED_EDGE('',*,*,#12238,.T.);
#16091=ORIENTED_EDGE('',*,*,#12239,.T.);
#16092=ORIENTED_EDGE('',*,*,#12240,.T.);
#16093=ORIENTED_EDGE('',*,*,#12237,.F.);
#16094=ORIENTED_EDGE('',*,*,#12241,.T.);
#16095=ORIENTED_EDGE('',*,*,#12242,.T.);
#16096=ORIENTED_EDGE('',*,*,#12243,.T.);
#16097=ORIENTED_EDGE('',*,*,#12239,.F.);
#16098=ORIENTED_EDGE('',*,*,#12244,.T.);
#16099=ORIENTED_EDGE('',*,*,#12245,.T.);
#16100=ORIENTED_EDGE('',*,*,#12246,.T.);
#16101=ORIENTED_EDGE('',*,*,#12242,.F.);
#16102=ORIENTED_EDGE('',*,*,#12247,.T.);
#16103=ORIENTED_EDGE('',*,*,#12231,.F.);
#16104=ORIENTED_EDGE('',*,*,#12248,.T.);
#16105=ORIENTED_EDGE('',*,*,#12245,.F.);
#16106=ORIENTED_EDGE('',*,*,#12249,.T.);
#16107=ORIENTED_EDGE('',*,*,#12204,.F.);
#16108=ORIENTED_EDGE('',*,*,#12250,.F.);
#16109=ORIENTED_EDGE('',*,*,#12243,.F.);
#16110=ORIENTED_EDGE('',*,*,#12251,.T.);
#16111=ORIENTED_EDGE('',*,*,#12202,.F.);
#16112=ORIENTED_EDGE('',*,*,#12251,.F.);
#16113=ORIENTED_EDGE('',*,*,#12246,.F.);
#16114=ORIENTED_EDGE('',*,*,#12252,.T.);
#16115=ORIENTED_EDGE('',*,*,#12200,.F.);
#16116=ORIENTED_EDGE('',*,*,#12252,.F.);
#16117=ORIENTED_EDGE('',*,*,#12248,.F.);
#16118=ORIENTED_EDGE('',*,*,#12223,.F.);
#16119=ORIENTED_EDGE('',*,*,#12232,.F.);
#16120=ORIENTED_EDGE('',*,*,#12249,.F.);
#16121=ORIENTED_EDGE('',*,*,#12247,.F.);
#16122=ORIENTED_EDGE('',*,*,#12244,.F.);
#16123=ORIENTED_EDGE('',*,*,#12241,.F.);
#16124=ORIENTED_EDGE('',*,*,#12238,.F.);
#16125=ORIENTED_EDGE('',*,*,#12236,.F.);
#16126=ORIENTED_EDGE('',*,*,#12234,.F.);
#16127=ORIENTED_EDGE('',*,*,#12253,.F.);
#16128=ORIENTED_EDGE('',*,*,#12254,.T.);
#16129=ORIENTED_EDGE('',*,*,#12255,.T.);
#16130=ORIENTED_EDGE('',*,*,#12256,.T.);
#16131=ORIENTED_EDGE('',*,*,#12255,.F.);
#16132=ORIENTED_EDGE('',*,*,#12257,.F.);
#16133=ORIENTED_EDGE('',*,*,#12258,.T.);
#16134=ORIENTED_EDGE('',*,*,#12254,.F.);
#16135=ORIENTED_EDGE('',*,*,#12258,.F.);
#16136=ORIENTED_EDGE('',*,*,#12228,.T.);
#16137=ORIENTED_EDGE('',*,*,#12256,.F.);
#16138=ORIENTED_EDGE('',*,*,#12259,.T.);
#16139=ORIENTED_EDGE('',*,*,#12260,.T.);
#16140=ORIENTED_EDGE('',*,*,#12253,.T.);
#16141=ORIENTED_EDGE('',*,*,#12260,.F.);
#16142=ORIENTED_EDGE('',*,*,#12259,.F.);
#16143=ORIENTED_EDGE('',*,*,#12261,.T.);
#16144=ORIENTED_EDGE('',*,*,#12262,.F.);
#16145=ORIENTED_EDGE('',*,*,#12261,.F.);
#16146=ORIENTED_EDGE('',*,*,#12262,.T.);
#16147=ORIENTED_EDGE('',*,*,#12263,.T.);
#16148=ORIENTED_EDGE('',*,*,#12257,.T.);
#16149=ORIENTED_EDGE('',*,*,#12263,.F.);
#16150=ORIENTED_EDGE('',*,*,#12264,.T.);
#16151=ORIENTED_EDGE('',*,*,#12265,.T.);
#16152=ORIENTED_EDGE('',*,*,#12264,.F.);
#16153=ORIENTED_EDGE('',*,*,#12265,.F.);
#16154=ORIENTED_EDGE('',*,*,#12266,.T.);
#16155=ORIENTED_EDGE('',*,*,#12267,.T.);
#16156=ORIENTED_EDGE('',*,*,#12266,.F.);
#16157=ORIENTED_EDGE('',*,*,#12267,.F.);
#16158=ORIENTED_EDGE('',*,*,#12268,.T.);
#16159=ORIENTED_EDGE('',*,*,#12162,.F.);
#16160=ORIENTED_EDGE('',*,*,#12268,.F.);
#16161=ORIENTED_EDGE('',*,*,#12269,.T.);
#16162=ORIENTED_EDGE('',*,*,#12270,.T.);
#16163=ORIENTED_EDGE('',*,*,#12269,.F.);
#16164=ORIENTED_EDGE('',*,*,#12270,.F.);
#16165=ORIENTED_EDGE('',*,*,#12271,.T.);
#16166=ORIENTED_EDGE('',*,*,#12272,.T.);
#16167=ORIENTED_EDGE('',*,*,#12271,.F.);
#16168=ORIENTED_EDGE('',*,*,#12272,.F.);
#16169=ORIENTED_EDGE('',*,*,#12273,.T.);
#16170=ORIENTED_EDGE('',*,*,#12163,.F.);
#16171=ORIENTED_EDGE('',*,*,#12273,.F.);
#16172=ORIENTED_EDGE('',*,*,#12274,.T.);
#16173=ORIENTED_EDGE('',*,*,#12275,.T.);
#16174=ORIENTED_EDGE('',*,*,#12274,.F.);
#16175=ORIENTED_EDGE('',*,*,#12275,.F.);
#16176=ORIENTED_EDGE('',*,*,#12276,.T.);
#16177=ORIENTED_EDGE('',*,*,#12277,.T.);
#16178=ORIENTED_EDGE('',*,*,#12276,.F.);
#16179=ORIENTED_EDGE('',*,*,#12277,.F.);
#16180=ORIENTED_EDGE('',*,*,#12278,.T.);
#16181=ORIENTED_EDGE('',*,*,#12164,.F.);
#16182=ORIENTED_EDGE('',*,*,#12278,.F.);
#16183=ORIENTED_EDGE('',*,*,#12206,.F.);
#16184=ORIENTED_EDGE('',*,*,#12218,.F.);
#16185=ORIENTED_EDGE('',*,*,#12240,.F.);
#16186=ORIENTED_EDGE('',*,*,#12250,.T.);
#16187=ORIENTED_EDGE('',*,*,#12133,.F.);
#16188=ORIENTED_EDGE('',*,*,#12279,.T.);
#16189=ORIENTED_EDGE('',*,*,#12173,.F.);
#16190=ORIENTED_EDGE('',*,*,#12159,.F.);
#16191=ORIENTED_EDGE('',*,*,#12136,.F.);
#16192=ORIENTED_EDGE('',*,*,#12195,.T.);
#16193=ORIENTED_EDGE('',*,*,#12170,.F.);
#16194=ORIENTED_EDGE('',*,*,#12279,.F.);
#16195=ORIENTED_EDGE('',*,*,#12182,.F.);
#16196=ORIENTED_EDGE('',*,*,#12280,.F.);
#16197=ORIENTED_EDGE('',*,*,#12210,.F.);
#16198=ORIENTED_EDGE('',*,*,#12281,.F.);
#16199=ORIENTED_EDGE('',*,*,#12180,.F.);
#16200=ORIENTED_EDGE('',*,*,#12282,.T.);
#16201=ORIENTED_EDGE('',*,*,#12213,.F.);
#16202=ORIENTED_EDGE('',*,*,#12280,.T.);
#16203=ORIENTED_EDGE('',*,*,#12178,.F.);
#16204=ORIENTED_EDGE('',*,*,#12187,.F.);
#16205=ORIENTED_EDGE('',*,*,#12215,.F.);
#16206=ORIENTED_EDGE('',*,*,#12282,.F.);
#16207=ORIENTED_EDGE('',*,*,#12184,.F.);
#16208=ORIENTED_EDGE('',*,*,#12281,.T.);
#16209=ORIENTED_EDGE('',*,*,#12207,.F.);
#16210=ORIENTED_EDGE('',*,*,#12192,.T.);
#16211=ORIENTED_EDGE('',*,*,#12283,.T.);
#16212=ORIENTED_EDGE('',*,*,#12284,.T.);
#16213=ORIENTED_EDGE('',*,*,#12285,.T.);
#16214=ORIENTED_EDGE('',*,*,#12286,.T.);
#16215=ORIENTED_EDGE('',*,*,#12284,.F.);
#16216=ORIENTED_EDGE('',*,*,#12285,.F.);
#16217=ORIENTED_EDGE('',*,*,#12286,.F.);
#16218=ORIENTED_EDGE('',*,*,#12287,.T.);
#16219=ORIENTED_EDGE('',*,*,#12288,.F.);
#16220=ORIENTED_EDGE('',*,*,#12289,.F.);
#16221=ORIENTED_EDGE('',*,*,#12287,.F.);
#16222=ORIENTED_EDGE('',*,*,#12283,.F.);
#16223=ORIENTED_EDGE('',*,*,#12290,.T.);
#16224=ORIENTED_EDGE('',*,*,#12291,.F.);
#16225=ORIENTED_EDGE('',*,*,#12290,.F.);
#16226=ORIENTED_EDGE('',*,*,#12292,.T.);
#16227=ORIENTED_EDGE('',*,*,#12293,.T.);
#16228=ORIENTED_EDGE('',*,*,#12288,.T.);
#16229=ORIENTED_EDGE('',*,*,#12289,.T.);
#16230=ORIENTED_EDGE('',*,*,#12293,.F.);
#16231=ORIENTED_EDGE('',*,*,#12294,.F.);
#16232=ORIENTED_EDGE('',*,*,#12295,.T.);
#16233=ORIENTED_EDGE('',*,*,#12292,.F.);
#16234=ORIENTED_EDGE('',*,*,#12295,.F.);
#16235=ORIENTED_EDGE('',*,*,#12294,.T.);
#16236=ORIENTED_EDGE('',*,*,#12296,.T.);
#16237=ORIENTED_EDGE('',*,*,#12297,.T.);
#16238=ORIENTED_EDGE('',*,*,#12296,.F.);
#16239=ORIENTED_EDGE('',*,*,#12298,.F.);
#16240=ORIENTED_EDGE('',*,*,#12299,.T.);
#16241=ORIENTED_EDGE('',*,*,#12300,.T.);
#16242=ORIENTED_EDGE('',*,*,#12301,.T.);
#16243=ORIENTED_EDGE('',*,*,#12297,.F.);
#16244=ORIENTED_EDGE('',*,*,#12302,.T.);
#16245=ORIENTED_EDGE('',*,*,#12303,.T.);
#16246=ORIENTED_EDGE('',*,*,#12298,.T.);
#16247=ORIENTED_EDGE('',*,*,#12303,.F.);
#16248=ORIENTED_EDGE('',*,*,#12304,.F.);
#16249=ORIENTED_EDGE('',*,*,#12305,.T.);
#16250=ORIENTED_EDGE('',*,*,#12302,.F.);
#16251=ORIENTED_EDGE('',*,*,#12305,.F.);
#16252=ORIENTED_EDGE('',*,*,#12291,.T.);
#16253=ORIENTED_EDGE('',*,*,#12306,.T.);
#16254=ORIENTED_EDGE('',*,*,#12307,.T.);
#16255=ORIENTED_EDGE('',*,*,#12306,.F.);
#16256=ORIENTED_EDGE('',*,*,#12308,.F.);
#16257=ORIENTED_EDGE('',*,*,#12307,.F.);
#16258=ORIENTED_EDGE('',*,*,#12304,.T.);
#16259=ORIENTED_EDGE('',*,*,#12309,.T.);
#16260=ORIENTED_EDGE('',*,*,#12310,.T.);
#16261=ORIENTED_EDGE('',*,*,#12311,.T.);
#16262=ORIENTED_EDGE('',*,*,#12309,.F.);
#16263=ORIENTED_EDGE('',*,*,#12312,.F.);
#16264=ORIENTED_EDGE('',*,*,#12313,.F.);
#16265=ORIENTED_EDGE('',*,*,#12314,.T.);
#16266=ORIENTED_EDGE('',*,*,#12310,.F.);
#16267=ORIENTED_EDGE('',*,*,#12311,.F.);
#16268=ORIENTED_EDGE('',*,*,#12314,.F.);
#16269=ORIENTED_EDGE('',*,*,#12315,.T.);
#16270=ORIENTED_EDGE('',*,*,#12316,.T.);
#16271=ORIENTED_EDGE('',*,*,#12308,.T.);
#16272=ORIENTED_EDGE('',*,*,#12316,.F.);
#16273=ORIENTED_EDGE('',*,*,#12315,.F.);
#16274=ORIENTED_EDGE('',*,*,#12317,.T.);
#16275=ORIENTED_EDGE('',*,*,#12318,.F.);
#16276=ORIENTED_EDGE('',*,*,#12317,.F.);
#16277=ORIENTED_EDGE('',*,*,#12318,.T.);
#16278=ORIENTED_EDGE('',*,*,#12319,.T.);
#16279=ORIENTED_EDGE('',*,*,#12312,.T.);
#16280=ORIENTED_EDGE('',*,*,#12313,.T.);
#16281=ORIENTED_EDGE('',*,*,#12319,.F.);
#16282=ORIENTED_EDGE('',*,*,#12320,.T.);
#16283=ORIENTED_EDGE('',*,*,#12321,.T.);
#16284=ORIENTED_EDGE('',*,*,#12320,.F.);
#16285=ORIENTED_EDGE('',*,*,#12321,.F.);
#16286=ORIENTED_EDGE('',*,*,#12322,.T.);
#16287=ORIENTED_EDGE('',*,*,#12323,.T.);
#16288=ORIENTED_EDGE('',*,*,#12322,.F.);
#16289=ORIENTED_EDGE('',*,*,#12323,.F.);
#16290=ORIENTED_EDGE('',*,*,#12324,.T.);
#16291=ORIENTED_EDGE('',*,*,#12299,.F.);
#16292=ORIENTED_EDGE('',*,*,#12324,.F.);
#16293=ORIENTED_EDGE('',*,*,#12325,.T.);
#16294=ORIENTED_EDGE('',*,*,#12326,.T.);
#16295=ORIENTED_EDGE('',*,*,#12325,.F.);
#16296=ORIENTED_EDGE('',*,*,#12326,.F.);
#16297=ORIENTED_EDGE('',*,*,#12327,.T.);
#16298=ORIENTED_EDGE('',*,*,#12328,.T.);
#16299=ORIENTED_EDGE('',*,*,#12327,.F.);
#16300=ORIENTED_EDGE('',*,*,#12328,.F.);
#16301=ORIENTED_EDGE('',*,*,#12329,.T.);
#16302=ORIENTED_EDGE('',*,*,#12300,.F.);
#16303=ORIENTED_EDGE('',*,*,#12329,.F.);
#16304=ORIENTED_EDGE('',*,*,#12330,.T.);
#16305=ORIENTED_EDGE('',*,*,#12331,.T.);
#16306=ORIENTED_EDGE('',*,*,#12330,.F.);
#16307=ORIENTED_EDGE('',*,*,#12331,.F.);
#16308=ORIENTED_EDGE('',*,*,#12332,.T.);
#16309=ORIENTED_EDGE('',*,*,#12333,.T.);
#16310=ORIENTED_EDGE('',*,*,#12332,.F.);
#16311=ORIENTED_EDGE('',*,*,#12333,.F.);
#16312=ORIENTED_EDGE('',*,*,#12334,.T.);
#16313=ORIENTED_EDGE('',*,*,#12301,.F.);
#16314=ORIENTED_EDGE('',*,*,#12334,.F.);
#16315=ORIENTED_EDGE('',*,*,#12335,.T.);
#16316=ORIENTED_EDGE('',*,*,#12336,.T.);
#16317=ORIENTED_EDGE('',*,*,#12337,.T.);
#16318=ORIENTED_EDGE('',*,*,#12338,.T.);
#16319=ORIENTED_EDGE('',*,*,#12336,.F.);
#16320=ORIENTED_EDGE('',*,*,#12339,.F.);
#16321=ORIENTED_EDGE('',*,*,#12340,.T.);
#16322=ORIENTED_EDGE('',*,*,#12337,.F.);
#16323=ORIENTED_EDGE('',*,*,#12338,.F.);
#16324=ORIENTED_EDGE('',*,*,#12340,.F.);
#16325=ORIENTED_EDGE('',*,*,#12341,.F.);
#16326=ORIENTED_EDGE('',*,*,#12342,.F.);
#16327=ORIENTED_EDGE('',*,*,#12343,.F.);
#16328=ORIENTED_EDGE('',*,*,#12344,.F.);
#16329=ORIENTED_EDGE('',*,*,#12345,.F.);
#16330=ORIENTED_EDGE('',*,*,#12346,.F.);
#16331=ORIENTED_EDGE('',*,*,#12347,.F.);
#16332=ORIENTED_EDGE('',*,*,#12335,.F.);
#16333=ORIENTED_EDGE('',*,*,#12348,.T.);
#16334=ORIENTED_EDGE('',*,*,#12349,.T.);
#16335=ORIENTED_EDGE('',*,*,#12339,.T.);
#16336=ORIENTED_EDGE('',*,*,#12349,.F.);
#16337=ORIENTED_EDGE('',*,*,#12350,.F.);
#16338=ORIENTED_EDGE('',*,*,#12351,.F.);
#16339=ORIENTED_EDGE('',*,*,#12352,.F.);
#16340=ORIENTED_EDGE('',*,*,#12353,.F.);
#16341=ORIENTED_EDGE('',*,*,#12354,.F.);
#16342=ORIENTED_EDGE('',*,*,#12355,.F.);
#16343=ORIENTED_EDGE('',*,*,#12356,.F.);
#16344=ORIENTED_EDGE('',*,*,#12348,.F.);
#16345=ORIENTED_EDGE('',*,*,#12342,.T.);
#16346=ORIENTED_EDGE('',*,*,#12357,.T.);
#16347=ORIENTED_EDGE('',*,*,#12358,.T.);
#16348=ORIENTED_EDGE('',*,*,#12359,.T.);
#16349=ORIENTED_EDGE('',*,*,#12357,.F.);
#16350=ORIENTED_EDGE('',*,*,#12360,.F.);
#16351=ORIENTED_EDGE('',*,*,#12361,.T.);
#16352=ORIENTED_EDGE('',*,*,#12358,.F.);
#16353=ORIENTED_EDGE('',*,*,#12359,.F.);
#16354=ORIENTED_EDGE('',*,*,#12361,.F.);
#16355=ORIENTED_EDGE('',*,*,#12351,.T.);
#16356=ORIENTED_EDGE('',*,*,#12362,.T.);
#16357=ORIENTED_EDGE('',*,*,#12360,.T.);
#16358=ORIENTED_EDGE('',*,*,#12362,.F.);
#16359=ORIENTED_EDGE('',*,*,#12347,.T.);
#16360=ORIENTED_EDGE('',*,*,#12363,.T.);
#16361=ORIENTED_EDGE('',*,*,#12364,.T.);
#16362=ORIENTED_EDGE('',*,*,#12365,.T.);
#16363=ORIENTED_EDGE('',*,*,#12363,.F.);
#16364=ORIENTED_EDGE('',*,*,#12366,.F.);
#16365=ORIENTED_EDGE('',*,*,#12367,.T.);
#16366=ORIENTED_EDGE('',*,*,#12364,.F.);
#16367=ORIENTED_EDGE('',*,*,#12365,.F.);
#16368=ORIENTED_EDGE('',*,*,#12367,.F.);
#16369=ORIENTED_EDGE('',*,*,#12356,.T.);
#16370=ORIENTED_EDGE('',*,*,#12368,.T.);
#16371=ORIENTED_EDGE('',*,*,#12366,.T.);
#16372=ORIENTED_EDGE('',*,*,#12368,.F.);
#16373=ORIENTED_EDGE('',*,*,#12343,.T.);
#16374=ORIENTED_EDGE('',*,*,#12369,.T.);
#16375=ORIENTED_EDGE('',*,*,#12370,.T.);
#16376=ORIENTED_EDGE('',*,*,#12371,.T.);
#16377=ORIENTED_EDGE('',*,*,#12369,.F.);
#16378=ORIENTED_EDGE('',*,*,#12372,.F.);
#16379=ORIENTED_EDGE('',*,*,#12373,.T.);
#16380=ORIENTED_EDGE('',*,*,#12370,.F.);
#16381=ORIENTED_EDGE('',*,*,#12371,.F.);
#16382=ORIENTED_EDGE('',*,*,#12373,.F.);
#16383=ORIENTED_EDGE('',*,*,#12352,.T.);
#16384=ORIENTED_EDGE('',*,*,#12374,.T.);
#16385=ORIENTED_EDGE('',*,*,#12372,.T.);
#16386=ORIENTED_EDGE('',*,*,#12374,.F.);
#16387=ORIENTED_EDGE('',*,*,#12346,.T.);
#16388=ORIENTED_EDGE('',*,*,#12375,.T.);
#16389=ORIENTED_EDGE('',*,*,#12376,.T.);
#16390=ORIENTED_EDGE('',*,*,#12377,.T.);
#16391=ORIENTED_EDGE('',*,*,#12375,.F.);
#16392=ORIENTED_EDGE('',*,*,#12378,.F.);
#16393=ORIENTED_EDGE('',*,*,#12379,.T.);
#16394=ORIENTED_EDGE('',*,*,#12376,.F.);
#16395=ORIENTED_EDGE('',*,*,#12377,.F.);
#16396=ORIENTED_EDGE('',*,*,#12379,.F.);
#16397=ORIENTED_EDGE('',*,*,#12355,.T.);
#16398=ORIENTED_EDGE('',*,*,#12380,.T.);
#16399=ORIENTED_EDGE('',*,*,#12378,.T.);
#16400=ORIENTED_EDGE('',*,*,#12380,.F.);
#16401=ORIENTED_EDGE('',*,*,#12344,.T.);
#16402=ORIENTED_EDGE('',*,*,#12381,.T.);
#16403=ORIENTED_EDGE('',*,*,#12382,.T.);
#16404=ORIENTED_EDGE('',*,*,#12383,.T.);
#16405=ORIENTED_EDGE('',*,*,#12381,.F.);
#16406=ORIENTED_EDGE('',*,*,#12384,.F.);
#16407=ORIENTED_EDGE('',*,*,#12385,.T.);
#16408=ORIENTED_EDGE('',*,*,#12382,.F.);
#16409=ORIENTED_EDGE('',*,*,#12383,.F.);
#16410=ORIENTED_EDGE('',*,*,#12385,.F.);
#16411=ORIENTED_EDGE('',*,*,#12353,.T.);
#16412=ORIENTED_EDGE('',*,*,#12386,.T.);
#16413=ORIENTED_EDGE('',*,*,#12384,.T.);
#16414=ORIENTED_EDGE('',*,*,#12386,.F.);
#16415=ORIENTED_EDGE('',*,*,#12341,.T.);
#16416=ORIENTED_EDGE('',*,*,#12387,.T.);
#16417=ORIENTED_EDGE('',*,*,#12388,.T.);
#16418=ORIENTED_EDGE('',*,*,#12389,.T.);
#16419=ORIENTED_EDGE('',*,*,#12387,.F.);
#16420=ORIENTED_EDGE('',*,*,#12388,.F.);
#16421=ORIENTED_EDGE('',*,*,#12389,.F.);
#16422=ORIENTED_EDGE('',*,*,#12390,.T.);
#16423=ORIENTED_EDGE('',*,*,#12391,.F.);
#16424=ORIENTED_EDGE('',*,*,#12392,.F.);
#16425=ORIENTED_EDGE('',*,*,#12390,.F.);
#16426=ORIENTED_EDGE('',*,*,#12391,.T.);
#16427=ORIENTED_EDGE('',*,*,#12392,.T.);
#16428=ORIENTED_EDGE('',*,*,#12393,.T.);
#16429=ORIENTED_EDGE('',*,*,#12350,.T.);
#16430=ORIENTED_EDGE('',*,*,#12393,.F.);
#16431=ORIENTED_EDGE('',*,*,#12354,.T.);
#16432=ORIENTED_EDGE('',*,*,#12394,.T.);
#16433=ORIENTED_EDGE('',*,*,#12395,.T.);
#16434=ORIENTED_EDGE('',*,*,#12396,.T.);
#16435=ORIENTED_EDGE('',*,*,#12394,.F.);
#16436=ORIENTED_EDGE('',*,*,#12397,.F.);
#16437=ORIENTED_EDGE('',*,*,#12398,.F.);
#16438=ORIENTED_EDGE('',*,*,#12399,.T.);
#16439=ORIENTED_EDGE('',*,*,#12395,.F.);
#16440=ORIENTED_EDGE('',*,*,#12396,.F.);
#16441=ORIENTED_EDGE('',*,*,#12399,.F.);
#16442=ORIENTED_EDGE('',*,*,#12397,.T.);
#16443=ORIENTED_EDGE('',*,*,#12398,.T.);
#16444=ORIENTED_EDGE('',*,*,#12400,.T.);
#16445=ORIENTED_EDGE('',*,*,#12345,.T.);
#16446=ORIENTED_EDGE('',*,*,#12400,.F.);
#16447=ORIENTED_EDGE('',*,*,#12401,.F.);
#16448=ORIENTED_EDGE('',*,*,#12402,.T.);
#16449=ORIENTED_EDGE('',*,*,#12403,.T.);
#16450=ORIENTED_EDGE('',*,*,#12404,.T.);
#16451=ORIENTED_EDGE('',*,*,#12403,.F.);
#16452=ORIENTED_EDGE('',*,*,#12405,.T.);
#16453=ORIENTED_EDGE('',*,*,#12406,.T.);
#16454=ORIENTED_EDGE('',*,*,#12407,.T.);
#16455=ORIENTED_EDGE('',*,*,#12408,.F.);
#16456=ORIENTED_EDGE('',*,*,#12409,.T.);
#16457=ORIENTED_EDGE('',*,*,#12401,.T.);
#16458=ORIENTED_EDGE('',*,*,#12410,.T.);
#16459=ORIENTED_EDGE('',*,*,#12411,.F.);
#16460=ORIENTED_EDGE('',*,*,#12412,.T.);
#16461=ORIENTED_EDGE('',*,*,#12408,.T.);
#16462=ORIENTED_EDGE('',*,*,#12413,.T.);
#16463=ORIENTED_EDGE('',*,*,#12414,.F.);
#16464=ORIENTED_EDGE('',*,*,#12415,.T.);
#16465=ORIENTED_EDGE('',*,*,#12411,.T.);
#16466=ORIENTED_EDGE('',*,*,#12416,.T.);
#16467=ORIENTED_EDGE('',*,*,#12417,.F.);
#16468=ORIENTED_EDGE('',*,*,#12418,.T.);
#16469=ORIENTED_EDGE('',*,*,#12414,.T.);
#16470=ORIENTED_EDGE('',*,*,#12419,.T.);
#16471=ORIENTED_EDGE('',*,*,#12420,.F.);
#16472=ORIENTED_EDGE('',*,*,#12421,.T.);
#16473=ORIENTED_EDGE('',*,*,#12417,.T.);
#16474=ORIENTED_EDGE('',*,*,#12422,.T.);
#16475=ORIENTED_EDGE('',*,*,#12423,.F.);
#16476=ORIENTED_EDGE('',*,*,#12424,.T.);
#16477=ORIENTED_EDGE('',*,*,#12420,.T.);
#16478=ORIENTED_EDGE('',*,*,#12425,.T.);
#16479=ORIENTED_EDGE('',*,*,#12426,.F.);
#16480=ORIENTED_EDGE('',*,*,#12427,.T.);
#16481=ORIENTED_EDGE('',*,*,#12423,.T.);
#16482=ORIENTED_EDGE('',*,*,#12428,.T.);
#16483=ORIENTED_EDGE('',*,*,#12429,.F.);
#16484=ORIENTED_EDGE('',*,*,#12430,.T.);
#16485=ORIENTED_EDGE('',*,*,#12426,.T.);
#16486=ORIENTED_EDGE('',*,*,#12431,.T.);
#16487=ORIENTED_EDGE('',*,*,#12432,.F.);
#16488=ORIENTED_EDGE('',*,*,#12433,.T.);
#16489=ORIENTED_EDGE('',*,*,#12429,.T.);
#16490=ORIENTED_EDGE('',*,*,#12434,.T.);
#16491=ORIENTED_EDGE('',*,*,#12435,.F.);
#16492=ORIENTED_EDGE('',*,*,#12436,.T.);
#16493=ORIENTED_EDGE('',*,*,#12437,.F.);
#16494=ORIENTED_EDGE('',*,*,#12438,.F.);
#16495=ORIENTED_EDGE('',*,*,#12439,.F.);
#16496=ORIENTED_EDGE('',*,*,#12440,.T.);
#16497=ORIENTED_EDGE('',*,*,#12435,.T.);
#16498=ORIENTED_EDGE('',*,*,#12441,.F.);
#16499=ORIENTED_EDGE('',*,*,#12442,.F.);
#16500=ORIENTED_EDGE('',*,*,#12443,.T.);
#16501=ORIENTED_EDGE('',*,*,#12439,.T.);
#16502=ORIENTED_EDGE('',*,*,#12444,.F.);
#16503=ORIENTED_EDGE('',*,*,#12445,.F.);
#16504=ORIENTED_EDGE('',*,*,#12446,.T.);
#16505=ORIENTED_EDGE('',*,*,#12442,.T.);
#16506=ORIENTED_EDGE('',*,*,#12447,.F.);
#16507=ORIENTED_EDGE('',*,*,#12448,.F.);
#16508=ORIENTED_EDGE('',*,*,#12449,.T.);
#16509=ORIENTED_EDGE('',*,*,#12445,.T.);
#16510=ORIENTED_EDGE('',*,*,#12450,.F.);
#16511=ORIENTED_EDGE('',*,*,#12451,.F.);
#16512=ORIENTED_EDGE('',*,*,#12452,.T.);
#16513=ORIENTED_EDGE('',*,*,#12448,.T.);
#16514=ORIENTED_EDGE('',*,*,#12453,.F.);
#16515=ORIENTED_EDGE('',*,*,#12454,.F.);
#16516=ORIENTED_EDGE('',*,*,#12455,.T.);
#16517=ORIENTED_EDGE('',*,*,#12451,.T.);
#16518=ORIENTED_EDGE('',*,*,#12456,.F.);
#16519=ORIENTED_EDGE('',*,*,#12457,.F.);
#16520=ORIENTED_EDGE('',*,*,#12458,.T.);
#16521=ORIENTED_EDGE('',*,*,#12454,.T.);
#16522=ORIENTED_EDGE('',*,*,#12459,.F.);
#16523=ORIENTED_EDGE('',*,*,#12460,.F.);
#16524=ORIENTED_EDGE('',*,*,#12461,.T.);
#16525=ORIENTED_EDGE('',*,*,#12457,.T.);
#16526=ORIENTED_EDGE('',*,*,#12462,.F.);
#16527=ORIENTED_EDGE('',*,*,#12463,.F.);
#16528=ORIENTED_EDGE('',*,*,#12464,.T.);
#16529=ORIENTED_EDGE('',*,*,#12460,.T.);
#16530=ORIENTED_EDGE('',*,*,#12465,.F.);
#16531=ORIENTED_EDGE('',*,*,#12466,.F.);
#16532=ORIENTED_EDGE('',*,*,#12467,.T.);
#16533=ORIENTED_EDGE('',*,*,#12463,.T.);
#16534=ORIENTED_EDGE('',*,*,#12468,.F.);
#16535=ORIENTED_EDGE('',*,*,#12469,.F.);
#16536=ORIENTED_EDGE('',*,*,#12470,.F.);
#16537=ORIENTED_EDGE('',*,*,#12434,.F.);
#16538=ORIENTED_EDGE('',*,*,#12431,.F.);
#16539=ORIENTED_EDGE('',*,*,#12428,.F.);
#16540=ORIENTED_EDGE('',*,*,#12425,.F.);
#16541=ORIENTED_EDGE('',*,*,#12422,.F.);
#16542=ORIENTED_EDGE('',*,*,#12419,.F.);
#16543=ORIENTED_EDGE('',*,*,#12416,.F.);
#16544=ORIENTED_EDGE('',*,*,#12413,.F.);
#16545=ORIENTED_EDGE('',*,*,#12410,.F.);
#16546=ORIENTED_EDGE('',*,*,#12407,.F.);
#16547=ORIENTED_EDGE('',*,*,#12471,.F.);
#16548=ORIENTED_EDGE('',*,*,#12472,.T.);
#16549=ORIENTED_EDGE('',*,*,#12468,.T.);
#16550=ORIENTED_EDGE('',*,*,#12465,.T.);
#16551=ORIENTED_EDGE('',*,*,#12462,.T.);
#16552=ORIENTED_EDGE('',*,*,#12459,.T.);
#16553=ORIENTED_EDGE('',*,*,#12456,.T.);
#16554=ORIENTED_EDGE('',*,*,#12453,.T.);
#16555=ORIENTED_EDGE('',*,*,#12450,.T.);
#16556=ORIENTED_EDGE('',*,*,#12447,.T.);
#16557=ORIENTED_EDGE('',*,*,#12444,.T.);
#16558=ORIENTED_EDGE('',*,*,#12441,.T.);
#16559=ORIENTED_EDGE('',*,*,#12438,.T.);
#16560=ORIENTED_EDGE('',*,*,#12406,.F.);
#16561=ORIENTED_EDGE('',*,*,#12473,.T.);
#16562=ORIENTED_EDGE('',*,*,#12474,.T.);
#16563=ORIENTED_EDGE('',*,*,#12471,.T.);
#16564=ORIENTED_EDGE('',*,*,#12466,.T.);
#16565=ORIENTED_EDGE('',*,*,#12472,.F.);
#16566=ORIENTED_EDGE('',*,*,#12474,.F.);
#16567=ORIENTED_EDGE('',*,*,#12475,.T.);
#16568=ORIENTED_EDGE('',*,*,#12476,.F.);
#16569=ORIENTED_EDGE('',*,*,#12436,.F.);
#16570=ORIENTED_EDGE('',*,*,#12440,.F.);
#16571=ORIENTED_EDGE('',*,*,#12443,.F.);
#16572=ORIENTED_EDGE('',*,*,#12446,.F.);
#16573=ORIENTED_EDGE('',*,*,#12449,.F.);
#16574=ORIENTED_EDGE('',*,*,#12452,.F.);
#16575=ORIENTED_EDGE('',*,*,#12455,.F.);
#16576=ORIENTED_EDGE('',*,*,#12458,.F.);
#16577=ORIENTED_EDGE('',*,*,#12461,.F.);
#16578=ORIENTED_EDGE('',*,*,#12464,.F.);
#16579=ORIENTED_EDGE('',*,*,#12467,.F.);
#16580=ORIENTED_EDGE('',*,*,#12475,.F.);
#16581=ORIENTED_EDGE('',*,*,#12473,.F.);
#16582=ORIENTED_EDGE('',*,*,#12405,.F.);
#16583=ORIENTED_EDGE('',*,*,#12402,.F.);
#16584=ORIENTED_EDGE('',*,*,#12409,.F.);
#16585=ORIENTED_EDGE('',*,*,#12412,.F.);
#16586=ORIENTED_EDGE('',*,*,#12415,.F.);
#16587=ORIENTED_EDGE('',*,*,#12418,.F.);
#16588=ORIENTED_EDGE('',*,*,#12421,.F.);
#16589=ORIENTED_EDGE('',*,*,#12424,.F.);
#16590=ORIENTED_EDGE('',*,*,#12427,.F.);
#16591=ORIENTED_EDGE('',*,*,#12430,.F.);
#16592=ORIENTED_EDGE('',*,*,#12433,.F.);
#16593=ORIENTED_EDGE('',*,*,#12477,.F.);
#16594=ORIENTED_EDGE('',*,*,#12478,.F.);
#16595=ORIENTED_EDGE('',*,*,#12479,.T.);
#16596=ORIENTED_EDGE('',*,*,#12480,.F.);
#16597=ORIENTED_EDGE('',*,*,#12479,.F.);
#16598=ORIENTED_EDGE('',*,*,#12481,.F.);
#16599=ORIENTED_EDGE('',*,*,#12482,.T.);
#16600=ORIENTED_EDGE('',*,*,#12483,.F.);
#16601=ORIENTED_EDGE('',*,*,#12482,.F.);
#16602=ORIENTED_EDGE('',*,*,#12484,.F.);
#16603=ORIENTED_EDGE('',*,*,#12485,.T.);
#16604=ORIENTED_EDGE('',*,*,#12486,.F.);
#16605=ORIENTED_EDGE('',*,*,#12485,.F.);
#16606=ORIENTED_EDGE('',*,*,#12487,.F.);
#16607=ORIENTED_EDGE('',*,*,#12488,.T.);
#16608=ORIENTED_EDGE('',*,*,#12489,.F.);
#16609=ORIENTED_EDGE('',*,*,#12488,.F.);
#16610=ORIENTED_EDGE('',*,*,#12490,.F.);
#16611=ORIENTED_EDGE('',*,*,#12491,.F.);
#16612=ORIENTED_EDGE('',*,*,#12492,.T.);
#16613=ORIENTED_EDGE('',*,*,#12493,.T.);
#16614=ORIENTED_EDGE('',*,*,#12494,.F.);
#16615=ORIENTED_EDGE('',*,*,#12493,.F.);
#16616=ORIENTED_EDGE('',*,*,#12495,.F.);
#16617=ORIENTED_EDGE('',*,*,#12496,.F.);
#16618=ORIENTED_EDGE('',*,*,#12495,.T.);
#16619=ORIENTED_EDGE('',*,*,#12492,.F.);
#16620=ORIENTED_EDGE('',*,*,#12497,.F.);
#16621=ORIENTED_EDGE('',*,*,#12498,.F.);
#16622=ORIENTED_EDGE('',*,*,#12497,.T.);
#16623=ORIENTED_EDGE('',*,*,#12491,.T.);
#16624=ORIENTED_EDGE('',*,*,#12499,.F.);
#16625=ORIENTED_EDGE('',*,*,#12500,.F.);
#16626=ORIENTED_EDGE('',*,*,#12501,.T.);
#16627=ORIENTED_EDGE('',*,*,#12502,.T.);
#16628=ORIENTED_EDGE('',*,*,#12503,.F.);
#16629=ORIENTED_EDGE('',*,*,#12502,.F.);
#16630=ORIENTED_EDGE('',*,*,#12504,.F.);
#16631=ORIENTED_EDGE('',*,*,#12505,.F.);
#16632=ORIENTED_EDGE('',*,*,#12504,.T.);
#16633=ORIENTED_EDGE('',*,*,#12501,.F.);
#16634=ORIENTED_EDGE('',*,*,#12506,.F.);
#16635=ORIENTED_EDGE('',*,*,#12507,.F.);
#16636=ORIENTED_EDGE('',*,*,#12506,.T.);
#16637=ORIENTED_EDGE('',*,*,#12500,.T.);
#16638=ORIENTED_EDGE('',*,*,#12508,.F.);
#16639=ORIENTED_EDGE('',*,*,#12509,.F.);
#16640=ORIENTED_EDGE('',*,*,#12510,.T.);
#16641=ORIENTED_EDGE('',*,*,#12511,.T.);
#16642=ORIENTED_EDGE('',*,*,#12512,.F.);
#16643=ORIENTED_EDGE('',*,*,#12511,.F.);
#16644=ORIENTED_EDGE('',*,*,#12513,.F.);
#16645=ORIENTED_EDGE('',*,*,#12514,.F.);
#16646=ORIENTED_EDGE('',*,*,#12513,.T.);
#16647=ORIENTED_EDGE('',*,*,#12510,.F.);
#16648=ORIENTED_EDGE('',*,*,#12515,.F.);
#16649=ORIENTED_EDGE('',*,*,#12516,.F.);
#16650=ORIENTED_EDGE('',*,*,#12515,.T.);
#16651=ORIENTED_EDGE('',*,*,#12509,.T.);
#16652=ORIENTED_EDGE('',*,*,#12517,.F.);
#16653=ORIENTED_EDGE('',*,*,#12518,.F.);
#16654=ORIENTED_EDGE('',*,*,#12519,.T.);
#16655=ORIENTED_EDGE('',*,*,#12520,.T.);
#16656=ORIENTED_EDGE('',*,*,#12521,.F.);
#16657=ORIENTED_EDGE('',*,*,#12520,.F.);
#16658=ORIENTED_EDGE('',*,*,#12522,.F.);
#16659=ORIENTED_EDGE('',*,*,#12523,.F.);
#16660=ORIENTED_EDGE('',*,*,#12522,.T.);
#16661=ORIENTED_EDGE('',*,*,#12519,.F.);
#16662=ORIENTED_EDGE('',*,*,#12524,.F.);
#16663=ORIENTED_EDGE('',*,*,#12525,.F.);
#16664=ORIENTED_EDGE('',*,*,#12524,.T.);
#16665=ORIENTED_EDGE('',*,*,#12518,.T.);
#16666=ORIENTED_EDGE('',*,*,#12526,.F.);
#16667=ORIENTED_EDGE('',*,*,#12527,.F.);
#16668=ORIENTED_EDGE('',*,*,#12528,.T.);
#16669=ORIENTED_EDGE('',*,*,#12529,.T.);
#16670=ORIENTED_EDGE('',*,*,#12530,.F.);
#16671=ORIENTED_EDGE('',*,*,#12529,.F.);
#16672=ORIENTED_EDGE('',*,*,#12531,.F.);
#16673=ORIENTED_EDGE('',*,*,#12532,.F.);
#16674=ORIENTED_EDGE('',*,*,#12531,.T.);
#16675=ORIENTED_EDGE('',*,*,#12528,.F.);
#16676=ORIENTED_EDGE('',*,*,#12533,.F.);
#16677=ORIENTED_EDGE('',*,*,#12534,.F.);
#16678=ORIENTED_EDGE('',*,*,#12533,.T.);
#16679=ORIENTED_EDGE('',*,*,#12527,.T.);
#16680=ORIENTED_EDGE('',*,*,#12535,.F.);
#16681=ORIENTED_EDGE('',*,*,#12536,.F.);
#16682=ORIENTED_EDGE('',*,*,#12537,.T.);
#16683=ORIENTED_EDGE('',*,*,#12538,.T.);
#16684=ORIENTED_EDGE('',*,*,#12539,.F.);
#16685=ORIENTED_EDGE('',*,*,#12538,.F.);
#16686=ORIENTED_EDGE('',*,*,#12540,.F.);
#16687=ORIENTED_EDGE('',*,*,#12541,.F.);
#16688=ORIENTED_EDGE('',*,*,#12540,.T.);
#16689=ORIENTED_EDGE('',*,*,#12537,.F.);
#16690=ORIENTED_EDGE('',*,*,#12542,.F.);
#16691=ORIENTED_EDGE('',*,*,#12543,.F.);
#16692=ORIENTED_EDGE('',*,*,#12542,.T.);
#16693=ORIENTED_EDGE('',*,*,#12536,.T.);
#16694=ORIENTED_EDGE('',*,*,#12544,.F.);
#16695=ORIENTED_EDGE('',*,*,#12545,.F.);
#16696=ORIENTED_EDGE('',*,*,#12546,.T.);
#16697=ORIENTED_EDGE('',*,*,#12547,.T.);
#16698=ORIENTED_EDGE('',*,*,#12548,.F.);
#16699=ORIENTED_EDGE('',*,*,#12547,.F.);
#16700=ORIENTED_EDGE('',*,*,#12549,.F.);
#16701=ORIENTED_EDGE('',*,*,#12550,.F.);
#16702=ORIENTED_EDGE('',*,*,#12549,.T.);
#16703=ORIENTED_EDGE('',*,*,#12546,.F.);
#16704=ORIENTED_EDGE('',*,*,#12551,.F.);
#16705=ORIENTED_EDGE('',*,*,#12552,.F.);
#16706=ORIENTED_EDGE('',*,*,#12551,.T.);
#16707=ORIENTED_EDGE('',*,*,#12545,.T.);
#16708=ORIENTED_EDGE('',*,*,#12553,.F.);
#16709=ORIENTED_EDGE('',*,*,#12554,.F.);
#16710=ORIENTED_EDGE('',*,*,#12555,.T.);
#16711=ORIENTED_EDGE('',*,*,#12556,.T.);
#16712=ORIENTED_EDGE('',*,*,#12557,.F.);
#16713=ORIENTED_EDGE('',*,*,#12556,.F.);
#16714=ORIENTED_EDGE('',*,*,#12558,.F.);
#16715=ORIENTED_EDGE('',*,*,#12559,.F.);
#16716=ORIENTED_EDGE('',*,*,#12558,.T.);
#16717=ORIENTED_EDGE('',*,*,#12555,.F.);
#16718=ORIENTED_EDGE('',*,*,#12560,.F.);
#16719=ORIENTED_EDGE('',*,*,#12561,.F.);
#16720=ORIENTED_EDGE('',*,*,#12560,.T.);
#16721=ORIENTED_EDGE('',*,*,#12554,.T.);
#16722=ORIENTED_EDGE('',*,*,#12562,.F.);
#16723=ORIENTED_EDGE('',*,*,#12563,.F.);
#16724=ORIENTED_EDGE('',*,*,#12564,.T.);
#16725=ORIENTED_EDGE('',*,*,#12565,.T.);
#16726=ORIENTED_EDGE('',*,*,#12566,.F.);
#16727=ORIENTED_EDGE('',*,*,#12565,.F.);
#16728=ORIENTED_EDGE('',*,*,#12567,.F.);
#16729=ORIENTED_EDGE('',*,*,#12568,.F.);
#16730=ORIENTED_EDGE('',*,*,#12567,.T.);
#16731=ORIENTED_EDGE('',*,*,#12564,.F.);
#16732=ORIENTED_EDGE('',*,*,#12569,.F.);
#16733=ORIENTED_EDGE('',*,*,#12570,.F.);
#16734=ORIENTED_EDGE('',*,*,#12569,.T.);
#16735=ORIENTED_EDGE('',*,*,#12563,.T.);
#16736=ORIENTED_EDGE('',*,*,#12571,.F.);
#16737=ORIENTED_EDGE('',*,*,#12572,.F.);
#16738=ORIENTED_EDGE('',*,*,#12573,.T.);
#16739=ORIENTED_EDGE('',*,*,#12574,.T.);
#16740=ORIENTED_EDGE('',*,*,#12575,.F.);
#16741=ORIENTED_EDGE('',*,*,#12574,.F.);
#16742=ORIENTED_EDGE('',*,*,#12576,.F.);
#16743=ORIENTED_EDGE('',*,*,#12577,.F.);
#16744=ORIENTED_EDGE('',*,*,#12576,.T.);
#16745=ORIENTED_EDGE('',*,*,#12573,.F.);
#16746=ORIENTED_EDGE('',*,*,#12578,.F.);
#16747=ORIENTED_EDGE('',*,*,#12579,.F.);
#16748=ORIENTED_EDGE('',*,*,#12578,.T.);
#16749=ORIENTED_EDGE('',*,*,#12572,.T.);
#16750=ORIENTED_EDGE('',*,*,#12580,.F.);
#16751=ORIENTED_EDGE('',*,*,#12581,.F.);
#16752=ORIENTED_EDGE('',*,*,#12582,.T.);
#16753=ORIENTED_EDGE('',*,*,#12583,.T.);
#16754=ORIENTED_EDGE('',*,*,#12584,.F.);
#16755=ORIENTED_EDGE('',*,*,#12583,.F.);
#16756=ORIENTED_EDGE('',*,*,#12585,.F.);
#16757=ORIENTED_EDGE('',*,*,#12586,.F.);
#16758=ORIENTED_EDGE('',*,*,#12585,.T.);
#16759=ORIENTED_EDGE('',*,*,#12582,.F.);
#16760=ORIENTED_EDGE('',*,*,#12587,.F.);
#16761=ORIENTED_EDGE('',*,*,#12588,.F.);
#16762=ORIENTED_EDGE('',*,*,#12587,.T.);
#16763=ORIENTED_EDGE('',*,*,#12581,.T.);
#16764=ORIENTED_EDGE('',*,*,#12589,.F.);
#16765=ORIENTED_EDGE('',*,*,#12590,.F.);
#16766=ORIENTED_EDGE('',*,*,#12591,.T.);
#16767=ORIENTED_EDGE('',*,*,#12592,.T.);
#16768=ORIENTED_EDGE('',*,*,#12593,.F.);
#16769=ORIENTED_EDGE('',*,*,#12592,.F.);
#16770=ORIENTED_EDGE('',*,*,#12594,.F.);
#16771=ORIENTED_EDGE('',*,*,#12595,.F.);
#16772=ORIENTED_EDGE('',*,*,#12596,.F.);
#16773=ORIENTED_EDGE('',*,*,#12594,.T.);
#16774=ORIENTED_EDGE('',*,*,#12591,.F.);
#16775=ORIENTED_EDGE('',*,*,#12597,.F.);
#16776=ORIENTED_EDGE('',*,*,#12598,.F.);
#16777=ORIENTED_EDGE('',*,*,#12597,.T.);
#16778=ORIENTED_EDGE('',*,*,#12590,.T.);
#16779=ORIENTED_EDGE('',*,*,#12599,.F.);
#16780=ORIENTED_EDGE('',*,*,#12600,.F.);
#16781=ORIENTED_EDGE('',*,*,#12601,.F.);
#16782=ORIENTED_EDGE('',*,*,#12602,.T.);
#16783=ORIENTED_EDGE('',*,*,#12603,.T.);
#16784=ORIENTED_EDGE('',*,*,#12604,.F.);
#16785=ORIENTED_EDGE('',*,*,#12603,.F.);
#16786=ORIENTED_EDGE('',*,*,#12605,.F.);
#16787=ORIENTED_EDGE('',*,*,#12606,.F.);
#16788=ORIENTED_EDGE('',*,*,#12605,.T.);
#16789=ORIENTED_EDGE('',*,*,#12602,.F.);
#16790=ORIENTED_EDGE('',*,*,#12607,.F.);
#16791=ORIENTED_EDGE('',*,*,#12608,.F.);
#16792=ORIENTED_EDGE('',*,*,#12607,.T.);
#16793=ORIENTED_EDGE('',*,*,#12601,.T.);
#16794=ORIENTED_EDGE('',*,*,#12609,.F.);
#16795=ORIENTED_EDGE('',*,*,#12610,.F.);
#16796=ORIENTED_EDGE('',*,*,#12611,.T.);
#16797=ORIENTED_EDGE('',*,*,#12612,.T.);
#16798=ORIENTED_EDGE('',*,*,#12613,.F.);
#16799=ORIENTED_EDGE('',*,*,#12612,.F.);
#16800=ORIENTED_EDGE('',*,*,#12614,.F.);
#16801=ORIENTED_EDGE('',*,*,#12615,.F.);
#16802=ORIENTED_EDGE('',*,*,#12614,.T.);
#16803=ORIENTED_EDGE('',*,*,#12611,.F.);
#16804=ORIENTED_EDGE('',*,*,#12616,.F.);
#16805=ORIENTED_EDGE('',*,*,#12617,.F.);
#16806=ORIENTED_EDGE('',*,*,#12616,.T.);
#16807=ORIENTED_EDGE('',*,*,#12610,.T.);
#16808=ORIENTED_EDGE('',*,*,#12618,.F.);
#16809=ORIENTED_EDGE('',*,*,#12619,.F.);
#16810=ORIENTED_EDGE('',*,*,#12620,.T.);
#16811=ORIENTED_EDGE('',*,*,#12621,.T.);
#16812=ORIENTED_EDGE('',*,*,#12622,.F.);
#16813=ORIENTED_EDGE('',*,*,#12621,.F.);
#16814=ORIENTED_EDGE('',*,*,#12623,.F.);
#16815=ORIENTED_EDGE('',*,*,#12624,.F.);
#16816=ORIENTED_EDGE('',*,*,#12623,.T.);
#16817=ORIENTED_EDGE('',*,*,#12620,.F.);
#16818=ORIENTED_EDGE('',*,*,#12625,.F.);
#16819=ORIENTED_EDGE('',*,*,#12626,.F.);
#16820=ORIENTED_EDGE('',*,*,#12625,.T.);
#16821=ORIENTED_EDGE('',*,*,#12619,.T.);
#16822=ORIENTED_EDGE('',*,*,#12627,.F.);
#16823=ORIENTED_EDGE('',*,*,#12628,.F.);
#16824=ORIENTED_EDGE('',*,*,#12629,.T.);
#16825=ORIENTED_EDGE('',*,*,#12630,.T.);
#16826=ORIENTED_EDGE('',*,*,#12631,.F.);
#16827=ORIENTED_EDGE('',*,*,#12630,.F.);
#16828=ORIENTED_EDGE('',*,*,#12632,.F.);
#16829=ORIENTED_EDGE('',*,*,#12633,.F.);
#16830=ORIENTED_EDGE('',*,*,#12632,.T.);
#16831=ORIENTED_EDGE('',*,*,#12629,.F.);
#16832=ORIENTED_EDGE('',*,*,#12634,.F.);
#16833=ORIENTED_EDGE('',*,*,#12635,.F.);
#16834=ORIENTED_EDGE('',*,*,#12634,.T.);
#16835=ORIENTED_EDGE('',*,*,#12628,.T.);
#16836=ORIENTED_EDGE('',*,*,#12636,.F.);
#16837=ORIENTED_EDGE('',*,*,#12637,.F.);
#16838=ORIENTED_EDGE('',*,*,#12638,.T.);
#16839=ORIENTED_EDGE('',*,*,#12639,.T.);
#16840=ORIENTED_EDGE('',*,*,#12640,.F.);
#16841=ORIENTED_EDGE('',*,*,#12639,.F.);
#16842=ORIENTED_EDGE('',*,*,#12641,.F.);
#16843=ORIENTED_EDGE('',*,*,#12642,.F.);
#16844=ORIENTED_EDGE('',*,*,#12641,.T.);
#16845=ORIENTED_EDGE('',*,*,#12638,.F.);
#16846=ORIENTED_EDGE('',*,*,#12643,.F.);
#16847=ORIENTED_EDGE('',*,*,#12644,.F.);
#16848=ORIENTED_EDGE('',*,*,#12643,.T.);
#16849=ORIENTED_EDGE('',*,*,#12637,.T.);
#16850=ORIENTED_EDGE('',*,*,#12645,.F.);
#16851=ORIENTED_EDGE('',*,*,#12646,.F.);
#16852=ORIENTED_EDGE('',*,*,#12647,.T.);
#16853=ORIENTED_EDGE('',*,*,#12648,.T.);
#16854=ORIENTED_EDGE('',*,*,#12649,.F.);
#16855=ORIENTED_EDGE('',*,*,#12648,.F.);
#16856=ORIENTED_EDGE('',*,*,#12650,.F.);
#16857=ORIENTED_EDGE('',*,*,#12651,.F.);
#16858=ORIENTED_EDGE('',*,*,#12650,.T.);
#16859=ORIENTED_EDGE('',*,*,#12647,.F.);
#16860=ORIENTED_EDGE('',*,*,#12652,.F.);
#16861=ORIENTED_EDGE('',*,*,#12653,.F.);
#16862=ORIENTED_EDGE('',*,*,#12652,.T.);
#16863=ORIENTED_EDGE('',*,*,#12646,.T.);
#16864=ORIENTED_EDGE('',*,*,#12654,.F.);
#16865=ORIENTED_EDGE('',*,*,#12655,.F.);
#16866=ORIENTED_EDGE('',*,*,#12656,.T.);
#16867=ORIENTED_EDGE('',*,*,#12657,.T.);
#16868=ORIENTED_EDGE('',*,*,#12658,.F.);
#16869=ORIENTED_EDGE('',*,*,#12657,.F.);
#16870=ORIENTED_EDGE('',*,*,#12659,.F.);
#16871=ORIENTED_EDGE('',*,*,#12660,.F.);
#16872=ORIENTED_EDGE('',*,*,#12659,.T.);
#16873=ORIENTED_EDGE('',*,*,#12656,.F.);
#16874=ORIENTED_EDGE('',*,*,#12661,.F.);
#16875=ORIENTED_EDGE('',*,*,#12662,.F.);
#16876=ORIENTED_EDGE('',*,*,#12661,.T.);
#16877=ORIENTED_EDGE('',*,*,#12655,.T.);
#16878=ORIENTED_EDGE('',*,*,#12663,.F.);
#16879=ORIENTED_EDGE('',*,*,#12664,.F.);
#16880=ORIENTED_EDGE('',*,*,#12665,.T.);
#16881=ORIENTED_EDGE('',*,*,#12666,.T.);
#16882=ORIENTED_EDGE('',*,*,#12667,.F.);
#16883=ORIENTED_EDGE('',*,*,#12666,.F.);
#16884=ORIENTED_EDGE('',*,*,#12668,.F.);
#16885=ORIENTED_EDGE('',*,*,#12669,.F.);
#16886=ORIENTED_EDGE('',*,*,#12668,.T.);
#16887=ORIENTED_EDGE('',*,*,#12665,.F.);
#16888=ORIENTED_EDGE('',*,*,#12670,.F.);
#16889=ORIENTED_EDGE('',*,*,#12671,.F.);
#16890=ORIENTED_EDGE('',*,*,#12670,.T.);
#16891=ORIENTED_EDGE('',*,*,#12664,.T.);
#16892=ORIENTED_EDGE('',*,*,#12672,.F.);
#16893=ORIENTED_EDGE('',*,*,#12673,.F.);
#16894=ORIENTED_EDGE('',*,*,#12674,.T.);
#16895=ORIENTED_EDGE('',*,*,#12675,.T.);
#16896=ORIENTED_EDGE('',*,*,#12676,.F.);
#16897=ORIENTED_EDGE('',*,*,#12675,.F.);
#16898=ORIENTED_EDGE('',*,*,#12677,.F.);
#16899=ORIENTED_EDGE('',*,*,#12678,.F.);
#16900=ORIENTED_EDGE('',*,*,#12677,.T.);
#16901=ORIENTED_EDGE('',*,*,#12674,.F.);
#16902=ORIENTED_EDGE('',*,*,#12679,.F.);
#16903=ORIENTED_EDGE('',*,*,#12680,.F.);
#16904=ORIENTED_EDGE('',*,*,#12679,.T.);
#16905=ORIENTED_EDGE('',*,*,#12673,.T.);
#16906=ORIENTED_EDGE('',*,*,#12681,.F.);
#16907=ORIENTED_EDGE('',*,*,#12682,.F.);
#16908=ORIENTED_EDGE('',*,*,#12683,.T.);
#16909=ORIENTED_EDGE('',*,*,#12684,.T.);
#16910=ORIENTED_EDGE('',*,*,#12685,.F.);
#16911=ORIENTED_EDGE('',*,*,#12684,.F.);
#16912=ORIENTED_EDGE('',*,*,#12686,.F.);
#16913=ORIENTED_EDGE('',*,*,#12687,.F.);
#16914=ORIENTED_EDGE('',*,*,#12686,.T.);
#16915=ORIENTED_EDGE('',*,*,#12683,.F.);
#16916=ORIENTED_EDGE('',*,*,#12688,.F.);
#16917=ORIENTED_EDGE('',*,*,#12689,.F.);
#16918=ORIENTED_EDGE('',*,*,#12688,.T.);
#16919=ORIENTED_EDGE('',*,*,#12682,.T.);
#16920=ORIENTED_EDGE('',*,*,#12690,.F.);
#16921=ORIENTED_EDGE('',*,*,#12691,.F.);
#16922=ORIENTED_EDGE('',*,*,#12692,.T.);
#16923=ORIENTED_EDGE('',*,*,#12693,.T.);
#16924=ORIENTED_EDGE('',*,*,#12694,.F.);
#16925=ORIENTED_EDGE('',*,*,#12693,.F.);
#16926=ORIENTED_EDGE('',*,*,#12695,.F.);
#16927=ORIENTED_EDGE('',*,*,#12696,.F.);
#16928=ORIENTED_EDGE('',*,*,#12695,.T.);
#16929=ORIENTED_EDGE('',*,*,#12692,.F.);
#16930=ORIENTED_EDGE('',*,*,#12697,.F.);
#16931=ORIENTED_EDGE('',*,*,#12698,.F.);
#16932=ORIENTED_EDGE('',*,*,#12697,.T.);
#16933=ORIENTED_EDGE('',*,*,#12691,.T.);
#16934=ORIENTED_EDGE('',*,*,#12699,.F.);
#16935=ORIENTED_EDGE('',*,*,#12700,.F.);
#16936=ORIENTED_EDGE('',*,*,#12701,.T.);
#16937=ORIENTED_EDGE('',*,*,#12702,.T.);
#16938=ORIENTED_EDGE('',*,*,#12703,.F.);
#16939=ORIENTED_EDGE('',*,*,#12702,.F.);
#16940=ORIENTED_EDGE('',*,*,#12704,.F.);
#16941=ORIENTED_EDGE('',*,*,#12705,.F.);
#16942=ORIENTED_EDGE('',*,*,#12704,.T.);
#16943=ORIENTED_EDGE('',*,*,#12701,.F.);
#16944=ORIENTED_EDGE('',*,*,#12706,.F.);
#16945=ORIENTED_EDGE('',*,*,#12707,.F.);
#16946=ORIENTED_EDGE('',*,*,#12706,.T.);
#16947=ORIENTED_EDGE('',*,*,#12700,.T.);
#16948=ORIENTED_EDGE('',*,*,#12708,.F.);
#16949=ORIENTED_EDGE('',*,*,#12709,.T.);
#16950=ORIENTED_EDGE('',*,*,#12710,.F.);
#16951=ORIENTED_EDGE('',*,*,#12709,.F.);
#16952=ORIENTED_EDGE('',*,*,#12711,.F.);
#16953=ORIENTED_EDGE('',*,*,#12712,.T.);
#16954=ORIENTED_EDGE('',*,*,#12708,.T.);
#16955=ORIENTED_EDGE('',*,*,#12712,.F.);
#16956=ORIENTED_EDGE('',*,*,#12711,.T.);
#16957=ORIENTED_EDGE('',*,*,#12713,.T.);
#16958=ORIENTED_EDGE('',*,*,#12710,.T.);
#16959=ORIENTED_EDGE('',*,*,#12713,.F.);
#16960=ORIENTED_EDGE('',*,*,#12714,.T.);
#16961=ORIENTED_EDGE('',*,*,#12715,.F.);
#16962=ORIENTED_EDGE('',*,*,#12714,.F.);
#16963=ORIENTED_EDGE('',*,*,#12716,.F.);
#16964=ORIENTED_EDGE('',*,*,#12717,.T.);
#16965=ORIENTED_EDGE('',*,*,#12595,.T.);
#16966=ORIENTED_EDGE('',*,*,#12596,.T.);
#16967=ORIENTED_EDGE('',*,*,#12598,.T.);
#16968=ORIENTED_EDGE('',*,*,#12718,.T.);
#16969=ORIENTED_EDGE('',*,*,#12719,.F.);
#16970=ORIENTED_EDGE('',*,*,#12718,.F.);
#16971=ORIENTED_EDGE('',*,*,#12599,.T.);
#16972=ORIENTED_EDGE('',*,*,#12589,.T.);
#16973=ORIENTED_EDGE('',*,*,#12593,.T.);
#16974=ORIENTED_EDGE('',*,*,#12717,.F.);
#16975=ORIENTED_EDGE('',*,*,#12496,.T.);
#16976=ORIENTED_EDGE('',*,*,#12498,.T.);
#16977=ORIENTED_EDGE('',*,*,#12490,.T.);
#16978=ORIENTED_EDGE('',*,*,#12494,.T.);
#16979=ORIENTED_EDGE('',*,*,#12505,.T.);
#16980=ORIENTED_EDGE('',*,*,#12507,.T.);
#16981=ORIENTED_EDGE('',*,*,#12499,.T.);
#16982=ORIENTED_EDGE('',*,*,#12503,.T.);
#16983=ORIENTED_EDGE('',*,*,#12514,.T.);
#16984=ORIENTED_EDGE('',*,*,#12516,.T.);
#16985=ORIENTED_EDGE('',*,*,#12508,.T.);
#16986=ORIENTED_EDGE('',*,*,#12512,.T.);
#16987=ORIENTED_EDGE('',*,*,#12523,.T.);
#16988=ORIENTED_EDGE('',*,*,#12525,.T.);
#16989=ORIENTED_EDGE('',*,*,#12517,.T.);
#16990=ORIENTED_EDGE('',*,*,#12521,.T.);
#16991=ORIENTED_EDGE('',*,*,#12532,.T.);
#16992=ORIENTED_EDGE('',*,*,#12534,.T.);
#16993=ORIENTED_EDGE('',*,*,#12526,.T.);
#16994=ORIENTED_EDGE('',*,*,#12530,.T.);
#16995=ORIENTED_EDGE('',*,*,#12541,.T.);
#16996=ORIENTED_EDGE('',*,*,#12543,.T.);
#16997=ORIENTED_EDGE('',*,*,#12535,.T.);
#16998=ORIENTED_EDGE('',*,*,#12539,.T.);
#16999=ORIENTED_EDGE('',*,*,#12550,.T.);
#17000=ORIENTED_EDGE('',*,*,#12552,.T.);
#17001=ORIENTED_EDGE('',*,*,#12544,.T.);
#17002=ORIENTED_EDGE('',*,*,#12548,.T.);
#17003=ORIENTED_EDGE('',*,*,#12559,.T.);
#17004=ORIENTED_EDGE('',*,*,#12561,.T.);
#17005=ORIENTED_EDGE('',*,*,#12553,.T.);
#17006=ORIENTED_EDGE('',*,*,#12557,.T.);
#17007=ORIENTED_EDGE('',*,*,#12568,.T.);
#17008=ORIENTED_EDGE('',*,*,#12570,.T.);
#17009=ORIENTED_EDGE('',*,*,#12562,.T.);
#17010=ORIENTED_EDGE('',*,*,#12566,.T.);
#17011=ORIENTED_EDGE('',*,*,#12577,.T.);
#17012=ORIENTED_EDGE('',*,*,#12579,.T.);
#17013=ORIENTED_EDGE('',*,*,#12571,.T.);
#17014=ORIENTED_EDGE('',*,*,#12575,.T.);
#17015=ORIENTED_EDGE('',*,*,#12586,.T.);
#17016=ORIENTED_EDGE('',*,*,#12588,.T.);
#17017=ORIENTED_EDGE('',*,*,#12580,.T.);
#17018=ORIENTED_EDGE('',*,*,#12584,.T.);
#17019=ORIENTED_EDGE('',*,*,#12606,.T.);
#17020=ORIENTED_EDGE('',*,*,#12608,.T.);
#17021=ORIENTED_EDGE('',*,*,#12600,.T.);
#17022=ORIENTED_EDGE('',*,*,#12604,.T.);
#17023=ORIENTED_EDGE('',*,*,#12615,.T.);
#17024=ORIENTED_EDGE('',*,*,#12617,.T.);
#17025=ORIENTED_EDGE('',*,*,#12609,.T.);
#17026=ORIENTED_EDGE('',*,*,#12613,.T.);
#17027=ORIENTED_EDGE('',*,*,#12624,.T.);
#17028=ORIENTED_EDGE('',*,*,#12626,.T.);
#17029=ORIENTED_EDGE('',*,*,#12618,.T.);
#17030=ORIENTED_EDGE('',*,*,#12622,.T.);
#17031=ORIENTED_EDGE('',*,*,#12633,.T.);
#17032=ORIENTED_EDGE('',*,*,#12635,.T.);
#17033=ORIENTED_EDGE('',*,*,#12627,.T.);
#17034=ORIENTED_EDGE('',*,*,#12631,.T.);
#17035=ORIENTED_EDGE('',*,*,#12642,.T.);
#17036=ORIENTED_EDGE('',*,*,#12644,.T.);
#17037=ORIENTED_EDGE('',*,*,#12636,.T.);
#17038=ORIENTED_EDGE('',*,*,#12640,.T.);
#17039=ORIENTED_EDGE('',*,*,#12651,.T.);
#17040=ORIENTED_EDGE('',*,*,#12653,.T.);
#17041=ORIENTED_EDGE('',*,*,#12645,.T.);
#17042=ORIENTED_EDGE('',*,*,#12649,.T.);
#17043=ORIENTED_EDGE('',*,*,#12660,.T.);
#17044=ORIENTED_EDGE('',*,*,#12662,.T.);
#17045=ORIENTED_EDGE('',*,*,#12654,.T.);
#17046=ORIENTED_EDGE('',*,*,#12658,.T.);
#17047=ORIENTED_EDGE('',*,*,#12669,.T.);
#17048=ORIENTED_EDGE('',*,*,#12671,.T.);
#17049=ORIENTED_EDGE('',*,*,#12663,.T.);
#17050=ORIENTED_EDGE('',*,*,#12667,.T.);
#17051=ORIENTED_EDGE('',*,*,#12678,.T.);
#17052=ORIENTED_EDGE('',*,*,#12680,.T.);
#17053=ORIENTED_EDGE('',*,*,#12672,.T.);
#17054=ORIENTED_EDGE('',*,*,#12676,.T.);
#17055=ORIENTED_EDGE('',*,*,#12687,.T.);
#17056=ORIENTED_EDGE('',*,*,#12689,.T.);
#17057=ORIENTED_EDGE('',*,*,#12681,.T.);
#17058=ORIENTED_EDGE('',*,*,#12685,.T.);
#17059=ORIENTED_EDGE('',*,*,#12696,.T.);
#17060=ORIENTED_EDGE('',*,*,#12698,.T.);
#17061=ORIENTED_EDGE('',*,*,#12690,.T.);
#17062=ORIENTED_EDGE('',*,*,#12694,.T.);
#17063=ORIENTED_EDGE('',*,*,#12705,.T.);
#17064=ORIENTED_EDGE('',*,*,#12707,.T.);
#17065=ORIENTED_EDGE('',*,*,#12699,.T.);
#17066=ORIENTED_EDGE('',*,*,#12703,.T.);
#17067=ORIENTED_EDGE('',*,*,#12720,.F.);
#17068=ORIENTED_EDGE('',*,*,#12716,.T.);
#17069=ORIENTED_EDGE('',*,*,#12721,.F.);
#17070=ORIENTED_EDGE('',*,*,#12722,.T.);
#17071=ORIENTED_EDGE('',*,*,#12720,.T.);
#17072=ORIENTED_EDGE('',*,*,#12722,.F.);
#17073=ORIENTED_EDGE('',*,*,#12723,.F.);
#17074=ORIENTED_EDGE('',*,*,#12724,.T.);
#17075=ORIENTED_EDGE('',*,*,#12721,.T.);
#17076=ORIENTED_EDGE('',*,*,#12724,.F.);
#17077=ORIENTED_EDGE('',*,*,#12723,.T.);
#17078=ORIENTED_EDGE('',*,*,#12715,.T.);
#17079=ORIENTED_EDGE('',*,*,#12725,.F.);
#17080=ORIENTED_EDGE('',*,*,#12726,.T.);
#17081=ORIENTED_EDGE('',*,*,#12727,.F.);
#17082=ORIENTED_EDGE('',*,*,#12728,.F.);
#17083=ORIENTED_EDGE('',*,*,#12729,.F.);
#17084=ORIENTED_EDGE('',*,*,#12728,.T.);
#17085=ORIENTED_EDGE('',*,*,#12730,.F.);
#17086=ORIENTED_EDGE('',*,*,#12731,.F.);
#17087=ORIENTED_EDGE('',*,*,#12732,.F.);
#17088=ORIENTED_EDGE('',*,*,#12731,.T.);
#17089=ORIENTED_EDGE('',*,*,#12733,.F.);
#17090=ORIENTED_EDGE('',*,*,#12734,.F.);
#17091=ORIENTED_EDGE('',*,*,#12735,.F.);
#17092=ORIENTED_EDGE('',*,*,#12734,.T.);
#17093=ORIENTED_EDGE('',*,*,#12736,.F.);
#17094=ORIENTED_EDGE('',*,*,#12737,.F.);
#17095=ORIENTED_EDGE('',*,*,#12738,.F.);
#17096=ORIENTED_EDGE('',*,*,#12737,.T.);
#17097=ORIENTED_EDGE('',*,*,#12739,.F.);
#17098=ORIENTED_EDGE('',*,*,#12740,.F.);
#17099=ORIENTED_EDGE('',*,*,#12741,.F.);
#17100=ORIENTED_EDGE('',*,*,#12740,.T.);
#17101=ORIENTED_EDGE('',*,*,#12742,.F.);
#17102=ORIENTED_EDGE('',*,*,#12726,.F.);
#17103=ORIENTED_EDGE('',*,*,#12742,.T.);
#17104=ORIENTED_EDGE('',*,*,#12739,.T.);
#17105=ORIENTED_EDGE('',*,*,#12736,.T.);
#17106=ORIENTED_EDGE('',*,*,#12733,.T.);
#17107=ORIENTED_EDGE('',*,*,#12730,.T.);
#17108=ORIENTED_EDGE('',*,*,#12727,.T.);
#17109=ORIENTED_EDGE('',*,*,#12719,.T.);
#17110=ORIENTED_EDGE('',*,*,#12743,.F.);
#17111=ORIENTED_EDGE('',*,*,#12744,.F.);
#17112=ORIENTED_EDGE('',*,*,#12745,.F.);
#17113=ORIENTED_EDGE('',*,*,#12746,.F.);
#17114=ORIENTED_EDGE('',*,*,#12478,.T.);
#17115=ORIENTED_EDGE('',*,*,#12481,.T.);
#17116=ORIENTED_EDGE('',*,*,#12484,.T.);
#17117=ORIENTED_EDGE('',*,*,#12487,.T.);
#17118=ORIENTED_EDGE('',*,*,#12747,.T.);
#17119=ORIENTED_EDGE('',*,*,#12469,.T.);
#17120=ORIENTED_EDGE('',*,*,#12437,.T.);
#17121=ORIENTED_EDGE('',*,*,#12476,.T.);
#17122=ORIENTED_EDGE('',*,*,#12744,.T.);
#17123=ORIENTED_EDGE('',*,*,#12748,.T.);
#17124=ORIENTED_EDGE('',*,*,#12749,.F.);
#17125=ORIENTED_EDGE('',*,*,#12750,.F.);
#17126=ORIENTED_EDGE('',*,*,#12745,.T.);
#17127=ORIENTED_EDGE('',*,*,#12750,.T.);
#17128=ORIENTED_EDGE('',*,*,#12751,.F.);
#17129=ORIENTED_EDGE('',*,*,#12752,.F.);
#17130=ORIENTED_EDGE('',*,*,#12746,.T.);
#17131=ORIENTED_EDGE('',*,*,#12752,.T.);
#17132=ORIENTED_EDGE('',*,*,#12753,.F.);
#17133=ORIENTED_EDGE('',*,*,#12754,.F.);
#17134=ORIENTED_EDGE('',*,*,#12743,.T.);
#17135=ORIENTED_EDGE('',*,*,#12754,.T.);
#17136=ORIENTED_EDGE('',*,*,#12755,.F.);
#17137=ORIENTED_EDGE('',*,*,#12748,.F.);
#17138=ORIENTED_EDGE('',*,*,#12755,.T.);
#17139=ORIENTED_EDGE('',*,*,#12753,.T.);
#17140=ORIENTED_EDGE('',*,*,#12751,.T.);
#17141=ORIENTED_EDGE('',*,*,#12749,.T.);
#17142=ORIENTED_EDGE('',*,*,#12480,.T.);
#17143=ORIENTED_EDGE('',*,*,#12483,.T.);
#17144=ORIENTED_EDGE('',*,*,#12486,.T.);
#17145=ORIENTED_EDGE('',*,*,#12489,.T.);
#17146=ORIENTED_EDGE('',*,*,#12725,.T.);
#17147=ORIENTED_EDGE('',*,*,#12729,.T.);
#17148=ORIENTED_EDGE('',*,*,#12732,.T.);
#17149=ORIENTED_EDGE('',*,*,#12735,.T.);
#17150=ORIENTED_EDGE('',*,*,#12738,.T.);
#17151=ORIENTED_EDGE('',*,*,#12741,.T.);
#17152=ORIENTED_EDGE('',*,*,#12756,.F.);
#17153=ORIENTED_EDGE('',*,*,#12404,.F.);
#17154=ORIENTED_EDGE('',*,*,#12757,.T.);
#17155=ORIENTED_EDGE('',*,*,#12756,.T.);
#17156=ORIENTED_EDGE('',*,*,#12757,.F.);
#17157=ORIENTED_EDGE('',*,*,#12432,.T.);
#17158=ORIENTED_EDGE('',*,*,#12470,.T.);
#17159=ORIENTED_EDGE('',*,*,#12747,.F.);
#17160=ORIENTED_EDGE('',*,*,#12477,.T.);
#17161=ORIENTED_EDGE('',*,*,#12758,.T.);
#17162=ORIENTED_EDGE('',*,*,#12759,.T.);
#17163=ORIENTED_EDGE('',*,*,#12760,.T.);
#17164=ORIENTED_EDGE('',*,*,#12761,.T.);
#17165=ORIENTED_EDGE('',*,*,#12759,.F.);
#17166=ORIENTED_EDGE('',*,*,#12760,.F.);
#17167=ORIENTED_EDGE('',*,*,#12761,.F.);
#17168=ORIENTED_EDGE('',*,*,#12762,.T.);
#17169=ORIENTED_EDGE('',*,*,#12763,.F.);
#17170=ORIENTED_EDGE('',*,*,#12764,.F.);
#17171=ORIENTED_EDGE('',*,*,#12762,.F.);
#17172=ORIENTED_EDGE('',*,*,#12758,.F.);
#17173=ORIENTED_EDGE('',*,*,#12763,.T.);
#17174=ORIENTED_EDGE('',*,*,#12764,.T.);
#17175=ORIENTED_EDGE('',*,*,#12765,.T.);
#17176=ORIENTED_EDGE('',*,*,#12766,.T.);
#17177=ORIENTED_EDGE('',*,*,#12765,.F.);
#17178=ORIENTED_EDGE('',*,*,#12766,.F.);
#17179=ORIENTED_EDGE('',*,*,#12767,.T.);
#17180=ORIENTED_EDGE('',*,*,#12768,.T.);
#17181=ORIENTED_EDGE('',*,*,#12769,.F.);
#17182=ORIENTED_EDGE('',*,*,#12768,.F.);
#17183=ORIENTED_EDGE('',*,*,#12770,.F.);
#17184=ORIENTED_EDGE('',*,*,#12767,.F.);
#17185=ORIENTED_EDGE('',*,*,#12771,.F.);
#17186=ORIENTED_EDGE('',*,*,#12769,.T.);
#17187=ORIENTED_EDGE('',*,*,#12772,.F.);
#17188=ORIENTED_EDGE('',*,*,#12773,.F.);
#17189=ORIENTED_EDGE('',*,*,#12774,.T.);
#17190=ORIENTED_EDGE('',*,*,#12771,.T.);
#17191=ORIENTED_EDGE('',*,*,#12774,.F.);
#17192=ORIENTED_EDGE('',*,*,#12775,.T.);
#17193=ORIENTED_EDGE('',*,*,#12776,.T.);
#17194=ORIENTED_EDGE('',*,*,#12777,.F.);
#17195=ORIENTED_EDGE('',*,*,#12776,.F.);
#17196=ORIENTED_EDGE('',*,*,#12778,.F.);
#17197=ORIENTED_EDGE('',*,*,#12775,.F.);
#17198=ORIENTED_EDGE('',*,*,#12779,.F.);
#17199=ORIENTED_EDGE('',*,*,#12777,.T.);
#17200=ORIENTED_EDGE('',*,*,#12770,.T.);
#17201=ORIENTED_EDGE('',*,*,#12780,.T.);
#17202=ORIENTED_EDGE('',*,*,#12779,.T.);
#17203=ORIENTED_EDGE('',*,*,#12780,.F.);
#17204=ORIENTED_EDGE('',*,*,#12781,.T.);
#17205=ORIENTED_EDGE('',*,*,#12782,.T.);
#17206=ORIENTED_EDGE('',*,*,#12772,.T.);
#17207=ORIENTED_EDGE('',*,*,#12773,.T.);
#17208=ORIENTED_EDGE('',*,*,#12782,.F.);
#17209=ORIENTED_EDGE('',*,*,#12778,.T.);
#17210=ORIENTED_EDGE('',*,*,#12783,.T.);
#17211=ORIENTED_EDGE('',*,*,#12784,.F.);
#17212=ORIENTED_EDGE('',*,*,#12785,.F.);
#17213=ORIENTED_EDGE('',*,*,#12783,.F.);
#17214=ORIENTED_EDGE('',*,*,#12781,.F.);
#17215=ORIENTED_EDGE('',*,*,#12786,.F.);
#17216=ORIENTED_EDGE('',*,*,#12784,.T.);
#17217=ORIENTED_EDGE('',*,*,#12785,.T.);
#17218=ORIENTED_EDGE('',*,*,#12787,.T.);
#17219=ORIENTED_EDGE('',*,*,#12788,.T.);
#17220=ORIENTED_EDGE('',*,*,#12787,.F.);
#17221=ORIENTED_EDGE('',*,*,#12788,.F.);
#17222=ORIENTED_EDGE('',*,*,#12789,.T.);
#17223=ORIENTED_EDGE('',*,*,#12786,.T.);
#17224=ORIENTED_EDGE('',*,*,#12790,.T.);
#17225=ORIENTED_EDGE('',*,*,#12789,.F.);
#17226=ORIENTED_EDGE('',*,*,#12790,.F.);
#17227=ORIENTED_EDGE('',*,*,#12791,.T.);
#17228=ORIENTED_EDGE('',*,*,#12792,.T.);
#17229=ORIENTED_EDGE('',*,*,#12793,.T.);
#17230=ORIENTED_EDGE('',*,*,#12794,.T.);
#17231=ORIENTED_EDGE('',*,*,#12795,.T.);
#17232=ORIENTED_EDGE('',*,*,#12793,.F.);
#17233=ORIENTED_EDGE('',*,*,#12794,.F.);
#17234=ORIENTED_EDGE('',*,*,#12795,.F.);
#17235=ORIENTED_EDGE('',*,*,#12796,.T.);
#17236=ORIENTED_EDGE('',*,*,#12797,.F.);
#17237=ORIENTED_EDGE('',*,*,#12798,.F.);
#17238=ORIENTED_EDGE('',*,*,#12796,.F.);
#17239=ORIENTED_EDGE('',*,*,#12799,.F.);
#17240=ORIENTED_EDGE('',*,*,#12800,.T.);
#17241=ORIENTED_EDGE('',*,*,#12791,.F.);
#17242=ORIENTED_EDGE('',*,*,#12792,.F.);
#17243=ORIENTED_EDGE('',*,*,#12800,.F.);
#17244=ORIENTED_EDGE('',*,*,#12797,.T.);
#17245=ORIENTED_EDGE('',*,*,#12798,.T.);
#17246=ORIENTED_EDGE('',*,*,#12801,.T.);
#17247=ORIENTED_EDGE('',*,*,#12802,.T.);
#17248=ORIENTED_EDGE('',*,*,#12801,.F.);
#17249=ORIENTED_EDGE('',*,*,#12802,.F.);
#17250=ORIENTED_EDGE('',*,*,#12803,.T.);
#17251=ORIENTED_EDGE('',*,*,#12804,.F.);
#17252=ORIENTED_EDGE('',*,*,#12805,.F.);
#17253=ORIENTED_EDGE('',*,*,#12806,.T.);
#17254=ORIENTED_EDGE('',*,*,#12807,.T.);
#17255=ORIENTED_EDGE('',*,*,#12808,.F.);
#17256=ORIENTED_EDGE('',*,*,#12807,.F.);
#17257=ORIENTED_EDGE('',*,*,#12809,.F.);
#17258=ORIENTED_EDGE('',*,*,#12810,.F.);
#17259=ORIENTED_EDGE('',*,*,#12809,.T.);
#17260=ORIENTED_EDGE('',*,*,#12806,.F.);
#17261=ORIENTED_EDGE('',*,*,#12811,.F.);
#17262=ORIENTED_EDGE('',*,*,#12812,.F.);
#17263=ORIENTED_EDGE('',*,*,#12811,.T.);
#17264=ORIENTED_EDGE('',*,*,#12805,.T.);
#17265=ORIENTED_EDGE('',*,*,#12813,.F.);
#17266=ORIENTED_EDGE('',*,*,#12814,.F.);
#17267=ORIENTED_EDGE('',*,*,#12815,.T.);
#17268=ORIENTED_EDGE('',*,*,#12816,.T.);
#17269=ORIENTED_EDGE('',*,*,#12817,.F.);
#17270=ORIENTED_EDGE('',*,*,#12816,.F.);
#17271=ORIENTED_EDGE('',*,*,#12818,.F.);
#17272=ORIENTED_EDGE('',*,*,#12819,.F.);
#17273=ORIENTED_EDGE('',*,*,#12818,.T.);
#17274=ORIENTED_EDGE('',*,*,#12815,.F.);
#17275=ORIENTED_EDGE('',*,*,#12820,.F.);
#17276=ORIENTED_EDGE('',*,*,#12821,.F.);
#17277=ORIENTED_EDGE('',*,*,#12820,.T.);
#17278=ORIENTED_EDGE('',*,*,#12814,.T.);
#17279=ORIENTED_EDGE('',*,*,#12822,.F.);
#17280=ORIENTED_EDGE('',*,*,#12823,.F.);
#17281=ORIENTED_EDGE('',*,*,#12824,.T.);
#17282=ORIENTED_EDGE('',*,*,#12825,.T.);
#17283=ORIENTED_EDGE('',*,*,#12826,.F.);
#17284=ORIENTED_EDGE('',*,*,#12825,.F.);
#17285=ORIENTED_EDGE('',*,*,#12827,.F.);
#17286=ORIENTED_EDGE('',*,*,#12828,.F.);
#17287=ORIENTED_EDGE('',*,*,#12827,.T.);
#17288=ORIENTED_EDGE('',*,*,#12824,.F.);
#17289=ORIENTED_EDGE('',*,*,#12829,.F.);
#17290=ORIENTED_EDGE('',*,*,#12830,.F.);
#17291=ORIENTED_EDGE('',*,*,#12829,.T.);
#17292=ORIENTED_EDGE('',*,*,#12823,.T.);
#17293=ORIENTED_EDGE('',*,*,#12831,.F.);
#17294=ORIENTED_EDGE('',*,*,#12832,.F.);
#17295=ORIENTED_EDGE('',*,*,#12833,.T.);
#17296=ORIENTED_EDGE('',*,*,#12834,.T.);
#17297=ORIENTED_EDGE('',*,*,#12835,.F.);
#17298=ORIENTED_EDGE('',*,*,#12834,.F.);
#17299=ORIENTED_EDGE('',*,*,#12836,.F.);
#17300=ORIENTED_EDGE('',*,*,#12837,.F.);
#17301=ORIENTED_EDGE('',*,*,#12836,.T.);
#17302=ORIENTED_EDGE('',*,*,#12833,.F.);
#17303=ORIENTED_EDGE('',*,*,#12838,.F.);
#17304=ORIENTED_EDGE('',*,*,#12839,.F.);
#17305=ORIENTED_EDGE('',*,*,#12838,.T.);
#17306=ORIENTED_EDGE('',*,*,#12832,.T.);
#17307=ORIENTED_EDGE('',*,*,#12840,.F.);
#17308=ORIENTED_EDGE('',*,*,#12841,.F.);
#17309=ORIENTED_EDGE('',*,*,#12842,.T.);
#17310=ORIENTED_EDGE('',*,*,#12843,.T.);
#17311=ORIENTED_EDGE('',*,*,#12844,.F.);
#17312=ORIENTED_EDGE('',*,*,#12843,.F.);
#17313=ORIENTED_EDGE('',*,*,#12845,.F.);
#17314=ORIENTED_EDGE('',*,*,#12846,.F.);
#17315=ORIENTED_EDGE('',*,*,#12845,.T.);
#17316=ORIENTED_EDGE('',*,*,#12842,.F.);
#17317=ORIENTED_EDGE('',*,*,#12847,.F.);
#17318=ORIENTED_EDGE('',*,*,#12848,.F.);
#17319=ORIENTED_EDGE('',*,*,#12847,.T.);
#17320=ORIENTED_EDGE('',*,*,#12841,.T.);
#17321=ORIENTED_EDGE('',*,*,#12849,.F.);
#17322=ORIENTED_EDGE('',*,*,#12850,.F.);
#17323=ORIENTED_EDGE('',*,*,#12851,.T.);
#17324=ORIENTED_EDGE('',*,*,#12852,.T.);
#17325=ORIENTED_EDGE('',*,*,#12853,.F.);
#17326=ORIENTED_EDGE('',*,*,#12852,.F.);
#17327=ORIENTED_EDGE('',*,*,#12854,.F.);
#17328=ORIENTED_EDGE('',*,*,#12855,.F.);
#17329=ORIENTED_EDGE('',*,*,#12854,.T.);
#17330=ORIENTED_EDGE('',*,*,#12851,.F.);
#17331=ORIENTED_EDGE('',*,*,#12856,.F.);
#17332=ORIENTED_EDGE('',*,*,#12857,.F.);
#17333=ORIENTED_EDGE('',*,*,#12856,.T.);
#17334=ORIENTED_EDGE('',*,*,#12850,.T.);
#17335=ORIENTED_EDGE('',*,*,#12858,.F.);
#17336=ORIENTED_EDGE('',*,*,#12859,.F.);
#17337=ORIENTED_EDGE('',*,*,#12860,.T.);
#17338=ORIENTED_EDGE('',*,*,#12861,.T.);
#17339=ORIENTED_EDGE('',*,*,#12862,.F.);
#17340=ORIENTED_EDGE('',*,*,#12861,.F.);
#17341=ORIENTED_EDGE('',*,*,#12863,.F.);
#17342=ORIENTED_EDGE('',*,*,#12864,.F.);
#17343=ORIENTED_EDGE('',*,*,#12863,.T.);
#17344=ORIENTED_EDGE('',*,*,#12860,.F.);
#17345=ORIENTED_EDGE('',*,*,#12865,.F.);
#17346=ORIENTED_EDGE('',*,*,#12866,.F.);
#17347=ORIENTED_EDGE('',*,*,#12865,.T.);
#17348=ORIENTED_EDGE('',*,*,#12859,.T.);
#17349=ORIENTED_EDGE('',*,*,#12867,.F.);
#17350=ORIENTED_EDGE('',*,*,#12868,.F.);
#17351=ORIENTED_EDGE('',*,*,#12869,.T.);
#17352=ORIENTED_EDGE('',*,*,#12870,.T.);
#17353=ORIENTED_EDGE('',*,*,#12871,.F.);
#17354=ORIENTED_EDGE('',*,*,#12870,.F.);
#17355=ORIENTED_EDGE('',*,*,#12872,.F.);
#17356=ORIENTED_EDGE('',*,*,#12873,.F.);
#17357=ORIENTED_EDGE('',*,*,#12872,.T.);
#17358=ORIENTED_EDGE('',*,*,#12869,.F.);
#17359=ORIENTED_EDGE('',*,*,#12874,.F.);
#17360=ORIENTED_EDGE('',*,*,#12875,.F.);
#17361=ORIENTED_EDGE('',*,*,#12874,.T.);
#17362=ORIENTED_EDGE('',*,*,#12868,.T.);
#17363=ORIENTED_EDGE('',*,*,#12876,.F.);
#17364=ORIENTED_EDGE('',*,*,#12877,.F.);
#17365=ORIENTED_EDGE('',*,*,#12878,.T.);
#17366=ORIENTED_EDGE('',*,*,#12879,.T.);
#17367=ORIENTED_EDGE('',*,*,#12880,.F.);
#17368=ORIENTED_EDGE('',*,*,#12879,.F.);
#17369=ORIENTED_EDGE('',*,*,#12881,.F.);
#17370=ORIENTED_EDGE('',*,*,#12882,.F.);
#17371=ORIENTED_EDGE('',*,*,#12883,.F.);
#17372=ORIENTED_EDGE('',*,*,#12881,.T.);
#17373=ORIENTED_EDGE('',*,*,#12878,.F.);
#17374=ORIENTED_EDGE('',*,*,#12884,.F.);
#17375=ORIENTED_EDGE('',*,*,#12885,.F.);
#17376=ORIENTED_EDGE('',*,*,#12884,.T.);
#17377=ORIENTED_EDGE('',*,*,#12877,.T.);
#17378=ORIENTED_EDGE('',*,*,#12886,.F.);
#17379=ORIENTED_EDGE('',*,*,#12887,.F.);
#17380=ORIENTED_EDGE('',*,*,#12888,.F.);
#17381=ORIENTED_EDGE('',*,*,#12889,.T.);
#17382=ORIENTED_EDGE('',*,*,#12890,.T.);
#17383=ORIENTED_EDGE('',*,*,#12891,.F.);
#17384=ORIENTED_EDGE('',*,*,#12890,.F.);
#17385=ORIENTED_EDGE('',*,*,#12892,.F.);
#17386=ORIENTED_EDGE('',*,*,#12893,.F.);
#17387=ORIENTED_EDGE('',*,*,#12892,.T.);
#17388=ORIENTED_EDGE('',*,*,#12889,.F.);
#17389=ORIENTED_EDGE('',*,*,#12894,.F.);
#17390=ORIENTED_EDGE('',*,*,#12895,.F.);
#17391=ORIENTED_EDGE('',*,*,#12894,.T.);
#17392=ORIENTED_EDGE('',*,*,#12888,.T.);
#17393=ORIENTED_EDGE('',*,*,#12896,.F.);
#17394=ORIENTED_EDGE('',*,*,#12897,.F.);
#17395=ORIENTED_EDGE('',*,*,#12898,.T.);
#17396=ORIENTED_EDGE('',*,*,#12899,.T.);
#17397=ORIENTED_EDGE('',*,*,#12900,.F.);
#17398=ORIENTED_EDGE('',*,*,#12899,.F.);
#17399=ORIENTED_EDGE('',*,*,#12901,.F.);
#17400=ORIENTED_EDGE('',*,*,#12902,.F.);
#17401=ORIENTED_EDGE('',*,*,#12901,.T.);
#17402=ORIENTED_EDGE('',*,*,#12898,.F.);
#17403=ORIENTED_EDGE('',*,*,#12903,.F.);
#17404=ORIENTED_EDGE('',*,*,#12904,.F.);
#17405=ORIENTED_EDGE('',*,*,#12903,.T.);
#17406=ORIENTED_EDGE('',*,*,#12897,.T.);
#17407=ORIENTED_EDGE('',*,*,#12905,.F.);
#17408=ORIENTED_EDGE('',*,*,#12906,.F.);
#17409=ORIENTED_EDGE('',*,*,#12907,.T.);
#17410=ORIENTED_EDGE('',*,*,#12908,.T.);
#17411=ORIENTED_EDGE('',*,*,#12909,.F.);
#17412=ORIENTED_EDGE('',*,*,#12908,.F.);
#17413=ORIENTED_EDGE('',*,*,#12910,.F.);
#17414=ORIENTED_EDGE('',*,*,#12911,.F.);
#17415=ORIENTED_EDGE('',*,*,#12910,.T.);
#17416=ORIENTED_EDGE('',*,*,#12907,.F.);
#17417=ORIENTED_EDGE('',*,*,#12912,.F.);
#17418=ORIENTED_EDGE('',*,*,#12913,.F.);
#17419=ORIENTED_EDGE('',*,*,#12912,.T.);
#17420=ORIENTED_EDGE('',*,*,#12906,.T.);
#17421=ORIENTED_EDGE('',*,*,#12914,.F.);
#17422=ORIENTED_EDGE('',*,*,#12915,.F.);
#17423=ORIENTED_EDGE('',*,*,#12916,.T.);
#17424=ORIENTED_EDGE('',*,*,#12917,.T.);
#17425=ORIENTED_EDGE('',*,*,#12918,.F.);
#17426=ORIENTED_EDGE('',*,*,#12917,.F.);
#17427=ORIENTED_EDGE('',*,*,#12919,.F.);
#17428=ORIENTED_EDGE('',*,*,#12920,.F.);
#17429=ORIENTED_EDGE('',*,*,#12919,.T.);
#17430=ORIENTED_EDGE('',*,*,#12916,.F.);
#17431=ORIENTED_EDGE('',*,*,#12921,.F.);
#17432=ORIENTED_EDGE('',*,*,#12922,.F.);
#17433=ORIENTED_EDGE('',*,*,#12921,.T.);
#17434=ORIENTED_EDGE('',*,*,#12915,.T.);
#17435=ORIENTED_EDGE('',*,*,#12923,.F.);
#17436=ORIENTED_EDGE('',*,*,#12924,.F.);
#17437=ORIENTED_EDGE('',*,*,#12925,.T.);
#17438=ORIENTED_EDGE('',*,*,#12926,.T.);
#17439=ORIENTED_EDGE('',*,*,#12927,.F.);
#17440=ORIENTED_EDGE('',*,*,#12926,.F.);
#17441=ORIENTED_EDGE('',*,*,#12928,.F.);
#17442=ORIENTED_EDGE('',*,*,#12929,.F.);
#17443=ORIENTED_EDGE('',*,*,#12928,.T.);
#17444=ORIENTED_EDGE('',*,*,#12925,.F.);
#17445=ORIENTED_EDGE('',*,*,#12930,.F.);
#17446=ORIENTED_EDGE('',*,*,#12931,.F.);
#17447=ORIENTED_EDGE('',*,*,#12930,.T.);
#17448=ORIENTED_EDGE('',*,*,#12924,.T.);
#17449=ORIENTED_EDGE('',*,*,#12932,.F.);
#17450=ORIENTED_EDGE('',*,*,#12933,.F.);
#17451=ORIENTED_EDGE('',*,*,#12934,.T.);
#17452=ORIENTED_EDGE('',*,*,#12935,.T.);
#17453=ORIENTED_EDGE('',*,*,#12936,.F.);
#17454=ORIENTED_EDGE('',*,*,#12935,.F.);
#17455=ORIENTED_EDGE('',*,*,#12937,.F.);
#17456=ORIENTED_EDGE('',*,*,#12938,.F.);
#17457=ORIENTED_EDGE('',*,*,#12937,.T.);
#17458=ORIENTED_EDGE('',*,*,#12934,.F.);
#17459=ORIENTED_EDGE('',*,*,#12939,.F.);
#17460=ORIENTED_EDGE('',*,*,#12940,.F.);
#17461=ORIENTED_EDGE('',*,*,#12939,.T.);
#17462=ORIENTED_EDGE('',*,*,#12933,.T.);
#17463=ORIENTED_EDGE('',*,*,#12941,.F.);
#17464=ORIENTED_EDGE('',*,*,#12942,.F.);
#17465=ORIENTED_EDGE('',*,*,#12943,.T.);
#17466=ORIENTED_EDGE('',*,*,#12944,.T.);
#17467=ORIENTED_EDGE('',*,*,#12945,.F.);
#17468=ORIENTED_EDGE('',*,*,#12944,.F.);
#17469=ORIENTED_EDGE('',*,*,#12946,.F.);
#17470=ORIENTED_EDGE('',*,*,#12947,.F.);
#17471=ORIENTED_EDGE('',*,*,#12946,.T.);
#17472=ORIENTED_EDGE('',*,*,#12943,.F.);
#17473=ORIENTED_EDGE('',*,*,#12948,.F.);
#17474=ORIENTED_EDGE('',*,*,#12949,.F.);
#17475=ORIENTED_EDGE('',*,*,#12948,.T.);
#17476=ORIENTED_EDGE('',*,*,#12942,.T.);
#17477=ORIENTED_EDGE('',*,*,#12950,.F.);
#17478=ORIENTED_EDGE('',*,*,#12951,.F.);
#17479=ORIENTED_EDGE('',*,*,#12952,.T.);
#17480=ORIENTED_EDGE('',*,*,#12953,.T.);
#17481=ORIENTED_EDGE('',*,*,#12954,.F.);
#17482=ORIENTED_EDGE('',*,*,#12953,.F.);
#17483=ORIENTED_EDGE('',*,*,#12955,.F.);
#17484=ORIENTED_EDGE('',*,*,#12956,.F.);
#17485=ORIENTED_EDGE('',*,*,#12955,.T.);
#17486=ORIENTED_EDGE('',*,*,#12952,.F.);
#17487=ORIENTED_EDGE('',*,*,#12957,.F.);
#17488=ORIENTED_EDGE('',*,*,#12958,.F.);
#17489=ORIENTED_EDGE('',*,*,#12957,.T.);
#17490=ORIENTED_EDGE('',*,*,#12951,.T.);
#17491=ORIENTED_EDGE('',*,*,#12959,.F.);
#17492=ORIENTED_EDGE('',*,*,#12960,.F.);
#17493=ORIENTED_EDGE('',*,*,#12961,.T.);
#17494=ORIENTED_EDGE('',*,*,#12962,.T.);
#17495=ORIENTED_EDGE('',*,*,#12963,.F.);
#17496=ORIENTED_EDGE('',*,*,#12962,.F.);
#17497=ORIENTED_EDGE('',*,*,#12964,.F.);
#17498=ORIENTED_EDGE('',*,*,#12965,.F.);
#17499=ORIENTED_EDGE('',*,*,#12964,.T.);
#17500=ORIENTED_EDGE('',*,*,#12961,.F.);
#17501=ORIENTED_EDGE('',*,*,#12966,.F.);
#17502=ORIENTED_EDGE('',*,*,#12967,.F.);
#17503=ORIENTED_EDGE('',*,*,#12966,.T.);
#17504=ORIENTED_EDGE('',*,*,#12960,.T.);
#17505=ORIENTED_EDGE('',*,*,#12968,.F.);
#17506=ORIENTED_EDGE('',*,*,#12969,.T.);
#17507=ORIENTED_EDGE('',*,*,#12970,.F.);
#17508=ORIENTED_EDGE('',*,*,#12969,.F.);
#17509=ORIENTED_EDGE('',*,*,#12971,.F.);
#17510=ORIENTED_EDGE('',*,*,#12972,.T.);
#17511=ORIENTED_EDGE('',*,*,#12973,.T.);
#17512=ORIENTED_EDGE('',*,*,#12972,.F.);
#17513=ORIENTED_EDGE('',*,*,#12973,.F.);
#17514=ORIENTED_EDGE('',*,*,#12970,.T.);
#17515=ORIENTED_EDGE('',*,*,#12974,.F.);
#17516=ORIENTED_EDGE('',*,*,#12971,.T.);
#17517=ORIENTED_EDGE('',*,*,#12968,.T.);
#17518=ORIENTED_EDGE('',*,*,#12975,.F.);
#17519=ORIENTED_EDGE('',*,*,#12976,.T.);
#17520=ORIENTED_EDGE('',*,*,#12974,.T.);
#17521=ORIENTED_EDGE('',*,*,#12976,.F.);
#17522=ORIENTED_EDGE('',*,*,#12803,.F.);
#17523=ORIENTED_EDGE('',*,*,#12977,.T.);
#17524=ORIENTED_EDGE('',*,*,#12975,.T.);
#17525=ORIENTED_EDGE('',*,*,#12977,.F.);
#17526=ORIENTED_EDGE('',*,*,#12799,.T.);
#17527=ORIENTED_EDGE('',*,*,#12978,.F.);
#17528=ORIENTED_EDGE('',*,*,#12979,.F.);
#17529=ORIENTED_EDGE('',*,*,#12980,.T.);
#17530=ORIENTED_EDGE('',*,*,#12882,.T.);
#17531=ORIENTED_EDGE('',*,*,#12883,.T.);
#17532=ORIENTED_EDGE('',*,*,#12885,.T.);
#17533=ORIENTED_EDGE('',*,*,#12981,.T.);
#17534=ORIENTED_EDGE('',*,*,#12978,.T.);
#17535=ORIENTED_EDGE('',*,*,#12981,.F.);
#17536=ORIENTED_EDGE('',*,*,#12886,.T.);
#17537=ORIENTED_EDGE('',*,*,#12876,.T.);
#17538=ORIENTED_EDGE('',*,*,#12880,.T.);
#17539=ORIENTED_EDGE('',*,*,#12980,.F.);
#17540=ORIENTED_EDGE('',*,*,#12810,.T.);
#17541=ORIENTED_EDGE('',*,*,#12812,.T.);
#17542=ORIENTED_EDGE('',*,*,#12804,.T.);
#17543=ORIENTED_EDGE('',*,*,#12808,.T.);
#17544=ORIENTED_EDGE('',*,*,#12819,.T.);
#17545=ORIENTED_EDGE('',*,*,#12821,.T.);
#17546=ORIENTED_EDGE('',*,*,#12813,.T.);
#17547=ORIENTED_EDGE('',*,*,#12817,.T.);
#17548=ORIENTED_EDGE('',*,*,#12828,.T.);
#17549=ORIENTED_EDGE('',*,*,#12830,.T.);
#17550=ORIENTED_EDGE('',*,*,#12822,.T.);
#17551=ORIENTED_EDGE('',*,*,#12826,.T.);
#17552=ORIENTED_EDGE('',*,*,#12837,.T.);
#17553=ORIENTED_EDGE('',*,*,#12839,.T.);
#17554=ORIENTED_EDGE('',*,*,#12831,.T.);
#17555=ORIENTED_EDGE('',*,*,#12835,.T.);
#17556=ORIENTED_EDGE('',*,*,#12846,.T.);
#17557=ORIENTED_EDGE('',*,*,#12848,.T.);
#17558=ORIENTED_EDGE('',*,*,#12840,.T.);
#17559=ORIENTED_EDGE('',*,*,#12844,.T.);
#17560=ORIENTED_EDGE('',*,*,#12855,.T.);
#17561=ORIENTED_EDGE('',*,*,#12857,.T.);
#17562=ORIENTED_EDGE('',*,*,#12849,.T.);
#17563=ORIENTED_EDGE('',*,*,#12853,.T.);
#17564=ORIENTED_EDGE('',*,*,#12864,.T.);
#17565=ORIENTED_EDGE('',*,*,#12866,.T.);
#17566=ORIENTED_EDGE('',*,*,#12858,.T.);
#17567=ORIENTED_EDGE('',*,*,#12862,.T.);
#17568=ORIENTED_EDGE('',*,*,#12873,.T.);
#17569=ORIENTED_EDGE('',*,*,#12875,.T.);
#17570=ORIENTED_EDGE('',*,*,#12867,.T.);
#17571=ORIENTED_EDGE('',*,*,#12871,.T.);
#17572=ORIENTED_EDGE('',*,*,#12893,.T.);
#17573=ORIENTED_EDGE('',*,*,#12895,.T.);
#17574=ORIENTED_EDGE('',*,*,#12887,.T.);
#17575=ORIENTED_EDGE('',*,*,#12891,.T.);
#17576=ORIENTED_EDGE('',*,*,#12902,.T.);
#17577=ORIENTED_EDGE('',*,*,#12904,.T.);
#17578=ORIENTED_EDGE('',*,*,#12896,.T.);
#17579=ORIENTED_EDGE('',*,*,#12900,.T.);
#17580=ORIENTED_EDGE('',*,*,#12911,.T.);
#17581=ORIENTED_EDGE('',*,*,#12913,.T.);
#17582=ORIENTED_EDGE('',*,*,#12905,.T.);
#17583=ORIENTED_EDGE('',*,*,#12909,.T.);
#17584=ORIENTED_EDGE('',*,*,#12920,.T.);
#17585=ORIENTED_EDGE('',*,*,#12922,.T.);
#17586=ORIENTED_EDGE('',*,*,#12914,.T.);
#17587=ORIENTED_EDGE('',*,*,#12918,.T.);
#17588=ORIENTED_EDGE('',*,*,#12929,.T.);
#17589=ORIENTED_EDGE('',*,*,#12931,.T.);
#17590=ORIENTED_EDGE('',*,*,#12923,.T.);
#17591=ORIENTED_EDGE('',*,*,#12927,.T.);
#17592=ORIENTED_EDGE('',*,*,#12938,.T.);
#17593=ORIENTED_EDGE('',*,*,#12940,.T.);
#17594=ORIENTED_EDGE('',*,*,#12932,.T.);
#17595=ORIENTED_EDGE('',*,*,#12936,.T.);
#17596=ORIENTED_EDGE('',*,*,#12947,.T.);
#17597=ORIENTED_EDGE('',*,*,#12949,.T.);
#17598=ORIENTED_EDGE('',*,*,#12941,.T.);
#17599=ORIENTED_EDGE('',*,*,#12945,.T.);
#17600=ORIENTED_EDGE('',*,*,#12956,.T.);
#17601=ORIENTED_EDGE('',*,*,#12958,.T.);
#17602=ORIENTED_EDGE('',*,*,#12950,.T.);
#17603=ORIENTED_EDGE('',*,*,#12954,.T.);
#17604=ORIENTED_EDGE('',*,*,#12965,.T.);
#17605=ORIENTED_EDGE('',*,*,#12967,.T.);
#17606=ORIENTED_EDGE('',*,*,#12959,.T.);
#17607=ORIENTED_EDGE('',*,*,#12963,.T.);
#17608=ORIENTED_EDGE('',*,*,#12979,.T.);
#17609=ORIENTED_EDGE('',*,*,#12982,.F.);
#17610=ORIENTED_EDGE('',*,*,#12983,.F.);
#17611=ORIENTED_EDGE('',*,*,#12984,.T.);
#17612=ORIENTED_EDGE('',*,*,#12982,.T.);
#17613=ORIENTED_EDGE('',*,*,#12984,.F.);
#17614=ORIENTED_EDGE('',*,*,#12983,.T.);
#17615=ORIENTED_EDGE('',*,*,#12985,.T.);
#17616=ORIENTED_EDGE('',*,*,#12986,.T.);
#17617=ORIENTED_EDGE('',*,*,#12987,.F.);
#17618=ORIENTED_EDGE('',*,*,#12986,.F.);
#17619=ORIENTED_EDGE('',*,*,#12988,.F.);
#17620=ORIENTED_EDGE('',*,*,#12987,.T.);
#17621=ORIENTED_EDGE('',*,*,#12989,.F.);
#17622=ORIENTED_EDGE('',*,*,#12990,.T.);
#17623=ORIENTED_EDGE('',*,*,#12988,.T.);
#17624=ORIENTED_EDGE('',*,*,#12990,.F.);
#17625=ORIENTED_EDGE('',*,*,#12989,.T.);
#17626=ORIENTED_EDGE('',*,*,#12985,.F.);
#17627=ORIENTED_EDGE('',*,*,#12991,.T.);
#17628=ORIENTED_EDGE('',*,*,#12992,.T.);
#17629=ORIENTED_EDGE('',*,*,#12993,.T.);
#17630=ORIENTED_EDGE('',*,*,#12992,.F.);
#17631=ORIENTED_EDGE('',*,*,#12993,.F.);
#17632=ORIENTED_EDGE('',*,*,#12994,.T.);
#17633=ORIENTED_EDGE('',*,*,#12995,.F.);
#17634=ORIENTED_EDGE('',*,*,#12996,.F.);
#17635=ORIENTED_EDGE('',*,*,#12994,.F.);
#17636=ORIENTED_EDGE('',*,*,#12997,.F.);
#17637=ORIENTED_EDGE('',*,*,#12998,.F.);
#17638=ORIENTED_EDGE('',*,*,#12999,.F.);
#17639=ORIENTED_EDGE('',*,*,#13000,.F.);
#17640=ORIENTED_EDGE('',*,*,#13001,.F.);
#17641=ORIENTED_EDGE('',*,*,#13002,.T.);
#17642=ORIENTED_EDGE('',*,*,#12991,.F.);
#17643=ORIENTED_EDGE('',*,*,#13003,.T.);
#17644=ORIENTED_EDGE('',*,*,#13004,.T.);
#17645=ORIENTED_EDGE('',*,*,#12995,.T.);
#17646=ORIENTED_EDGE('',*,*,#12996,.T.);
#17647=ORIENTED_EDGE('',*,*,#13004,.F.);
#17648=ORIENTED_EDGE('',*,*,#13005,.F.);
#17649=ORIENTED_EDGE('',*,*,#13006,.F.);
#17650=ORIENTED_EDGE('',*,*,#13007,.F.);
#17651=ORIENTED_EDGE('',*,*,#13008,.F.);
#17652=ORIENTED_EDGE('',*,*,#13009,.F.);
#17653=ORIENTED_EDGE('',*,*,#13010,.F.);
#17654=ORIENTED_EDGE('',*,*,#13011,.F.);
#17655=ORIENTED_EDGE('',*,*,#13012,.F.);
#17656=ORIENTED_EDGE('',*,*,#13003,.F.);
#17657=ORIENTED_EDGE('',*,*,#13013,.T.);
#17658=ORIENTED_EDGE('',*,*,#13001,.T.);
#17659=ORIENTED_EDGE('',*,*,#13014,.T.);
#17660=ORIENTED_EDGE('',*,*,#13015,.T.);
#17661=ORIENTED_EDGE('',*,*,#13016,.T.);
#17662=ORIENTED_EDGE('',*,*,#13017,.T.);
#17663=ORIENTED_EDGE('',*,*,#13014,.F.);
#17664=ORIENTED_EDGE('',*,*,#13000,.T.);
#17665=ORIENTED_EDGE('',*,*,#13018,.T.);
#17666=ORIENTED_EDGE('',*,*,#13019,.T.);
#17667=ORIENTED_EDGE('',*,*,#13016,.F.);
#17668=ORIENTED_EDGE('',*,*,#12999,.T.);
#17669=ORIENTED_EDGE('',*,*,#13020,.T.);
#17670=ORIENTED_EDGE('',*,*,#13021,.T.);
#17671=ORIENTED_EDGE('',*,*,#13018,.F.);
#17672=ORIENTED_EDGE('',*,*,#12998,.T.);
#17673=ORIENTED_EDGE('',*,*,#13022,.T.);
#17674=ORIENTED_EDGE('',*,*,#13023,.T.);
#17675=ORIENTED_EDGE('',*,*,#13020,.F.);
#17676=ORIENTED_EDGE('',*,*,#12997,.T.);
#17677=ORIENTED_EDGE('',*,*,#13024,.T.);
#17678=ORIENTED_EDGE('',*,*,#13025,.T.);
#17679=ORIENTED_EDGE('',*,*,#13026,.T.);
#17680=ORIENTED_EDGE('',*,*,#13027,.T.);
#17681=ORIENTED_EDGE('',*,*,#13028,.T.);
#17682=ORIENTED_EDGE('',*,*,#13029,.T.);
#17683=ORIENTED_EDGE('',*,*,#13030,.T.);
#17684=ORIENTED_EDGE('',*,*,#13027,.F.);
#17685=ORIENTED_EDGE('',*,*,#13031,.T.);
#17686=ORIENTED_EDGE('',*,*,#13032,.T.);
#17687=ORIENTED_EDGE('',*,*,#13029,.F.);
#17688=ORIENTED_EDGE('',*,*,#13033,.T.);
#17689=ORIENTED_EDGE('',*,*,#13034,.T.);
#17690=ORIENTED_EDGE('',*,*,#13035,.T.);
#17691=ORIENTED_EDGE('',*,*,#13031,.F.);
#17692=ORIENTED_EDGE('',*,*,#13036,.T.);
#17693=ORIENTED_EDGE('',*,*,#13037,.T.);
#17694=ORIENTED_EDGE('',*,*,#13038,.T.);
#17695=ORIENTED_EDGE('',*,*,#13034,.F.);
#17696=ORIENTED_EDGE('',*,*,#13039,.T.);
#17697=ORIENTED_EDGE('',*,*,#13040,.T.);
#17698=ORIENTED_EDGE('',*,*,#13037,.F.);
#17699=ORIENTED_EDGE('',*,*,#13041,.T.);
#17700=ORIENTED_EDGE('',*,*,#13025,.F.);
#17701=ORIENTED_EDGE('',*,*,#13038,.F.);
#17702=ORIENTED_EDGE('',*,*,#13042,.T.);
#17703=ORIENTED_EDGE('',*,*,#13043,.F.);
#17704=ORIENTED_EDGE('',*,*,#13044,.T.);
#17705=ORIENTED_EDGE('',*,*,#13015,.F.);
#17706=ORIENTED_EDGE('',*,*,#13045,.F.);
#17707=ORIENTED_EDGE('',*,*,#13046,.F.);
#17708=ORIENTED_EDGE('',*,*,#13042,.F.);
#17709=ORIENTED_EDGE('',*,*,#13040,.F.);
#17710=ORIENTED_EDGE('',*,*,#13047,.T.);
#17711=ORIENTED_EDGE('',*,*,#13024,.F.);
#17712=ORIENTED_EDGE('',*,*,#13048,.T.);
#17713=ORIENTED_EDGE('',*,*,#13022,.F.);
#17714=ORIENTED_EDGE('',*,*,#13002,.F.);
#17715=ORIENTED_EDGE('',*,*,#13013,.F.);
#17716=ORIENTED_EDGE('',*,*,#13047,.F.);
#17717=ORIENTED_EDGE('',*,*,#13026,.F.);
#17718=ORIENTED_EDGE('',*,*,#13041,.F.);
#17719=ORIENTED_EDGE('',*,*,#13039,.F.);
#17720=ORIENTED_EDGE('',*,*,#13036,.F.);
#17721=ORIENTED_EDGE('',*,*,#13033,.F.);
#17722=ORIENTED_EDGE('',*,*,#13028,.F.);
#17723=ORIENTED_EDGE('',*,*,#13049,.T.);
#17724=ORIENTED_EDGE('',*,*,#13050,.T.);
#17725=ORIENTED_EDGE('',*,*,#13051,.T.);
#17726=ORIENTED_EDGE('',*,*,#13005,.T.);
#17727=ORIENTED_EDGE('',*,*,#13049,.F.);
#17728=ORIENTED_EDGE('',*,*,#13012,.T.);
#17729=ORIENTED_EDGE('',*,*,#13052,.T.);
#17730=ORIENTED_EDGE('',*,*,#13053,.T.);
#17731=ORIENTED_EDGE('',*,*,#13054,.T.);
#17732=ORIENTED_EDGE('',*,*,#13055,.T.);
#17733=ORIENTED_EDGE('',*,*,#13052,.F.);
#17734=ORIENTED_EDGE('',*,*,#13011,.T.);
#17735=ORIENTED_EDGE('',*,*,#13054,.F.);
#17736=ORIENTED_EDGE('',*,*,#13010,.T.);
#17737=ORIENTED_EDGE('',*,*,#13056,.T.);
#17738=ORIENTED_EDGE('',*,*,#13057,.T.);
#17739=ORIENTED_EDGE('',*,*,#13058,.T.);
#17740=ORIENTED_EDGE('',*,*,#13059,.T.);
#17741=ORIENTED_EDGE('',*,*,#13056,.F.);
#17742=ORIENTED_EDGE('',*,*,#13009,.T.);
#17743=ORIENTED_EDGE('',*,*,#13058,.F.);
#17744=ORIENTED_EDGE('',*,*,#13008,.T.);
#17745=ORIENTED_EDGE('',*,*,#13060,.T.);
#17746=ORIENTED_EDGE('',*,*,#13046,.T.);
#17747=ORIENTED_EDGE('',*,*,#13061,.T.);
#17748=ORIENTED_EDGE('',*,*,#13043,.T.);
#17749=ORIENTED_EDGE('',*,*,#13060,.F.);
#17750=ORIENTED_EDGE('',*,*,#13007,.T.);
#17751=ORIENTED_EDGE('',*,*,#13061,.F.);
#17752=ORIENTED_EDGE('',*,*,#13006,.T.);
#17753=ORIENTED_EDGE('',*,*,#13051,.F.);
#17754=ORIENTED_EDGE('',*,*,#13062,.T.);
#17755=ORIENTED_EDGE('',*,*,#13035,.F.);
#17756=ORIENTED_EDGE('',*,*,#13044,.F.);
#17757=ORIENTED_EDGE('',*,*,#13062,.F.);
#17758=ORIENTED_EDGE('',*,*,#13063,.F.);
#17759=ORIENTED_EDGE('',*,*,#13032,.F.);
#17760=ORIENTED_EDGE('',*,*,#13063,.T.);
#17761=ORIENTED_EDGE('',*,*,#13050,.F.);
#17762=ORIENTED_EDGE('',*,*,#13064,.T.);
#17763=ORIENTED_EDGE('',*,*,#13048,.F.);
#17764=ORIENTED_EDGE('',*,*,#13030,.F.);
#17765=ORIENTED_EDGE('',*,*,#13064,.F.);
#17766=ORIENTED_EDGE('',*,*,#13053,.F.);
#17767=ORIENTED_EDGE('',*,*,#13065,.F.);
#17768=ORIENTED_EDGE('',*,*,#13023,.F.);
#17769=ORIENTED_EDGE('',*,*,#13021,.F.);
#17770=ORIENTED_EDGE('',*,*,#13065,.T.);
#17771=ORIENTED_EDGE('',*,*,#13055,.F.);
#17772=ORIENTED_EDGE('',*,*,#13066,.T.);
#17773=ORIENTED_EDGE('',*,*,#13019,.F.);
#17774=ORIENTED_EDGE('',*,*,#13066,.F.);
#17775=ORIENTED_EDGE('',*,*,#13057,.F.);
#17776=ORIENTED_EDGE('',*,*,#13067,.F.);
#17777=ORIENTED_EDGE('',*,*,#13017,.F.);
#17778=ORIENTED_EDGE('',*,*,#13067,.T.);
#17779=ORIENTED_EDGE('',*,*,#13059,.F.);
#17780=ORIENTED_EDGE('',*,*,#13045,.T.);
#17781=ORIENTED_EDGE('',*,*,#13068,.T.);
#17782=ORIENTED_EDGE('',*,*,#13069,.T.);
#17783=ORIENTED_EDGE('',*,*,#13070,.F.);
#17784=ORIENTED_EDGE('',*,*,#13069,.F.);
#17785=ORIENTED_EDGE('',*,*,#13070,.T.);
#17786=ORIENTED_EDGE('',*,*,#13071,.T.);
#17787=ORIENTED_EDGE('',*,*,#13072,.F.);
#17788=ORIENTED_EDGE('',*,*,#13071,.F.);
#17789=ORIENTED_EDGE('',*,*,#13073,.F.);
#17790=ORIENTED_EDGE('',*,*,#13074,.T.);
#17791=ORIENTED_EDGE('',*,*,#13072,.T.);
#17792=ORIENTED_EDGE('',*,*,#13074,.F.);
#17793=ORIENTED_EDGE('',*,*,#13068,.F.);
#17794=ORIENTED_EDGE('',*,*,#13075,.T.);
#17795=ORIENTED_EDGE('',*,*,#13073,.T.);
#17796=ORIENTED_EDGE('',*,*,#13075,.F.);
#17797=ORIENTED_EDGE('',*,*,#13076,.F.);
#17798=ORIENTED_EDGE('',*,*,#13077,.T.);
#17799=ORIENTED_EDGE('',*,*,#13078,.T.);
#17800=ORIENTED_EDGE('',*,*,#13079,.T.);
#17801=ORIENTED_EDGE('',*,*,#13080,.T.);
#17802=ORIENTED_EDGE('',*,*,#13079,.F.);
#17803=ORIENTED_EDGE('',*,*,#13081,.T.);
#17804=ORIENTED_EDGE('',*,*,#13082,.T.);
#17805=ORIENTED_EDGE('',*,*,#13083,.F.);
#17806=ORIENTED_EDGE('',*,*,#13084,.T.);
#17807=ORIENTED_EDGE('',*,*,#13076,.T.);
#17808=ORIENTED_EDGE('',*,*,#13085,.T.);
#17809=ORIENTED_EDGE('',*,*,#13086,.F.);
#17810=ORIENTED_EDGE('',*,*,#13087,.T.);
#17811=ORIENTED_EDGE('',*,*,#13083,.T.);
#17812=ORIENTED_EDGE('',*,*,#13088,.T.);
#17813=ORIENTED_EDGE('',*,*,#13089,.F.);
#17814=ORIENTED_EDGE('',*,*,#13090,.T.);
#17815=ORIENTED_EDGE('',*,*,#13086,.T.);
#17816=ORIENTED_EDGE('',*,*,#13091,.T.);
#17817=ORIENTED_EDGE('',*,*,#13092,.F.);
#17818=ORIENTED_EDGE('',*,*,#13093,.T.);
#17819=ORIENTED_EDGE('',*,*,#13089,.T.);
#17820=ORIENTED_EDGE('',*,*,#13094,.T.);
#17821=ORIENTED_EDGE('',*,*,#13095,.F.);
#17822=ORIENTED_EDGE('',*,*,#13096,.T.);
#17823=ORIENTED_EDGE('',*,*,#13092,.T.);
#17824=ORIENTED_EDGE('',*,*,#13097,.T.);
#17825=ORIENTED_EDGE('',*,*,#13098,.F.);
#17826=ORIENTED_EDGE('',*,*,#13099,.T.);
#17827=ORIENTED_EDGE('',*,*,#13095,.T.);
#17828=ORIENTED_EDGE('',*,*,#13100,.T.);
#17829=ORIENTED_EDGE('',*,*,#13101,.F.);
#17830=ORIENTED_EDGE('',*,*,#13102,.T.);
#17831=ORIENTED_EDGE('',*,*,#13098,.T.);
#17832=ORIENTED_EDGE('',*,*,#13103,.T.);
#17833=ORIENTED_EDGE('',*,*,#13104,.F.);
#17834=ORIENTED_EDGE('',*,*,#13105,.T.);
#17835=ORIENTED_EDGE('',*,*,#13101,.T.);
#17836=ORIENTED_EDGE('',*,*,#13106,.T.);
#17837=ORIENTED_EDGE('',*,*,#13107,.F.);
#17838=ORIENTED_EDGE('',*,*,#13108,.T.);
#17839=ORIENTED_EDGE('',*,*,#13104,.T.);
#17840=ORIENTED_EDGE('',*,*,#13109,.T.);
#17841=ORIENTED_EDGE('',*,*,#13110,.F.);
#17842=ORIENTED_EDGE('',*,*,#13111,.T.);
#17843=ORIENTED_EDGE('',*,*,#13107,.T.);
#17844=ORIENTED_EDGE('',*,*,#13112,.T.);
#17845=ORIENTED_EDGE('',*,*,#13113,.F.);
#17846=ORIENTED_EDGE('',*,*,#13114,.T.);
#17847=ORIENTED_EDGE('',*,*,#13110,.T.);
#17848=ORIENTED_EDGE('',*,*,#13115,.T.);
#17849=ORIENTED_EDGE('',*,*,#13116,.F.);
#17850=ORIENTED_EDGE('',*,*,#13117,.T.);
#17851=ORIENTED_EDGE('',*,*,#13113,.T.);
#17852=ORIENTED_EDGE('',*,*,#13118,.T.);
#17853=ORIENTED_EDGE('',*,*,#13119,.F.);
#17854=ORIENTED_EDGE('',*,*,#13120,.T.);
#17855=ORIENTED_EDGE('',*,*,#13116,.T.);
#17856=ORIENTED_EDGE('',*,*,#13121,.T.);
#17857=ORIENTED_EDGE('',*,*,#13122,.F.);
#17858=ORIENTED_EDGE('',*,*,#13123,.T.);
#17859=ORIENTED_EDGE('',*,*,#13124,.F.);
#17860=ORIENTED_EDGE('',*,*,#13125,.F.);
#17861=ORIENTED_EDGE('',*,*,#13126,.F.);
#17862=ORIENTED_EDGE('',*,*,#13127,.T.);
#17863=ORIENTED_EDGE('',*,*,#13122,.T.);
#17864=ORIENTED_EDGE('',*,*,#13128,.F.);
#17865=ORIENTED_EDGE('',*,*,#13129,.F.);
#17866=ORIENTED_EDGE('',*,*,#13130,.T.);
#17867=ORIENTED_EDGE('',*,*,#13126,.T.);
#17868=ORIENTED_EDGE('',*,*,#13131,.F.);
#17869=ORIENTED_EDGE('',*,*,#13132,.F.);
#17870=ORIENTED_EDGE('',*,*,#13133,.T.);
#17871=ORIENTED_EDGE('',*,*,#13129,.T.);
#17872=ORIENTED_EDGE('',*,*,#13134,.F.);
#17873=ORIENTED_EDGE('',*,*,#13135,.F.);
#17874=ORIENTED_EDGE('',*,*,#13136,.T.);
#17875=ORIENTED_EDGE('',*,*,#13132,.T.);
#17876=ORIENTED_EDGE('',*,*,#13137,.F.);
#17877=ORIENTED_EDGE('',*,*,#13138,.F.);
#17878=ORIENTED_EDGE('',*,*,#13139,.T.);
#17879=ORIENTED_EDGE('',*,*,#13135,.T.);
#17880=ORIENTED_EDGE('',*,*,#13140,.F.);
#17881=ORIENTED_EDGE('',*,*,#13141,.F.);
#17882=ORIENTED_EDGE('',*,*,#13142,.T.);
#17883=ORIENTED_EDGE('',*,*,#13138,.T.);
#17884=ORIENTED_EDGE('',*,*,#13143,.F.);
#17885=ORIENTED_EDGE('',*,*,#13144,.F.);
#17886=ORIENTED_EDGE('',*,*,#13145,.T.);
#17887=ORIENTED_EDGE('',*,*,#13141,.T.);
#17888=ORIENTED_EDGE('',*,*,#13146,.F.);
#17889=ORIENTED_EDGE('',*,*,#13147,.F.);
#17890=ORIENTED_EDGE('',*,*,#13148,.T.);
#17891=ORIENTED_EDGE('',*,*,#13144,.T.);
#17892=ORIENTED_EDGE('',*,*,#13149,.F.);
#17893=ORIENTED_EDGE('',*,*,#13150,.F.);
#17894=ORIENTED_EDGE('',*,*,#13151,.T.);
#17895=ORIENTED_EDGE('',*,*,#13147,.T.);
#17896=ORIENTED_EDGE('',*,*,#13152,.F.);
#17897=ORIENTED_EDGE('',*,*,#13153,.F.);
#17898=ORIENTED_EDGE('',*,*,#13154,.T.);
#17899=ORIENTED_EDGE('',*,*,#13150,.T.);
#17900=ORIENTED_EDGE('',*,*,#13155,.F.);
#17901=ORIENTED_EDGE('',*,*,#13156,.F.);
#17902=ORIENTED_EDGE('',*,*,#13157,.T.);
#17903=ORIENTED_EDGE('',*,*,#13153,.T.);
#17904=ORIENTED_EDGE('',*,*,#13158,.F.);
#17905=ORIENTED_EDGE('',*,*,#13159,.F.);
#17906=ORIENTED_EDGE('',*,*,#13160,.T.);
#17907=ORIENTED_EDGE('',*,*,#13156,.T.);
#17908=ORIENTED_EDGE('',*,*,#13161,.F.);
#17909=ORIENTED_EDGE('',*,*,#13162,.F.);
#17910=ORIENTED_EDGE('',*,*,#13163,.T.);
#17911=ORIENTED_EDGE('',*,*,#13159,.T.);
#17912=ORIENTED_EDGE('',*,*,#13164,.F.);
#17913=ORIENTED_EDGE('',*,*,#13165,.F.);
#17914=ORIENTED_EDGE('',*,*,#13166,.F.);
#17915=ORIENTED_EDGE('',*,*,#13167,.T.);
#17916=ORIENTED_EDGE('',*,*,#13162,.T.);
#17917=ORIENTED_EDGE('',*,*,#13168,.F.);
#17918=ORIENTED_EDGE('',*,*,#13169,.F.);
#17919=ORIENTED_EDGE('',*,*,#13170,.F.);
#17920=ORIENTED_EDGE('',*,*,#13121,.F.);
#17921=ORIENTED_EDGE('',*,*,#13118,.F.);
#17922=ORIENTED_EDGE('',*,*,#13115,.F.);
#17923=ORIENTED_EDGE('',*,*,#13112,.F.);
#17924=ORIENTED_EDGE('',*,*,#13109,.F.);
#17925=ORIENTED_EDGE('',*,*,#13106,.F.);
#17926=ORIENTED_EDGE('',*,*,#13103,.F.);
#17927=ORIENTED_EDGE('',*,*,#13100,.F.);
#17928=ORIENTED_EDGE('',*,*,#13097,.F.);
#17929=ORIENTED_EDGE('',*,*,#13094,.F.);
#17930=ORIENTED_EDGE('',*,*,#13091,.F.);
#17931=ORIENTED_EDGE('',*,*,#13088,.F.);
#17932=ORIENTED_EDGE('',*,*,#13085,.F.);
#17933=ORIENTED_EDGE('',*,*,#13082,.F.);
#17934=ORIENTED_EDGE('',*,*,#13171,.F.);
#17935=ORIENTED_EDGE('',*,*,#13172,.T.);
#17936=ORIENTED_EDGE('',*,*,#13168,.T.);
#17937=ORIENTED_EDGE('',*,*,#13164,.T.);
#17938=ORIENTED_EDGE('',*,*,#13161,.T.);
#17939=ORIENTED_EDGE('',*,*,#13158,.T.);
#17940=ORIENTED_EDGE('',*,*,#13155,.T.);
#17941=ORIENTED_EDGE('',*,*,#13152,.T.);
#17942=ORIENTED_EDGE('',*,*,#13149,.T.);
#17943=ORIENTED_EDGE('',*,*,#13146,.T.);
#17944=ORIENTED_EDGE('',*,*,#13143,.T.);
#17945=ORIENTED_EDGE('',*,*,#13140,.T.);
#17946=ORIENTED_EDGE('',*,*,#13137,.T.);
#17947=ORIENTED_EDGE('',*,*,#13134,.T.);
#17948=ORIENTED_EDGE('',*,*,#13131,.T.);
#17949=ORIENTED_EDGE('',*,*,#13128,.T.);
#17950=ORIENTED_EDGE('',*,*,#13125,.T.);
#17951=ORIENTED_EDGE('',*,*,#13078,.F.);
#17952=ORIENTED_EDGE('',*,*,#13173,.T.);
#17953=ORIENTED_EDGE('',*,*,#13166,.T.);
#17954=ORIENTED_EDGE('',*,*,#13174,.T.);
#17955=ORIENTED_EDGE('',*,*,#13171,.T.);
#17956=ORIENTED_EDGE('',*,*,#13081,.F.);
#17957=ORIENTED_EDGE('',*,*,#13165,.T.);
#17958=ORIENTED_EDGE('',*,*,#13172,.F.);
#17959=ORIENTED_EDGE('',*,*,#13174,.F.);
#17960=ORIENTED_EDGE('',*,*,#13175,.F.);
#17961=ORIENTED_EDGE('',*,*,#13123,.F.);
#17962=ORIENTED_EDGE('',*,*,#13127,.F.);
#17963=ORIENTED_EDGE('',*,*,#13130,.F.);
#17964=ORIENTED_EDGE('',*,*,#13133,.F.);
#17965=ORIENTED_EDGE('',*,*,#13136,.F.);
#17966=ORIENTED_EDGE('',*,*,#13139,.F.);
#17967=ORIENTED_EDGE('',*,*,#13142,.F.);
#17968=ORIENTED_EDGE('',*,*,#13145,.F.);
#17969=ORIENTED_EDGE('',*,*,#13148,.F.);
#17970=ORIENTED_EDGE('',*,*,#13151,.F.);
#17971=ORIENTED_EDGE('',*,*,#13154,.F.);
#17972=ORIENTED_EDGE('',*,*,#13157,.F.);
#17973=ORIENTED_EDGE('',*,*,#13160,.F.);
#17974=ORIENTED_EDGE('',*,*,#13163,.F.);
#17975=ORIENTED_EDGE('',*,*,#13167,.F.);
#17976=ORIENTED_EDGE('',*,*,#13173,.F.);
#17977=ORIENTED_EDGE('',*,*,#13077,.F.);
#17978=ORIENTED_EDGE('',*,*,#13084,.F.);
#17979=ORIENTED_EDGE('',*,*,#13087,.F.);
#17980=ORIENTED_EDGE('',*,*,#13090,.F.);
#17981=ORIENTED_EDGE('',*,*,#13093,.F.);
#17982=ORIENTED_EDGE('',*,*,#13096,.F.);
#17983=ORIENTED_EDGE('',*,*,#13099,.F.);
#17984=ORIENTED_EDGE('',*,*,#13102,.F.);
#17985=ORIENTED_EDGE('',*,*,#13105,.F.);
#17986=ORIENTED_EDGE('',*,*,#13108,.F.);
#17987=ORIENTED_EDGE('',*,*,#13111,.F.);
#17988=ORIENTED_EDGE('',*,*,#13114,.F.);
#17989=ORIENTED_EDGE('',*,*,#13117,.F.);
#17990=ORIENTED_EDGE('',*,*,#13120,.F.);
#17991=ORIENTED_EDGE('',*,*,#13176,.F.);
#17992=ORIENTED_EDGE('',*,*,#13119,.T.);
#17993=ORIENTED_EDGE('',*,*,#13170,.T.);
#17994=ORIENTED_EDGE('',*,*,#13177,.F.);
#17995=ORIENTED_EDGE('',*,*,#13176,.T.);
#17996=ORIENTED_EDGE('',*,*,#13178,.T.);
#17997=ORIENTED_EDGE('',*,*,#13179,.F.);
#17998=ORIENTED_EDGE('',*,*,#13178,.F.);
#17999=ORIENTED_EDGE('',*,*,#13180,.F.);
#18000=ORIENTED_EDGE('',*,*,#13181,.F.);
#18001=ORIENTED_EDGE('',*,*,#13182,.T.);
#18002=ORIENTED_EDGE('',*,*,#13183,.T.);
#18003=ORIENTED_EDGE('',*,*,#13184,.F.);
#18004=ORIENTED_EDGE('',*,*,#13183,.F.);
#18005=ORIENTED_EDGE('',*,*,#13185,.F.);
#18006=ORIENTED_EDGE('',*,*,#13186,.F.);
#18007=ORIENTED_EDGE('',*,*,#13185,.T.);
#18008=ORIENTED_EDGE('',*,*,#13182,.F.);
#18009=ORIENTED_EDGE('',*,*,#13187,.F.);
#18010=ORIENTED_EDGE('',*,*,#13188,.F.);
#18011=ORIENTED_EDGE('',*,*,#13187,.T.);
#18012=ORIENTED_EDGE('',*,*,#13181,.T.);
#18013=ORIENTED_EDGE('',*,*,#13189,.F.);
#18014=ORIENTED_EDGE('',*,*,#13190,.F.);
#18015=ORIENTED_EDGE('',*,*,#13191,.T.);
#18016=ORIENTED_EDGE('',*,*,#13192,.T.);
#18017=ORIENTED_EDGE('',*,*,#13193,.F.);
#18018=ORIENTED_EDGE('',*,*,#13192,.F.);
#18019=ORIENTED_EDGE('',*,*,#13194,.F.);
#18020=ORIENTED_EDGE('',*,*,#13195,.F.);
#18021=ORIENTED_EDGE('',*,*,#13194,.T.);
#18022=ORIENTED_EDGE('',*,*,#13191,.F.);
#18023=ORIENTED_EDGE('',*,*,#13196,.F.);
#18024=ORIENTED_EDGE('',*,*,#13197,.F.);
#18025=ORIENTED_EDGE('',*,*,#13196,.T.);
#18026=ORIENTED_EDGE('',*,*,#13190,.T.);
#18027=ORIENTED_EDGE('',*,*,#13198,.F.);
#18028=ORIENTED_EDGE('',*,*,#13199,.F.);
#18029=ORIENTED_EDGE('',*,*,#13200,.T.);
#18030=ORIENTED_EDGE('',*,*,#13201,.T.);
#18031=ORIENTED_EDGE('',*,*,#13202,.F.);
#18032=ORIENTED_EDGE('',*,*,#13201,.F.);
#18033=ORIENTED_EDGE('',*,*,#13203,.F.);
#18034=ORIENTED_EDGE('',*,*,#13204,.F.);
#18035=ORIENTED_EDGE('',*,*,#13203,.T.);
#18036=ORIENTED_EDGE('',*,*,#13200,.F.);
#18037=ORIENTED_EDGE('',*,*,#13205,.F.);
#18038=ORIENTED_EDGE('',*,*,#13206,.F.);
#18039=ORIENTED_EDGE('',*,*,#13205,.T.);
#18040=ORIENTED_EDGE('',*,*,#13199,.T.);
#18041=ORIENTED_EDGE('',*,*,#13207,.F.);
#18042=ORIENTED_EDGE('',*,*,#13208,.F.);
#18043=ORIENTED_EDGE('',*,*,#13209,.T.);
#18044=ORIENTED_EDGE('',*,*,#13210,.T.);
#18045=ORIENTED_EDGE('',*,*,#13211,.F.);
#18046=ORIENTED_EDGE('',*,*,#13210,.F.);
#18047=ORIENTED_EDGE('',*,*,#13212,.F.);
#18048=ORIENTED_EDGE('',*,*,#13213,.F.);
#18049=ORIENTED_EDGE('',*,*,#13212,.T.);
#18050=ORIENTED_EDGE('',*,*,#13209,.F.);
#18051=ORIENTED_EDGE('',*,*,#13214,.F.);
#18052=ORIENTED_EDGE('',*,*,#13215,.F.);
#18053=ORIENTED_EDGE('',*,*,#13214,.T.);
#18054=ORIENTED_EDGE('',*,*,#13208,.T.);
#18055=ORIENTED_EDGE('',*,*,#13216,.F.);
#18056=ORIENTED_EDGE('',*,*,#13217,.F.);
#18057=ORIENTED_EDGE('',*,*,#13218,.T.);
#18058=ORIENTED_EDGE('',*,*,#13219,.T.);
#18059=ORIENTED_EDGE('',*,*,#13220,.F.);
#18060=ORIENTED_EDGE('',*,*,#13219,.F.);
#18061=ORIENTED_EDGE('',*,*,#13221,.F.);
#18062=ORIENTED_EDGE('',*,*,#13222,.F.);
#18063=ORIENTED_EDGE('',*,*,#13221,.T.);
#18064=ORIENTED_EDGE('',*,*,#13218,.F.);
#18065=ORIENTED_EDGE('',*,*,#13223,.F.);
#18066=ORIENTED_EDGE('',*,*,#13224,.F.);
#18067=ORIENTED_EDGE('',*,*,#13223,.T.);
#18068=ORIENTED_EDGE('',*,*,#13217,.T.);
#18069=ORIENTED_EDGE('',*,*,#13225,.F.);
#18070=ORIENTED_EDGE('',*,*,#13226,.F.);
#18071=ORIENTED_EDGE('',*,*,#13227,.T.);
#18072=ORIENTED_EDGE('',*,*,#13228,.T.);
#18073=ORIENTED_EDGE('',*,*,#13229,.F.);
#18074=ORIENTED_EDGE('',*,*,#13228,.F.);
#18075=ORIENTED_EDGE('',*,*,#13230,.F.);
#18076=ORIENTED_EDGE('',*,*,#13231,.F.);
#18077=ORIENTED_EDGE('',*,*,#13230,.T.);
#18078=ORIENTED_EDGE('',*,*,#13227,.F.);
#18079=ORIENTED_EDGE('',*,*,#13232,.F.);
#18080=ORIENTED_EDGE('',*,*,#13233,.F.);
#18081=ORIENTED_EDGE('',*,*,#13232,.T.);
#18082=ORIENTED_EDGE('',*,*,#13226,.T.);
#18083=ORIENTED_EDGE('',*,*,#13234,.F.);
#18084=ORIENTED_EDGE('',*,*,#13235,.F.);
#18085=ORIENTED_EDGE('',*,*,#13236,.T.);
#18086=ORIENTED_EDGE('',*,*,#13237,.T.);
#18087=ORIENTED_EDGE('',*,*,#13238,.F.);
#18088=ORIENTED_EDGE('',*,*,#13237,.F.);
#18089=ORIENTED_EDGE('',*,*,#13239,.F.);
#18090=ORIENTED_EDGE('',*,*,#13240,.F.);
#18091=ORIENTED_EDGE('',*,*,#13239,.T.);
#18092=ORIENTED_EDGE('',*,*,#13236,.F.);
#18093=ORIENTED_EDGE('',*,*,#13241,.F.);
#18094=ORIENTED_EDGE('',*,*,#13242,.F.);
#18095=ORIENTED_EDGE('',*,*,#13241,.T.);
#18096=ORIENTED_EDGE('',*,*,#13235,.T.);
#18097=ORIENTED_EDGE('',*,*,#13243,.F.);
#18098=ORIENTED_EDGE('',*,*,#13244,.F.);
#18099=ORIENTED_EDGE('',*,*,#13245,.T.);
#18100=ORIENTED_EDGE('',*,*,#13246,.T.);
#18101=ORIENTED_EDGE('',*,*,#13247,.F.);
#18102=ORIENTED_EDGE('',*,*,#13246,.F.);
#18103=ORIENTED_EDGE('',*,*,#13248,.F.);
#18104=ORIENTED_EDGE('',*,*,#13249,.F.);
#18105=ORIENTED_EDGE('',*,*,#13248,.T.);
#18106=ORIENTED_EDGE('',*,*,#13245,.F.);
#18107=ORIENTED_EDGE('',*,*,#13250,.F.);
#18108=ORIENTED_EDGE('',*,*,#13251,.F.);
#18109=ORIENTED_EDGE('',*,*,#13250,.T.);
#18110=ORIENTED_EDGE('',*,*,#13244,.T.);
#18111=ORIENTED_EDGE('',*,*,#13252,.F.);
#18112=ORIENTED_EDGE('',*,*,#13253,.F.);
#18113=ORIENTED_EDGE('',*,*,#13254,.T.);
#18114=ORIENTED_EDGE('',*,*,#13255,.T.);
#18115=ORIENTED_EDGE('',*,*,#13256,.F.);
#18116=ORIENTED_EDGE('',*,*,#13255,.F.);
#18117=ORIENTED_EDGE('',*,*,#13257,.F.);
#18118=ORIENTED_EDGE('',*,*,#13258,.F.);
#18119=ORIENTED_EDGE('',*,*,#13257,.T.);
#18120=ORIENTED_EDGE('',*,*,#13254,.F.);
#18121=ORIENTED_EDGE('',*,*,#13259,.F.);
#18122=ORIENTED_EDGE('',*,*,#13260,.F.);
#18123=ORIENTED_EDGE('',*,*,#13259,.T.);
#18124=ORIENTED_EDGE('',*,*,#13253,.T.);
#18125=ORIENTED_EDGE('',*,*,#13261,.F.);
#18126=ORIENTED_EDGE('',*,*,#13262,.F.);
#18127=ORIENTED_EDGE('',*,*,#13263,.T.);
#18128=ORIENTED_EDGE('',*,*,#13264,.T.);
#18129=ORIENTED_EDGE('',*,*,#13265,.F.);
#18130=ORIENTED_EDGE('',*,*,#13264,.F.);
#18131=ORIENTED_EDGE('',*,*,#13266,.F.);
#18132=ORIENTED_EDGE('',*,*,#13267,.F.);
#18133=ORIENTED_EDGE('',*,*,#13266,.T.);
#18134=ORIENTED_EDGE('',*,*,#13263,.F.);
#18135=ORIENTED_EDGE('',*,*,#13268,.F.);
#18136=ORIENTED_EDGE('',*,*,#13269,.F.);
#18137=ORIENTED_EDGE('',*,*,#13268,.T.);
#18138=ORIENTED_EDGE('',*,*,#13262,.T.);
#18139=ORIENTED_EDGE('',*,*,#13270,.F.);
#18140=ORIENTED_EDGE('',*,*,#13271,.F.);
#18141=ORIENTED_EDGE('',*,*,#13272,.T.);
#18142=ORIENTED_EDGE('',*,*,#13273,.T.);
#18143=ORIENTED_EDGE('',*,*,#13274,.F.);
#18144=ORIENTED_EDGE('',*,*,#13273,.F.);
#18145=ORIENTED_EDGE('',*,*,#13275,.F.);
#18146=ORIENTED_EDGE('',*,*,#13276,.F.);
#18147=ORIENTED_EDGE('',*,*,#13275,.T.);
#18148=ORIENTED_EDGE('',*,*,#13272,.F.);
#18149=ORIENTED_EDGE('',*,*,#13277,.F.);
#18150=ORIENTED_EDGE('',*,*,#13278,.F.);
#18151=ORIENTED_EDGE('',*,*,#13277,.T.);
#18152=ORIENTED_EDGE('',*,*,#13271,.T.);
#18153=ORIENTED_EDGE('',*,*,#13279,.F.);
#18154=ORIENTED_EDGE('',*,*,#13280,.F.);
#18155=ORIENTED_EDGE('',*,*,#13281,.T.);
#18156=ORIENTED_EDGE('',*,*,#13282,.T.);
#18157=ORIENTED_EDGE('',*,*,#13283,.F.);
#18158=ORIENTED_EDGE('',*,*,#13282,.F.);
#18159=ORIENTED_EDGE('',*,*,#13284,.F.);
#18160=ORIENTED_EDGE('',*,*,#13285,.F.);
#18161=ORIENTED_EDGE('',*,*,#13286,.F.);
#18162=ORIENTED_EDGE('',*,*,#13284,.T.);
#18163=ORIENTED_EDGE('',*,*,#13281,.F.);
#18164=ORIENTED_EDGE('',*,*,#13287,.F.);
#18165=ORIENTED_EDGE('',*,*,#13288,.F.);
#18166=ORIENTED_EDGE('',*,*,#13287,.T.);
#18167=ORIENTED_EDGE('',*,*,#13280,.T.);
#18168=ORIENTED_EDGE('',*,*,#13289,.F.);
#18169=ORIENTED_EDGE('',*,*,#13290,.F.);
#18170=ORIENTED_EDGE('',*,*,#13291,.F.);
#18171=ORIENTED_EDGE('',*,*,#13292,.T.);
#18172=ORIENTED_EDGE('',*,*,#13293,.T.);
#18173=ORIENTED_EDGE('',*,*,#13294,.F.);
#18174=ORIENTED_EDGE('',*,*,#13293,.F.);
#18175=ORIENTED_EDGE('',*,*,#13295,.F.);
#18176=ORIENTED_EDGE('',*,*,#13296,.F.);
#18177=ORIENTED_EDGE('',*,*,#13295,.T.);
#18178=ORIENTED_EDGE('',*,*,#13292,.F.);
#18179=ORIENTED_EDGE('',*,*,#13297,.F.);
#18180=ORIENTED_EDGE('',*,*,#13298,.F.);
#18181=ORIENTED_EDGE('',*,*,#13297,.T.);
#18182=ORIENTED_EDGE('',*,*,#13291,.T.);
#18183=ORIENTED_EDGE('',*,*,#13299,.F.);
#18184=ORIENTED_EDGE('',*,*,#13300,.F.);
#18185=ORIENTED_EDGE('',*,*,#13301,.T.);
#18186=ORIENTED_EDGE('',*,*,#13302,.T.);
#18187=ORIENTED_EDGE('',*,*,#13303,.F.);
#18188=ORIENTED_EDGE('',*,*,#13302,.F.);
#18189=ORIENTED_EDGE('',*,*,#13304,.F.);
#18190=ORIENTED_EDGE('',*,*,#13305,.F.);
#18191=ORIENTED_EDGE('',*,*,#13304,.T.);
#18192=ORIENTED_EDGE('',*,*,#13301,.F.);
#18193=ORIENTED_EDGE('',*,*,#13306,.F.);
#18194=ORIENTED_EDGE('',*,*,#13307,.F.);
#18195=ORIENTED_EDGE('',*,*,#13306,.T.);
#18196=ORIENTED_EDGE('',*,*,#13300,.T.);
#18197=ORIENTED_EDGE('',*,*,#13308,.F.);
#18198=ORIENTED_EDGE('',*,*,#13309,.F.);
#18199=ORIENTED_EDGE('',*,*,#13310,.T.);
#18200=ORIENTED_EDGE('',*,*,#13311,.T.);
#18201=ORIENTED_EDGE('',*,*,#13312,.F.);
#18202=ORIENTED_EDGE('',*,*,#13311,.F.);
#18203=ORIENTED_EDGE('',*,*,#13313,.F.);
#18204=ORIENTED_EDGE('',*,*,#13314,.F.);
#18205=ORIENTED_EDGE('',*,*,#13313,.T.);
#18206=ORIENTED_EDGE('',*,*,#13310,.F.);
#18207=ORIENTED_EDGE('',*,*,#13315,.F.);
#18208=ORIENTED_EDGE('',*,*,#13316,.F.);
#18209=ORIENTED_EDGE('',*,*,#13315,.T.);
#18210=ORIENTED_EDGE('',*,*,#13309,.T.);
#18211=ORIENTED_EDGE('',*,*,#13317,.F.);
#18212=ORIENTED_EDGE('',*,*,#13318,.F.);
#18213=ORIENTED_EDGE('',*,*,#13319,.T.);
#18214=ORIENTED_EDGE('',*,*,#13320,.T.);
#18215=ORIENTED_EDGE('',*,*,#13321,.F.);
#18216=ORIENTED_EDGE('',*,*,#13320,.F.);
#18217=ORIENTED_EDGE('',*,*,#13322,.F.);
#18218=ORIENTED_EDGE('',*,*,#13323,.F.);
#18219=ORIENTED_EDGE('',*,*,#13322,.T.);
#18220=ORIENTED_EDGE('',*,*,#13319,.F.);
#18221=ORIENTED_EDGE('',*,*,#13324,.F.);
#18222=ORIENTED_EDGE('',*,*,#13325,.F.);
#18223=ORIENTED_EDGE('',*,*,#13324,.T.);
#18224=ORIENTED_EDGE('',*,*,#13318,.T.);
#18225=ORIENTED_EDGE('',*,*,#13326,.F.);
#18226=ORIENTED_EDGE('',*,*,#13327,.F.);
#18227=ORIENTED_EDGE('',*,*,#13328,.T.);
#18228=ORIENTED_EDGE('',*,*,#13329,.T.);
#18229=ORIENTED_EDGE('',*,*,#13330,.F.);
#18230=ORIENTED_EDGE('',*,*,#13329,.F.);
#18231=ORIENTED_EDGE('',*,*,#13331,.F.);
#18232=ORIENTED_EDGE('',*,*,#13332,.F.);
#18233=ORIENTED_EDGE('',*,*,#13331,.T.);
#18234=ORIENTED_EDGE('',*,*,#13328,.F.);
#18235=ORIENTED_EDGE('',*,*,#13333,.F.);
#18236=ORIENTED_EDGE('',*,*,#13334,.F.);
#18237=ORIENTED_EDGE('',*,*,#13333,.T.);
#18238=ORIENTED_EDGE('',*,*,#13327,.T.);
#18239=ORIENTED_EDGE('',*,*,#13335,.F.);
#18240=ORIENTED_EDGE('',*,*,#13336,.F.);
#18241=ORIENTED_EDGE('',*,*,#13337,.T.);
#18242=ORIENTED_EDGE('',*,*,#13338,.T.);
#18243=ORIENTED_EDGE('',*,*,#13339,.F.);
#18244=ORIENTED_EDGE('',*,*,#13338,.F.);
#18245=ORIENTED_EDGE('',*,*,#13340,.F.);
#18246=ORIENTED_EDGE('',*,*,#13341,.F.);
#18247=ORIENTED_EDGE('',*,*,#13340,.T.);
#18248=ORIENTED_EDGE('',*,*,#13337,.F.);
#18249=ORIENTED_EDGE('',*,*,#13342,.F.);
#18250=ORIENTED_EDGE('',*,*,#13343,.F.);
#18251=ORIENTED_EDGE('',*,*,#13342,.T.);
#18252=ORIENTED_EDGE('',*,*,#13336,.T.);
#18253=ORIENTED_EDGE('',*,*,#13344,.F.);
#18254=ORIENTED_EDGE('',*,*,#13345,.F.);
#18255=ORIENTED_EDGE('',*,*,#13346,.T.);
#18256=ORIENTED_EDGE('',*,*,#13347,.T.);
#18257=ORIENTED_EDGE('',*,*,#13348,.F.);
#18258=ORIENTED_EDGE('',*,*,#13347,.F.);
#18259=ORIENTED_EDGE('',*,*,#13349,.F.);
#18260=ORIENTED_EDGE('',*,*,#13350,.F.);
#18261=ORIENTED_EDGE('',*,*,#13349,.T.);
#18262=ORIENTED_EDGE('',*,*,#13346,.F.);
#18263=ORIENTED_EDGE('',*,*,#13351,.F.);
#18264=ORIENTED_EDGE('',*,*,#13352,.F.);
#18265=ORIENTED_EDGE('',*,*,#13351,.T.);
#18266=ORIENTED_EDGE('',*,*,#13345,.T.);
#18267=ORIENTED_EDGE('',*,*,#13353,.F.);
#18268=ORIENTED_EDGE('',*,*,#13354,.F.);
#18269=ORIENTED_EDGE('',*,*,#13355,.T.);
#18270=ORIENTED_EDGE('',*,*,#13356,.T.);
#18271=ORIENTED_EDGE('',*,*,#13357,.F.);
#18272=ORIENTED_EDGE('',*,*,#13356,.F.);
#18273=ORIENTED_EDGE('',*,*,#13358,.F.);
#18274=ORIENTED_EDGE('',*,*,#13359,.F.);
#18275=ORIENTED_EDGE('',*,*,#13358,.T.);
#18276=ORIENTED_EDGE('',*,*,#13355,.F.);
#18277=ORIENTED_EDGE('',*,*,#13360,.F.);
#18278=ORIENTED_EDGE('',*,*,#13361,.F.);
#18279=ORIENTED_EDGE('',*,*,#13360,.T.);
#18280=ORIENTED_EDGE('',*,*,#13354,.T.);
#18281=ORIENTED_EDGE('',*,*,#13362,.F.);
#18282=ORIENTED_EDGE('',*,*,#13363,.F.);
#18283=ORIENTED_EDGE('',*,*,#13364,.T.);
#18284=ORIENTED_EDGE('',*,*,#13365,.T.);
#18285=ORIENTED_EDGE('',*,*,#13366,.F.);
#18286=ORIENTED_EDGE('',*,*,#13365,.F.);
#18287=ORIENTED_EDGE('',*,*,#13367,.F.);
#18288=ORIENTED_EDGE('',*,*,#13368,.F.);
#18289=ORIENTED_EDGE('',*,*,#13367,.T.);
#18290=ORIENTED_EDGE('',*,*,#13364,.F.);
#18291=ORIENTED_EDGE('',*,*,#13369,.F.);
#18292=ORIENTED_EDGE('',*,*,#13370,.F.);
#18293=ORIENTED_EDGE('',*,*,#13369,.T.);
#18294=ORIENTED_EDGE('',*,*,#13363,.T.);
#18295=ORIENTED_EDGE('',*,*,#13371,.F.);
#18296=ORIENTED_EDGE('',*,*,#13372,.F.);
#18297=ORIENTED_EDGE('',*,*,#13373,.T.);
#18298=ORIENTED_EDGE('',*,*,#13374,.T.);
#18299=ORIENTED_EDGE('',*,*,#13375,.F.);
#18300=ORIENTED_EDGE('',*,*,#13374,.F.);
#18301=ORIENTED_EDGE('',*,*,#13376,.F.);
#18302=ORIENTED_EDGE('',*,*,#13377,.F.);
#18303=ORIENTED_EDGE('',*,*,#13376,.T.);
#18304=ORIENTED_EDGE('',*,*,#13373,.F.);
#18305=ORIENTED_EDGE('',*,*,#13378,.F.);
#18306=ORIENTED_EDGE('',*,*,#13379,.F.);
#18307=ORIENTED_EDGE('',*,*,#13378,.T.);
#18308=ORIENTED_EDGE('',*,*,#13372,.T.);
#18309=ORIENTED_EDGE('',*,*,#13380,.F.);
#18310=ORIENTED_EDGE('',*,*,#13381,.F.);
#18311=ORIENTED_EDGE('',*,*,#13382,.T.);
#18312=ORIENTED_EDGE('',*,*,#13383,.T.);
#18313=ORIENTED_EDGE('',*,*,#13384,.F.);
#18314=ORIENTED_EDGE('',*,*,#13383,.F.);
#18315=ORIENTED_EDGE('',*,*,#13385,.F.);
#18316=ORIENTED_EDGE('',*,*,#13386,.F.);
#18317=ORIENTED_EDGE('',*,*,#13385,.T.);
#18318=ORIENTED_EDGE('',*,*,#13382,.F.);
#18319=ORIENTED_EDGE('',*,*,#13387,.F.);
#18320=ORIENTED_EDGE('',*,*,#13388,.F.);
#18321=ORIENTED_EDGE('',*,*,#13387,.T.);
#18322=ORIENTED_EDGE('',*,*,#13381,.T.);
#18323=ORIENTED_EDGE('',*,*,#13389,.F.);
#18324=ORIENTED_EDGE('',*,*,#13390,.F.);
#18325=ORIENTED_EDGE('',*,*,#13391,.T.);
#18326=ORIENTED_EDGE('',*,*,#13392,.T.);
#18327=ORIENTED_EDGE('',*,*,#13393,.F.);
#18328=ORIENTED_EDGE('',*,*,#13392,.F.);
#18329=ORIENTED_EDGE('',*,*,#13394,.F.);
#18330=ORIENTED_EDGE('',*,*,#13395,.F.);
#18331=ORIENTED_EDGE('',*,*,#13394,.T.);
#18332=ORIENTED_EDGE('',*,*,#13391,.F.);
#18333=ORIENTED_EDGE('',*,*,#13396,.F.);
#18334=ORIENTED_EDGE('',*,*,#13397,.F.);
#18335=ORIENTED_EDGE('',*,*,#13396,.T.);
#18336=ORIENTED_EDGE('',*,*,#13390,.T.);
#18337=ORIENTED_EDGE('',*,*,#13398,.F.);
#18338=ORIENTED_EDGE('',*,*,#13080,.F.);
#18339=ORIENTED_EDGE('',*,*,#13399,.T.);
#18340=ORIENTED_EDGE('',*,*,#13398,.T.);
#18341=ORIENTED_EDGE('',*,*,#13399,.F.);
#18342=ORIENTED_EDGE('',*,*,#13400,.F.);
#18343=ORIENTED_EDGE('',*,*,#13177,.T.);
#18344=ORIENTED_EDGE('',*,*,#13169,.T.);
#18345=ORIENTED_EDGE('',*,*,#13124,.T.);
#18346=ORIENTED_EDGE('',*,*,#13175,.T.);
#18347=ORIENTED_EDGE('',*,*,#13401,.F.);
#18348=ORIENTED_EDGE('',*,*,#13402,.T.);
#18349=ORIENTED_EDGE('',*,*,#13400,.T.);
#18350=ORIENTED_EDGE('',*,*,#13402,.F.);
#18351=ORIENTED_EDGE('',*,*,#13403,.F.);
#18352=ORIENTED_EDGE('',*,*,#13404,.T.);
#18353=ORIENTED_EDGE('',*,*,#13285,.T.);
#18354=ORIENTED_EDGE('',*,*,#13286,.T.);
#18355=ORIENTED_EDGE('',*,*,#13288,.T.);
#18356=ORIENTED_EDGE('',*,*,#13405,.T.);
#18357=ORIENTED_EDGE('',*,*,#13401,.T.);
#18358=ORIENTED_EDGE('',*,*,#13405,.F.);
#18359=ORIENTED_EDGE('',*,*,#13289,.T.);
#18360=ORIENTED_EDGE('',*,*,#13279,.T.);
#18361=ORIENTED_EDGE('',*,*,#13283,.T.);
#18362=ORIENTED_EDGE('',*,*,#13404,.F.);
#18363=ORIENTED_EDGE('',*,*,#13186,.T.);
#18364=ORIENTED_EDGE('',*,*,#13188,.T.);
#18365=ORIENTED_EDGE('',*,*,#13180,.T.);
#18366=ORIENTED_EDGE('',*,*,#13184,.T.);
#18367=ORIENTED_EDGE('',*,*,#13195,.T.);
#18368=ORIENTED_EDGE('',*,*,#13197,.T.);
#18369=ORIENTED_EDGE('',*,*,#13189,.T.);
#18370=ORIENTED_EDGE('',*,*,#13193,.T.);
#18371=ORIENTED_EDGE('',*,*,#13204,.T.);
#18372=ORIENTED_EDGE('',*,*,#13206,.T.);
#18373=ORIENTED_EDGE('',*,*,#13198,.T.);
#18374=ORIENTED_EDGE('',*,*,#13202,.T.);
#18375=ORIENTED_EDGE('',*,*,#13213,.T.);
#18376=ORIENTED_EDGE('',*,*,#13215,.T.);
#18377=ORIENTED_EDGE('',*,*,#13207,.T.);
#18378=ORIENTED_EDGE('',*,*,#13211,.T.);
#18379=ORIENTED_EDGE('',*,*,#13222,.T.);
#18380=ORIENTED_EDGE('',*,*,#13224,.T.);
#18381=ORIENTED_EDGE('',*,*,#13216,.T.);
#18382=ORIENTED_EDGE('',*,*,#13220,.T.);
#18383=ORIENTED_EDGE('',*,*,#13231,.T.);
#18384=ORIENTED_EDGE('',*,*,#13233,.T.);
#18385=ORIENTED_EDGE('',*,*,#13225,.T.);
#18386=ORIENTED_EDGE('',*,*,#13229,.T.);
#18387=ORIENTED_EDGE('',*,*,#13240,.T.);
#18388=ORIENTED_EDGE('',*,*,#13242,.T.);
#18389=ORIENTED_EDGE('',*,*,#13234,.T.);
#18390=ORIENTED_EDGE('',*,*,#13238,.T.);
#18391=ORIENTED_EDGE('',*,*,#13249,.T.);
#18392=ORIENTED_EDGE('',*,*,#13251,.T.);
#18393=ORIENTED_EDGE('',*,*,#13243,.T.);
#18394=ORIENTED_EDGE('',*,*,#13247,.T.);
#18395=ORIENTED_EDGE('',*,*,#13258,.T.);
#18396=ORIENTED_EDGE('',*,*,#13260,.T.);
#18397=ORIENTED_EDGE('',*,*,#13252,.T.);
#18398=ORIENTED_EDGE('',*,*,#13256,.T.);
#18399=ORIENTED_EDGE('',*,*,#13267,.T.);
#18400=ORIENTED_EDGE('',*,*,#13269,.T.);
#18401=ORIENTED_EDGE('',*,*,#13261,.T.);
#18402=ORIENTED_EDGE('',*,*,#13265,.T.);
#18403=ORIENTED_EDGE('',*,*,#13276,.T.);
#18404=ORIENTED_EDGE('',*,*,#13278,.T.);
#18405=ORIENTED_EDGE('',*,*,#13270,.T.);
#18406=ORIENTED_EDGE('',*,*,#13274,.T.);
#18407=ORIENTED_EDGE('',*,*,#13296,.T.);
#18408=ORIENTED_EDGE('',*,*,#13298,.T.);
#18409=ORIENTED_EDGE('',*,*,#13290,.T.);
#18410=ORIENTED_EDGE('',*,*,#13294,.T.);
#18411=ORIENTED_EDGE('',*,*,#13305,.T.);
#18412=ORIENTED_EDGE('',*,*,#13307,.T.);
#18413=ORIENTED_EDGE('',*,*,#13299,.T.);
#18414=ORIENTED_EDGE('',*,*,#13303,.T.);
#18415=ORIENTED_EDGE('',*,*,#13314,.T.);
#18416=ORIENTED_EDGE('',*,*,#13316,.T.);
#18417=ORIENTED_EDGE('',*,*,#13308,.T.);
#18418=ORIENTED_EDGE('',*,*,#13312,.T.);
#18419=ORIENTED_EDGE('',*,*,#13323,.T.);
#18420=ORIENTED_EDGE('',*,*,#13325,.T.);
#18421=ORIENTED_EDGE('',*,*,#13317,.T.);
#18422=ORIENTED_EDGE('',*,*,#13321,.T.);
#18423=ORIENTED_EDGE('',*,*,#13332,.T.);
#18424=ORIENTED_EDGE('',*,*,#13334,.T.);
#18425=ORIENTED_EDGE('',*,*,#13326,.T.);
#18426=ORIENTED_EDGE('',*,*,#13330,.T.);
#18427=ORIENTED_EDGE('',*,*,#13341,.T.);
#18428=ORIENTED_EDGE('',*,*,#13343,.T.);
#18429=ORIENTED_EDGE('',*,*,#13335,.T.);
#18430=ORIENTED_EDGE('',*,*,#13339,.T.);
#18431=ORIENTED_EDGE('',*,*,#13350,.T.);
#18432=ORIENTED_EDGE('',*,*,#13352,.T.);
#18433=ORIENTED_EDGE('',*,*,#13344,.T.);
#18434=ORIENTED_EDGE('',*,*,#13348,.T.);
#18435=ORIENTED_EDGE('',*,*,#13359,.T.);
#18436=ORIENTED_EDGE('',*,*,#13361,.T.);
#18437=ORIENTED_EDGE('',*,*,#13353,.T.);
#18438=ORIENTED_EDGE('',*,*,#13357,.T.);
#18439=ORIENTED_EDGE('',*,*,#13368,.T.);
#18440=ORIENTED_EDGE('',*,*,#13370,.T.);
#18441=ORIENTED_EDGE('',*,*,#13362,.T.);
#18442=ORIENTED_EDGE('',*,*,#13366,.T.);
#18443=ORIENTED_EDGE('',*,*,#13377,.T.);
#18444=ORIENTED_EDGE('',*,*,#13379,.T.);
#18445=ORIENTED_EDGE('',*,*,#13371,.T.);
#18446=ORIENTED_EDGE('',*,*,#13375,.T.);
#18447=ORIENTED_EDGE('',*,*,#13386,.T.);
#18448=ORIENTED_EDGE('',*,*,#13388,.T.);
#18449=ORIENTED_EDGE('',*,*,#13380,.T.);
#18450=ORIENTED_EDGE('',*,*,#13384,.T.);
#18451=ORIENTED_EDGE('',*,*,#13395,.T.);
#18452=ORIENTED_EDGE('',*,*,#13397,.T.);
#18453=ORIENTED_EDGE('',*,*,#13389,.T.);
#18454=ORIENTED_EDGE('',*,*,#13393,.T.);
#18455=ORIENTED_EDGE('',*,*,#13406,.F.);
#18456=ORIENTED_EDGE('',*,*,#13407,.T.);
#18457=ORIENTED_EDGE('',*,*,#13403,.T.);
#18458=ORIENTED_EDGE('',*,*,#13407,.F.);
#18459=ORIENTED_EDGE('',*,*,#13406,.T.);
#18460=ORIENTED_EDGE('',*,*,#13179,.T.);
#18461=ORIENTED_EDGE('',*,*,#13408,.F.);
#18462=ORIENTED_EDGE('',*,*,#13409,.T.);
#18463=ORIENTED_EDGE('',*,*,#13410,.T.);
#18464=ORIENTED_EDGE('',*,*,#13411,.T.);
#18465=ORIENTED_EDGE('',*,*,#13412,.T.);
#18466=ORIENTED_EDGE('',*,*,#13411,.F.);
#18467=ORIENTED_EDGE('',*,*,#13413,.T.);
#18468=ORIENTED_EDGE('',*,*,#13414,.T.);
#18469=ORIENTED_EDGE('',*,*,#13415,.F.);
#18470=ORIENTED_EDGE('',*,*,#13416,.T.);
#18471=ORIENTED_EDGE('',*,*,#13408,.T.);
#18472=ORIENTED_EDGE('',*,*,#13417,.T.);
#18473=ORIENTED_EDGE('',*,*,#13418,.F.);
#18474=ORIENTED_EDGE('',*,*,#13419,.T.);
#18475=ORIENTED_EDGE('',*,*,#13415,.T.);
#18476=ORIENTED_EDGE('',*,*,#13420,.T.);
#18477=ORIENTED_EDGE('',*,*,#13421,.F.);
#18478=ORIENTED_EDGE('',*,*,#13422,.T.);
#18479=ORIENTED_EDGE('',*,*,#13418,.T.);
#18480=ORIENTED_EDGE('',*,*,#13423,.T.);
#18481=ORIENTED_EDGE('',*,*,#13424,.F.);
#18482=ORIENTED_EDGE('',*,*,#13425,.T.);
#18483=ORIENTED_EDGE('',*,*,#13421,.T.);
#18484=ORIENTED_EDGE('',*,*,#13426,.T.);
#18485=ORIENTED_EDGE('',*,*,#13427,.F.);
#18486=ORIENTED_EDGE('',*,*,#13428,.T.);
#18487=ORIENTED_EDGE('',*,*,#13424,.T.);
#18488=ORIENTED_EDGE('',*,*,#13429,.T.);
#18489=ORIENTED_EDGE('',*,*,#13430,.F.);
#18490=ORIENTED_EDGE('',*,*,#13431,.T.);
#18491=ORIENTED_EDGE('',*,*,#13427,.T.);
#18492=ORIENTED_EDGE('',*,*,#13432,.T.);
#18493=ORIENTED_EDGE('',*,*,#13433,.F.);
#18494=ORIENTED_EDGE('',*,*,#13434,.T.);
#18495=ORIENTED_EDGE('',*,*,#13430,.T.);
#18496=ORIENTED_EDGE('',*,*,#13435,.T.);
#18497=ORIENTED_EDGE('',*,*,#13436,.F.);
#18498=ORIENTED_EDGE('',*,*,#13437,.T.);
#18499=ORIENTED_EDGE('',*,*,#13433,.T.);
#18500=ORIENTED_EDGE('',*,*,#13438,.T.);
#18501=ORIENTED_EDGE('',*,*,#13439,.F.);
#18502=ORIENTED_EDGE('',*,*,#13440,.T.);
#18503=ORIENTED_EDGE('',*,*,#13436,.T.);
#18504=ORIENTED_EDGE('',*,*,#13441,.T.);
#18505=ORIENTED_EDGE('',*,*,#13442,.F.);
#18506=ORIENTED_EDGE('',*,*,#13443,.T.);
#18507=ORIENTED_EDGE('',*,*,#13439,.T.);
#18508=ORIENTED_EDGE('',*,*,#13444,.T.);
#18509=ORIENTED_EDGE('',*,*,#13445,.F.);
#18510=ORIENTED_EDGE('',*,*,#13446,.T.);
#18511=ORIENTED_EDGE('',*,*,#13442,.T.);
#18512=ORIENTED_EDGE('',*,*,#13447,.T.);
#18513=ORIENTED_EDGE('',*,*,#13448,.F.);
#18514=ORIENTED_EDGE('',*,*,#13449,.T.);
#18515=ORIENTED_EDGE('',*,*,#13445,.T.);
#18516=ORIENTED_EDGE('',*,*,#13450,.T.);
#18517=ORIENTED_EDGE('',*,*,#13451,.F.);
#18518=ORIENTED_EDGE('',*,*,#13452,.T.);
#18519=ORIENTED_EDGE('',*,*,#13448,.T.);
#18520=ORIENTED_EDGE('',*,*,#13453,.T.);
#18521=ORIENTED_EDGE('',*,*,#13454,.F.);
#18522=ORIENTED_EDGE('',*,*,#13455,.T.);
#18523=ORIENTED_EDGE('',*,*,#13456,.F.);
#18524=ORIENTED_EDGE('',*,*,#13457,.F.);
#18525=ORIENTED_EDGE('',*,*,#13458,.F.);
#18526=ORIENTED_EDGE('',*,*,#13459,.T.);
#18527=ORIENTED_EDGE('',*,*,#13454,.T.);
#18528=ORIENTED_EDGE('',*,*,#13460,.F.);
#18529=ORIENTED_EDGE('',*,*,#13461,.F.);
#18530=ORIENTED_EDGE('',*,*,#13462,.T.);
#18531=ORIENTED_EDGE('',*,*,#13458,.T.);
#18532=ORIENTED_EDGE('',*,*,#13463,.F.);
#18533=ORIENTED_EDGE('',*,*,#13464,.F.);
#18534=ORIENTED_EDGE('',*,*,#13465,.T.);
#18535=ORIENTED_EDGE('',*,*,#13461,.T.);
#18536=ORIENTED_EDGE('',*,*,#13466,.F.);
#18537=ORIENTED_EDGE('',*,*,#13467,.F.);
#18538=ORIENTED_EDGE('',*,*,#13468,.T.);
#18539=ORIENTED_EDGE('',*,*,#13464,.T.);
#18540=ORIENTED_EDGE('',*,*,#13469,.F.);
#18541=ORIENTED_EDGE('',*,*,#13470,.F.);
#18542=ORIENTED_EDGE('',*,*,#13471,.T.);
#18543=ORIENTED_EDGE('',*,*,#13467,.T.);
#18544=ORIENTED_EDGE('',*,*,#13472,.F.);
#18545=ORIENTED_EDGE('',*,*,#13473,.F.);
#18546=ORIENTED_EDGE('',*,*,#13474,.T.);
#18547=ORIENTED_EDGE('',*,*,#13470,.T.);
#18548=ORIENTED_EDGE('',*,*,#13475,.F.);
#18549=ORIENTED_EDGE('',*,*,#13476,.F.);
#18550=ORIENTED_EDGE('',*,*,#13477,.T.);
#18551=ORIENTED_EDGE('',*,*,#13473,.T.);
#18552=ORIENTED_EDGE('',*,*,#13478,.F.);
#18553=ORIENTED_EDGE('',*,*,#13479,.F.);
#18554=ORIENTED_EDGE('',*,*,#13480,.T.);
#18555=ORIENTED_EDGE('',*,*,#13476,.T.);
#18556=ORIENTED_EDGE('',*,*,#13481,.F.);
#18557=ORIENTED_EDGE('',*,*,#13482,.F.);
#18558=ORIENTED_EDGE('',*,*,#13483,.T.);
#18559=ORIENTED_EDGE('',*,*,#13479,.T.);
#18560=ORIENTED_EDGE('',*,*,#13484,.F.);
#18561=ORIENTED_EDGE('',*,*,#13485,.F.);
#18562=ORIENTED_EDGE('',*,*,#13486,.T.);
#18563=ORIENTED_EDGE('',*,*,#13482,.T.);
#18564=ORIENTED_EDGE('',*,*,#13487,.F.);
#18565=ORIENTED_EDGE('',*,*,#13488,.F.);
#18566=ORIENTED_EDGE('',*,*,#13489,.T.);
#18567=ORIENTED_EDGE('',*,*,#13485,.T.);
#18568=ORIENTED_EDGE('',*,*,#13490,.F.);
#18569=ORIENTED_EDGE('',*,*,#13491,.F.);
#18570=ORIENTED_EDGE('',*,*,#13492,.T.);
#18571=ORIENTED_EDGE('',*,*,#13488,.T.);
#18572=ORIENTED_EDGE('',*,*,#13493,.F.);
#18573=ORIENTED_EDGE('',*,*,#13494,.F.);
#18574=ORIENTED_EDGE('',*,*,#13495,.T.);
#18575=ORIENTED_EDGE('',*,*,#13491,.T.);
#18576=ORIENTED_EDGE('',*,*,#13496,.F.);
#18577=ORIENTED_EDGE('',*,*,#13497,.F.);
#18578=ORIENTED_EDGE('',*,*,#13498,.T.);
#18579=ORIENTED_EDGE('',*,*,#13494,.T.);
#18580=ORIENTED_EDGE('',*,*,#13499,.F.);
#18581=ORIENTED_EDGE('',*,*,#13456,.T.);
#18582=ORIENTED_EDGE('',*,*,#13500,.T.);
#18583=ORIENTED_EDGE('',*,*,#13501,.F.);
#18584=ORIENTED_EDGE('',*,*,#13502,.F.);
#18585=ORIENTED_EDGE('',*,*,#13503,.T.);
#18586=ORIENTED_EDGE('',*,*,#13503,.F.);
#18587=ORIENTED_EDGE('',*,*,#13504,.F.);
#18588=ORIENTED_EDGE('',*,*,#13453,.F.);
#18589=ORIENTED_EDGE('',*,*,#13450,.F.);
#18590=ORIENTED_EDGE('',*,*,#13447,.F.);
#18591=ORIENTED_EDGE('',*,*,#13444,.F.);
#18592=ORIENTED_EDGE('',*,*,#13441,.F.);
#18593=ORIENTED_EDGE('',*,*,#13438,.F.);
#18594=ORIENTED_EDGE('',*,*,#13435,.F.);
#18595=ORIENTED_EDGE('',*,*,#13432,.F.);
#18596=ORIENTED_EDGE('',*,*,#13429,.F.);
#18597=ORIENTED_EDGE('',*,*,#13426,.F.);
#18598=ORIENTED_EDGE('',*,*,#13423,.F.);
#18599=ORIENTED_EDGE('',*,*,#13420,.F.);
#18600=ORIENTED_EDGE('',*,*,#13417,.F.);
#18601=ORIENTED_EDGE('',*,*,#13414,.F.);
#18602=ORIENTED_EDGE('',*,*,#13505,.F.);
#18603=ORIENTED_EDGE('',*,*,#13506,.T.);
#18604=ORIENTED_EDGE('',*,*,#13499,.T.);
#18605=ORIENTED_EDGE('',*,*,#13496,.T.);
#18606=ORIENTED_EDGE('',*,*,#13493,.T.);
#18607=ORIENTED_EDGE('',*,*,#13490,.T.);
#18608=ORIENTED_EDGE('',*,*,#13487,.T.);
#18609=ORIENTED_EDGE('',*,*,#13484,.T.);
#18610=ORIENTED_EDGE('',*,*,#13481,.T.);
#18611=ORIENTED_EDGE('',*,*,#13478,.T.);
#18612=ORIENTED_EDGE('',*,*,#13475,.T.);
#18613=ORIENTED_EDGE('',*,*,#13472,.T.);
#18614=ORIENTED_EDGE('',*,*,#13469,.T.);
#18615=ORIENTED_EDGE('',*,*,#13466,.T.);
#18616=ORIENTED_EDGE('',*,*,#13463,.T.);
#18617=ORIENTED_EDGE('',*,*,#13460,.T.);
#18618=ORIENTED_EDGE('',*,*,#13457,.T.);
#18619=ORIENTED_EDGE('',*,*,#13410,.F.);
#18620=ORIENTED_EDGE('',*,*,#13507,.T.);
#18621=ORIENTED_EDGE('',*,*,#13508,.T.);
#18622=ORIENTED_EDGE('',*,*,#13505,.T.);
#18623=ORIENTED_EDGE('',*,*,#13413,.F.);
#18624=ORIENTED_EDGE('',*,*,#13497,.T.);
#18625=ORIENTED_EDGE('',*,*,#13506,.F.);
#18626=ORIENTED_EDGE('',*,*,#13508,.F.);
#18627=ORIENTED_EDGE('',*,*,#13509,.T.);
#18628=ORIENTED_EDGE('',*,*,#13500,.F.);
#18629=ORIENTED_EDGE('',*,*,#13455,.F.);
#18630=ORIENTED_EDGE('',*,*,#13459,.F.);
#18631=ORIENTED_EDGE('',*,*,#13462,.F.);
#18632=ORIENTED_EDGE('',*,*,#13465,.F.);
#18633=ORIENTED_EDGE('',*,*,#13468,.F.);
#18634=ORIENTED_EDGE('',*,*,#13471,.F.);
#18635=ORIENTED_EDGE('',*,*,#13474,.F.);
#18636=ORIENTED_EDGE('',*,*,#13477,.F.);
#18637=ORIENTED_EDGE('',*,*,#13480,.F.);
#18638=ORIENTED_EDGE('',*,*,#13483,.F.);
#18639=ORIENTED_EDGE('',*,*,#13486,.F.);
#18640=ORIENTED_EDGE('',*,*,#13489,.F.);
#18641=ORIENTED_EDGE('',*,*,#13492,.F.);
#18642=ORIENTED_EDGE('',*,*,#13495,.F.);
#18643=ORIENTED_EDGE('',*,*,#13498,.F.);
#18644=ORIENTED_EDGE('',*,*,#13509,.F.);
#18645=ORIENTED_EDGE('',*,*,#13507,.F.);
#18646=ORIENTED_EDGE('',*,*,#13409,.F.);
#18647=ORIENTED_EDGE('',*,*,#13416,.F.);
#18648=ORIENTED_EDGE('',*,*,#13419,.F.);
#18649=ORIENTED_EDGE('',*,*,#13422,.F.);
#18650=ORIENTED_EDGE('',*,*,#13425,.F.);
#18651=ORIENTED_EDGE('',*,*,#13428,.F.);
#18652=ORIENTED_EDGE('',*,*,#13431,.F.);
#18653=ORIENTED_EDGE('',*,*,#13434,.F.);
#18654=ORIENTED_EDGE('',*,*,#13437,.F.);
#18655=ORIENTED_EDGE('',*,*,#13440,.F.);
#18656=ORIENTED_EDGE('',*,*,#13443,.F.);
#18657=ORIENTED_EDGE('',*,*,#13446,.F.);
#18658=ORIENTED_EDGE('',*,*,#13449,.F.);
#18659=ORIENTED_EDGE('',*,*,#13452,.F.);
#18660=ORIENTED_EDGE('',*,*,#13510,.F.);
#18661=ORIENTED_EDGE('',*,*,#13511,.F.);
#18662=ORIENTED_EDGE('',*,*,#13512,.T.);
#18663=ORIENTED_EDGE('',*,*,#13513,.T.);
#18664=ORIENTED_EDGE('',*,*,#13514,.F.);
#18665=ORIENTED_EDGE('',*,*,#13513,.F.);
#18666=ORIENTED_EDGE('',*,*,#13515,.T.);
#18667=ORIENTED_EDGE('',*,*,#13516,.F.);
#18668=ORIENTED_EDGE('',*,*,#13517,.F.);
#18669=ORIENTED_EDGE('',*,*,#13518,.F.);
#18670=ORIENTED_EDGE('',*,*,#13515,.F.);
#18671=ORIENTED_EDGE('',*,*,#13512,.F.);
#18672=ORIENTED_EDGE('',*,*,#13519,.F.);
#18673=ORIENTED_EDGE('',*,*,#13520,.T.);
#18674=ORIENTED_EDGE('',*,*,#13521,.T.);
#18675=ORIENTED_EDGE('',*,*,#13522,.F.);
#18676=ORIENTED_EDGE('',*,*,#13521,.F.);
#18677=ORIENTED_EDGE('',*,*,#13523,.T.);
#18678=ORIENTED_EDGE('',*,*,#13524,.F.);
#18679=ORIENTED_EDGE('',*,*,#13525,.F.);
#18680=ORIENTED_EDGE('',*,*,#13526,.F.);
#18681=ORIENTED_EDGE('',*,*,#13523,.F.);
#18682=ORIENTED_EDGE('',*,*,#13520,.F.);
#18683=ORIENTED_EDGE('',*,*,#13527,.F.);
#18684=ORIENTED_EDGE('',*,*,#13528,.T.);
#18685=ORIENTED_EDGE('',*,*,#13529,.T.);
#18686=ORIENTED_EDGE('',*,*,#13530,.F.);
#18687=ORIENTED_EDGE('',*,*,#13529,.F.);
#18688=ORIENTED_EDGE('',*,*,#13531,.T.);
#18689=ORIENTED_EDGE('',*,*,#13532,.F.);
#18690=ORIENTED_EDGE('',*,*,#13533,.F.);
#18691=ORIENTED_EDGE('',*,*,#13534,.F.);
#18692=ORIENTED_EDGE('',*,*,#13531,.F.);
#18693=ORIENTED_EDGE('',*,*,#13528,.F.);
#18694=ORIENTED_EDGE('',*,*,#13535,.F.);
#18695=ORIENTED_EDGE('',*,*,#13536,.T.);
#18696=ORIENTED_EDGE('',*,*,#13537,.T.);
#18697=ORIENTED_EDGE('',*,*,#13538,.F.);
#18698=ORIENTED_EDGE('',*,*,#13537,.F.);
#18699=ORIENTED_EDGE('',*,*,#13539,.T.);
#18700=ORIENTED_EDGE('',*,*,#13540,.F.);
#18701=ORIENTED_EDGE('',*,*,#13541,.F.);
#18702=ORIENTED_EDGE('',*,*,#13542,.F.);
#18703=ORIENTED_EDGE('',*,*,#13539,.F.);
#18704=ORIENTED_EDGE('',*,*,#13536,.F.);
#18705=ORIENTED_EDGE('',*,*,#13543,.F.);
#18706=ORIENTED_EDGE('',*,*,#13544,.T.);
#18707=ORIENTED_EDGE('',*,*,#13545,.T.);
#18708=ORIENTED_EDGE('',*,*,#13546,.F.);
#18709=ORIENTED_EDGE('',*,*,#13545,.F.);
#18710=ORIENTED_EDGE('',*,*,#13547,.T.);
#18711=ORIENTED_EDGE('',*,*,#13548,.F.);
#18712=ORIENTED_EDGE('',*,*,#13549,.F.);
#18713=ORIENTED_EDGE('',*,*,#13550,.F.);
#18714=ORIENTED_EDGE('',*,*,#13547,.F.);
#18715=ORIENTED_EDGE('',*,*,#13544,.F.);
#18716=ORIENTED_EDGE('',*,*,#13551,.F.);
#18717=ORIENTED_EDGE('',*,*,#13552,.T.);
#18718=ORIENTED_EDGE('',*,*,#13553,.T.);
#18719=ORIENTED_EDGE('',*,*,#13554,.F.);
#18720=ORIENTED_EDGE('',*,*,#13553,.F.);
#18721=ORIENTED_EDGE('',*,*,#13555,.T.);
#18722=ORIENTED_EDGE('',*,*,#13556,.F.);
#18723=ORIENTED_EDGE('',*,*,#13557,.F.);
#18724=ORIENTED_EDGE('',*,*,#13558,.F.);
#18725=ORIENTED_EDGE('',*,*,#13555,.F.);
#18726=ORIENTED_EDGE('',*,*,#13552,.F.);
#18727=ORIENTED_EDGE('',*,*,#13559,.F.);
#18728=ORIENTED_EDGE('',*,*,#13560,.T.);
#18729=ORIENTED_EDGE('',*,*,#13561,.T.);
#18730=ORIENTED_EDGE('',*,*,#13562,.F.);
#18731=ORIENTED_EDGE('',*,*,#13561,.F.);
#18732=ORIENTED_EDGE('',*,*,#13563,.T.);
#18733=ORIENTED_EDGE('',*,*,#13564,.F.);
#18734=ORIENTED_EDGE('',*,*,#13565,.F.);
#18735=ORIENTED_EDGE('',*,*,#13566,.F.);
#18736=ORIENTED_EDGE('',*,*,#13563,.F.);
#18737=ORIENTED_EDGE('',*,*,#13560,.F.);
#18738=ORIENTED_EDGE('',*,*,#13567,.F.);
#18739=ORIENTED_EDGE('',*,*,#13568,.T.);
#18740=ORIENTED_EDGE('',*,*,#13569,.T.);
#18741=ORIENTED_EDGE('',*,*,#13570,.F.);
#18742=ORIENTED_EDGE('',*,*,#13569,.F.);
#18743=ORIENTED_EDGE('',*,*,#13571,.T.);
#18744=ORIENTED_EDGE('',*,*,#13572,.F.);
#18745=ORIENTED_EDGE('',*,*,#13573,.F.);
#18746=ORIENTED_EDGE('',*,*,#13574,.F.);
#18747=ORIENTED_EDGE('',*,*,#13571,.F.);
#18748=ORIENTED_EDGE('',*,*,#13568,.F.);
#18749=ORIENTED_EDGE('',*,*,#13575,.F.);
#18750=ORIENTED_EDGE('',*,*,#13576,.T.);
#18751=ORIENTED_EDGE('',*,*,#13577,.T.);
#18752=ORIENTED_EDGE('',*,*,#13578,.F.);
#18753=ORIENTED_EDGE('',*,*,#13577,.F.);
#18754=ORIENTED_EDGE('',*,*,#13579,.T.);
#18755=ORIENTED_EDGE('',*,*,#13580,.F.);
#18756=ORIENTED_EDGE('',*,*,#13581,.F.);
#18757=ORIENTED_EDGE('',*,*,#13582,.F.);
#18758=ORIENTED_EDGE('',*,*,#13579,.F.);
#18759=ORIENTED_EDGE('',*,*,#13576,.F.);
#18760=ORIENTED_EDGE('',*,*,#13583,.F.);
#18761=ORIENTED_EDGE('',*,*,#13584,.T.);
#18762=ORIENTED_EDGE('',*,*,#13585,.T.);
#18763=ORIENTED_EDGE('',*,*,#13586,.F.);
#18764=ORIENTED_EDGE('',*,*,#13585,.F.);
#18765=ORIENTED_EDGE('',*,*,#13587,.T.);
#18766=ORIENTED_EDGE('',*,*,#13588,.F.);
#18767=ORIENTED_EDGE('',*,*,#13589,.F.);
#18768=ORIENTED_EDGE('',*,*,#13590,.F.);
#18769=ORIENTED_EDGE('',*,*,#13587,.F.);
#18770=ORIENTED_EDGE('',*,*,#13584,.F.);
#18771=ORIENTED_EDGE('',*,*,#13591,.F.);
#18772=ORIENTED_EDGE('',*,*,#13592,.T.);
#18773=ORIENTED_EDGE('',*,*,#13593,.T.);
#18774=ORIENTED_EDGE('',*,*,#13594,.F.);
#18775=ORIENTED_EDGE('',*,*,#13593,.F.);
#18776=ORIENTED_EDGE('',*,*,#13595,.T.);
#18777=ORIENTED_EDGE('',*,*,#13596,.F.);
#18778=ORIENTED_EDGE('',*,*,#13597,.F.);
#18779=ORIENTED_EDGE('',*,*,#13598,.F.);
#18780=ORIENTED_EDGE('',*,*,#13595,.F.);
#18781=ORIENTED_EDGE('',*,*,#13592,.F.);
#18782=ORIENTED_EDGE('',*,*,#13599,.F.);
#18783=ORIENTED_EDGE('',*,*,#13600,.T.);
#18784=ORIENTED_EDGE('',*,*,#13601,.T.);
#18785=ORIENTED_EDGE('',*,*,#13602,.F.);
#18786=ORIENTED_EDGE('',*,*,#13601,.F.);
#18787=ORIENTED_EDGE('',*,*,#13603,.T.);
#18788=ORIENTED_EDGE('',*,*,#13604,.F.);
#18789=ORIENTED_EDGE('',*,*,#13605,.F.);
#18790=ORIENTED_EDGE('',*,*,#13606,.F.);
#18791=ORIENTED_EDGE('',*,*,#13603,.F.);
#18792=ORIENTED_EDGE('',*,*,#13600,.F.);
#18793=ORIENTED_EDGE('',*,*,#13607,.F.);
#18794=ORIENTED_EDGE('',*,*,#13608,.T.);
#18795=ORIENTED_EDGE('',*,*,#13609,.T.);
#18796=ORIENTED_EDGE('',*,*,#13610,.F.);
#18797=ORIENTED_EDGE('',*,*,#13609,.F.);
#18798=ORIENTED_EDGE('',*,*,#13611,.T.);
#18799=ORIENTED_EDGE('',*,*,#13612,.F.);
#18800=ORIENTED_EDGE('',*,*,#13613,.F.);
#18801=ORIENTED_EDGE('',*,*,#13614,.F.);
#18802=ORIENTED_EDGE('',*,*,#13611,.F.);
#18803=ORIENTED_EDGE('',*,*,#13608,.F.);
#18804=ORIENTED_EDGE('',*,*,#13615,.F.);
#18805=ORIENTED_EDGE('',*,*,#13616,.T.);
#18806=ORIENTED_EDGE('',*,*,#13617,.T.);
#18807=ORIENTED_EDGE('',*,*,#13618,.F.);
#18808=ORIENTED_EDGE('',*,*,#13617,.F.);
#18809=ORIENTED_EDGE('',*,*,#13619,.T.);
#18810=ORIENTED_EDGE('',*,*,#13620,.F.);
#18811=ORIENTED_EDGE('',*,*,#13621,.F.);
#18812=ORIENTED_EDGE('',*,*,#13622,.F.);
#18813=ORIENTED_EDGE('',*,*,#13619,.F.);
#18814=ORIENTED_EDGE('',*,*,#13616,.F.);
#18815=ORIENTED_EDGE('',*,*,#13623,.F.);
#18816=ORIENTED_EDGE('',*,*,#13624,.T.);
#18817=ORIENTED_EDGE('',*,*,#13625,.T.);
#18818=ORIENTED_EDGE('',*,*,#13626,.F.);
#18819=ORIENTED_EDGE('',*,*,#13625,.F.);
#18820=ORIENTED_EDGE('',*,*,#13627,.T.);
#18821=ORIENTED_EDGE('',*,*,#13628,.F.);
#18822=ORIENTED_EDGE('',*,*,#13629,.F.);
#18823=ORIENTED_EDGE('',*,*,#13630,.F.);
#18824=ORIENTED_EDGE('',*,*,#13627,.F.);
#18825=ORIENTED_EDGE('',*,*,#13624,.F.);
#18826=ORIENTED_EDGE('',*,*,#13631,.F.);
#18827=ORIENTED_EDGE('',*,*,#13632,.T.);
#18828=ORIENTED_EDGE('',*,*,#13633,.T.);
#18829=ORIENTED_EDGE('',*,*,#13634,.F.);
#18830=ORIENTED_EDGE('',*,*,#13633,.F.);
#18831=ORIENTED_EDGE('',*,*,#13635,.T.);
#18832=ORIENTED_EDGE('',*,*,#13636,.F.);
#18833=ORIENTED_EDGE('',*,*,#13637,.F.);
#18834=ORIENTED_EDGE('',*,*,#13638,.F.);
#18835=ORIENTED_EDGE('',*,*,#13635,.F.);
#18836=ORIENTED_EDGE('',*,*,#13632,.F.);
#18837=ORIENTED_EDGE('',*,*,#13639,.F.);
#18838=ORIENTED_EDGE('',*,*,#13640,.T.);
#18839=ORIENTED_EDGE('',*,*,#13641,.T.);
#18840=ORIENTED_EDGE('',*,*,#13642,.F.);
#18841=ORIENTED_EDGE('',*,*,#13641,.F.);
#18842=ORIENTED_EDGE('',*,*,#13643,.T.);
#18843=ORIENTED_EDGE('',*,*,#13644,.F.);
#18844=ORIENTED_EDGE('',*,*,#13645,.F.);
#18845=ORIENTED_EDGE('',*,*,#13646,.F.);
#18846=ORIENTED_EDGE('',*,*,#13643,.F.);
#18847=ORIENTED_EDGE('',*,*,#13640,.F.);
#18848=ORIENTED_EDGE('',*,*,#13647,.F.);
#18849=ORIENTED_EDGE('',*,*,#13648,.T.);
#18850=ORIENTED_EDGE('',*,*,#13649,.T.);
#18851=ORIENTED_EDGE('',*,*,#13650,.F.);
#18852=ORIENTED_EDGE('',*,*,#13651,.F.);
#18853=ORIENTED_EDGE('',*,*,#13649,.F.);
#18854=ORIENTED_EDGE('',*,*,#13652,.T.);
#18855=ORIENTED_EDGE('',*,*,#13653,.F.);
#18856=ORIENTED_EDGE('',*,*,#13654,.F.);
#18857=ORIENTED_EDGE('',*,*,#13655,.F.);
#18858=ORIENTED_EDGE('',*,*,#13652,.F.);
#18859=ORIENTED_EDGE('',*,*,#13648,.F.);
#18860=ORIENTED_EDGE('',*,*,#13656,.F.);
#18861=ORIENTED_EDGE('',*,*,#13657,.T.);
#18862=ORIENTED_EDGE('',*,*,#13658,.T.);
#18863=ORIENTED_EDGE('',*,*,#13659,.F.);
#18864=ORIENTED_EDGE('',*,*,#13658,.F.);
#18865=ORIENTED_EDGE('',*,*,#13660,.T.);
#18866=ORIENTED_EDGE('',*,*,#13661,.F.);
#18867=ORIENTED_EDGE('',*,*,#13662,.F.);
#18868=ORIENTED_EDGE('',*,*,#13663,.F.);
#18869=ORIENTED_EDGE('',*,*,#13660,.F.);
#18870=ORIENTED_EDGE('',*,*,#13657,.F.);
#18871=ORIENTED_EDGE('',*,*,#13664,.F.);
#18872=ORIENTED_EDGE('',*,*,#13665,.T.);
#18873=ORIENTED_EDGE('',*,*,#13666,.T.);
#18874=ORIENTED_EDGE('',*,*,#13667,.F.);
#18875=ORIENTED_EDGE('',*,*,#13666,.F.);
#18876=ORIENTED_EDGE('',*,*,#13668,.T.);
#18877=ORIENTED_EDGE('',*,*,#13669,.F.);
#18878=ORIENTED_EDGE('',*,*,#13670,.F.);
#18879=ORIENTED_EDGE('',*,*,#13671,.F.);
#18880=ORIENTED_EDGE('',*,*,#13668,.F.);
#18881=ORIENTED_EDGE('',*,*,#13665,.F.);
#18882=ORIENTED_EDGE('',*,*,#13672,.F.);
#18883=ORIENTED_EDGE('',*,*,#13673,.T.);
#18884=ORIENTED_EDGE('',*,*,#13674,.T.);
#18885=ORIENTED_EDGE('',*,*,#13675,.F.);
#18886=ORIENTED_EDGE('',*,*,#13674,.F.);
#18887=ORIENTED_EDGE('',*,*,#13676,.T.);
#18888=ORIENTED_EDGE('',*,*,#13677,.F.);
#18889=ORIENTED_EDGE('',*,*,#13678,.F.);
#18890=ORIENTED_EDGE('',*,*,#13679,.F.);
#18891=ORIENTED_EDGE('',*,*,#13676,.F.);
#18892=ORIENTED_EDGE('',*,*,#13673,.F.);
#18893=ORIENTED_EDGE('',*,*,#13680,.F.);
#18894=ORIENTED_EDGE('',*,*,#13681,.T.);
#18895=ORIENTED_EDGE('',*,*,#13682,.T.);
#18896=ORIENTED_EDGE('',*,*,#13683,.F.);
#18897=ORIENTED_EDGE('',*,*,#13682,.F.);
#18898=ORIENTED_EDGE('',*,*,#13684,.T.);
#18899=ORIENTED_EDGE('',*,*,#13685,.F.);
#18900=ORIENTED_EDGE('',*,*,#13686,.F.);
#18901=ORIENTED_EDGE('',*,*,#13687,.F.);
#18902=ORIENTED_EDGE('',*,*,#13684,.F.);
#18903=ORIENTED_EDGE('',*,*,#13681,.F.);
#18904=ORIENTED_EDGE('',*,*,#13688,.F.);
#18905=ORIENTED_EDGE('',*,*,#13689,.T.);
#18906=ORIENTED_EDGE('',*,*,#13690,.T.);
#18907=ORIENTED_EDGE('',*,*,#13691,.F.);
#18908=ORIENTED_EDGE('',*,*,#13690,.F.);
#18909=ORIENTED_EDGE('',*,*,#13692,.T.);
#18910=ORIENTED_EDGE('',*,*,#13693,.F.);
#18911=ORIENTED_EDGE('',*,*,#13694,.F.);
#18912=ORIENTED_EDGE('',*,*,#13695,.F.);
#18913=ORIENTED_EDGE('',*,*,#13692,.F.);
#18914=ORIENTED_EDGE('',*,*,#13689,.F.);
#18915=ORIENTED_EDGE('',*,*,#13696,.F.);
#18916=ORIENTED_EDGE('',*,*,#13697,.T.);
#18917=ORIENTED_EDGE('',*,*,#13698,.T.);
#18918=ORIENTED_EDGE('',*,*,#13699,.F.);
#18919=ORIENTED_EDGE('',*,*,#13698,.F.);
#18920=ORIENTED_EDGE('',*,*,#13700,.T.);
#18921=ORIENTED_EDGE('',*,*,#13701,.F.);
#18922=ORIENTED_EDGE('',*,*,#13702,.F.);
#18923=ORIENTED_EDGE('',*,*,#13703,.F.);
#18924=ORIENTED_EDGE('',*,*,#13700,.F.);
#18925=ORIENTED_EDGE('',*,*,#13697,.F.);
#18926=ORIENTED_EDGE('',*,*,#13704,.F.);
#18927=ORIENTED_EDGE('',*,*,#13705,.T.);
#18928=ORIENTED_EDGE('',*,*,#13706,.T.);
#18929=ORIENTED_EDGE('',*,*,#13707,.F.);
#18930=ORIENTED_EDGE('',*,*,#13706,.F.);
#18931=ORIENTED_EDGE('',*,*,#13708,.T.);
#18932=ORIENTED_EDGE('',*,*,#13709,.F.);
#18933=ORIENTED_EDGE('',*,*,#13710,.F.);
#18934=ORIENTED_EDGE('',*,*,#13711,.F.);
#18935=ORIENTED_EDGE('',*,*,#13708,.F.);
#18936=ORIENTED_EDGE('',*,*,#13705,.F.);
#18937=ORIENTED_EDGE('',*,*,#13712,.F.);
#18938=ORIENTED_EDGE('',*,*,#13713,.T.);
#18939=ORIENTED_EDGE('',*,*,#13714,.T.);
#18940=ORIENTED_EDGE('',*,*,#13715,.F.);
#18941=ORIENTED_EDGE('',*,*,#13714,.F.);
#18942=ORIENTED_EDGE('',*,*,#13716,.T.);
#18943=ORIENTED_EDGE('',*,*,#13717,.F.);
#18944=ORIENTED_EDGE('',*,*,#13718,.F.);
#18945=ORIENTED_EDGE('',*,*,#13719,.F.);
#18946=ORIENTED_EDGE('',*,*,#13716,.F.);
#18947=ORIENTED_EDGE('',*,*,#13713,.F.);
#18948=ORIENTED_EDGE('',*,*,#13720,.F.);
#18949=ORIENTED_EDGE('',*,*,#13721,.T.);
#18950=ORIENTED_EDGE('',*,*,#13722,.T.);
#18951=ORIENTED_EDGE('',*,*,#13723,.F.);
#18952=ORIENTED_EDGE('',*,*,#13722,.F.);
#18953=ORIENTED_EDGE('',*,*,#13724,.T.);
#18954=ORIENTED_EDGE('',*,*,#13725,.F.);
#18955=ORIENTED_EDGE('',*,*,#13726,.F.);
#18956=ORIENTED_EDGE('',*,*,#13727,.F.);
#18957=ORIENTED_EDGE('',*,*,#13724,.F.);
#18958=ORIENTED_EDGE('',*,*,#13721,.F.);
#18959=ORIENTED_EDGE('',*,*,#13728,.F.);
#18960=ORIENTED_EDGE('',*,*,#13729,.T.);
#18961=ORIENTED_EDGE('',*,*,#13730,.T.);
#18962=ORIENTED_EDGE('',*,*,#13731,.F.);
#18963=ORIENTED_EDGE('',*,*,#13730,.F.);
#18964=ORIENTED_EDGE('',*,*,#13732,.T.);
#18965=ORIENTED_EDGE('',*,*,#13733,.F.);
#18966=ORIENTED_EDGE('',*,*,#13734,.F.);
#18967=ORIENTED_EDGE('',*,*,#13735,.F.);
#18968=ORIENTED_EDGE('',*,*,#13732,.F.);
#18969=ORIENTED_EDGE('',*,*,#13729,.F.);
#18970=ORIENTED_EDGE('',*,*,#13736,.F.);
#18971=ORIENTED_EDGE('',*,*,#13737,.T.);
#18972=ORIENTED_EDGE('',*,*,#13738,.T.);
#18973=ORIENTED_EDGE('',*,*,#13739,.F.);
#18974=ORIENTED_EDGE('',*,*,#13738,.F.);
#18975=ORIENTED_EDGE('',*,*,#13740,.T.);
#18976=ORIENTED_EDGE('',*,*,#13741,.F.);
#18977=ORIENTED_EDGE('',*,*,#13742,.F.);
#18978=ORIENTED_EDGE('',*,*,#13743,.F.);
#18979=ORIENTED_EDGE('',*,*,#13740,.F.);
#18980=ORIENTED_EDGE('',*,*,#13737,.F.);
#18981=ORIENTED_EDGE('',*,*,#13744,.F.);
#18982=ORIENTED_EDGE('',*,*,#13745,.T.);
#18983=ORIENTED_EDGE('',*,*,#13746,.T.);
#18984=ORIENTED_EDGE('',*,*,#13747,.F.);
#18985=ORIENTED_EDGE('',*,*,#13746,.F.);
#18986=ORIENTED_EDGE('',*,*,#13748,.T.);
#18987=ORIENTED_EDGE('',*,*,#13749,.F.);
#18988=ORIENTED_EDGE('',*,*,#13750,.F.);
#18989=ORIENTED_EDGE('',*,*,#13751,.F.);
#18990=ORIENTED_EDGE('',*,*,#13748,.F.);
#18991=ORIENTED_EDGE('',*,*,#13745,.F.);
#18992=ORIENTED_EDGE('',*,*,#13752,.F.);
#18993=ORIENTED_EDGE('',*,*,#13753,.T.);
#18994=ORIENTED_EDGE('',*,*,#13754,.T.);
#18995=ORIENTED_EDGE('',*,*,#13755,.F.);
#18996=ORIENTED_EDGE('',*,*,#13754,.F.);
#18997=ORIENTED_EDGE('',*,*,#13756,.T.);
#18998=ORIENTED_EDGE('',*,*,#13757,.F.);
#18999=ORIENTED_EDGE('',*,*,#13758,.F.);
#19000=ORIENTED_EDGE('',*,*,#13759,.F.);
#19001=ORIENTED_EDGE('',*,*,#13756,.F.);
#19002=ORIENTED_EDGE('',*,*,#13753,.F.);
#19003=ORIENTED_EDGE('',*,*,#13760,.F.);
#19004=ORIENTED_EDGE('',*,*,#13761,.T.);
#19005=ORIENTED_EDGE('',*,*,#13762,.T.);
#19006=ORIENTED_EDGE('',*,*,#13763,.F.);
#19007=ORIENTED_EDGE('',*,*,#13762,.F.);
#19008=ORIENTED_EDGE('',*,*,#13764,.T.);
#19009=ORIENTED_EDGE('',*,*,#13765,.F.);
#19010=ORIENTED_EDGE('',*,*,#13766,.F.);
#19011=ORIENTED_EDGE('',*,*,#13767,.F.);
#19012=ORIENTED_EDGE('',*,*,#13764,.F.);
#19013=ORIENTED_EDGE('',*,*,#13761,.F.);
#19014=ORIENTED_EDGE('',*,*,#13768,.F.);
#19015=ORIENTED_EDGE('',*,*,#13769,.T.);
#19016=ORIENTED_EDGE('',*,*,#13770,.T.);
#19017=ORIENTED_EDGE('',*,*,#13771,.F.);
#19018=ORIENTED_EDGE('',*,*,#13770,.F.);
#19019=ORIENTED_EDGE('',*,*,#13772,.T.);
#19020=ORIENTED_EDGE('',*,*,#13773,.F.);
#19021=ORIENTED_EDGE('',*,*,#13774,.F.);
#19022=ORIENTED_EDGE('',*,*,#13775,.F.);
#19023=ORIENTED_EDGE('',*,*,#13772,.F.);
#19024=ORIENTED_EDGE('',*,*,#13769,.F.);
#19025=ORIENTED_EDGE('',*,*,#13776,.F.);
#19026=ORIENTED_EDGE('',*,*,#13777,.T.);
#19027=ORIENTED_EDGE('',*,*,#13778,.T.);
#19028=ORIENTED_EDGE('',*,*,#13779,.F.);
#19029=ORIENTED_EDGE('',*,*,#13778,.F.);
#19030=ORIENTED_EDGE('',*,*,#13780,.T.);
#19031=ORIENTED_EDGE('',*,*,#13781,.F.);
#19032=ORIENTED_EDGE('',*,*,#13782,.F.);
#19033=ORIENTED_EDGE('',*,*,#13783,.F.);
#19034=ORIENTED_EDGE('',*,*,#13780,.F.);
#19035=ORIENTED_EDGE('',*,*,#13777,.F.);
#19036=ORIENTED_EDGE('',*,*,#13784,.F.);
#19037=ORIENTED_EDGE('',*,*,#13785,.T.);
#19038=ORIENTED_EDGE('',*,*,#13786,.T.);
#19039=ORIENTED_EDGE('',*,*,#13787,.F.);
#19040=ORIENTED_EDGE('',*,*,#13786,.F.);
#19041=ORIENTED_EDGE('',*,*,#13788,.T.);
#19042=ORIENTED_EDGE('',*,*,#13789,.F.);
#19043=ORIENTED_EDGE('',*,*,#13790,.F.);
#19044=ORIENTED_EDGE('',*,*,#13791,.F.);
#19045=ORIENTED_EDGE('',*,*,#13788,.F.);
#19046=ORIENTED_EDGE('',*,*,#13785,.F.);
#19047=ORIENTED_EDGE('',*,*,#13517,.T.);
#19048=ORIENTED_EDGE('',*,*,#13511,.T.);
#19049=ORIENTED_EDGE('',*,*,#13514,.T.);
#19050=ORIENTED_EDGE('',*,*,#13792,.F.);
#19051=ORIENTED_EDGE('',*,*,#13525,.T.);
#19052=ORIENTED_EDGE('',*,*,#13519,.T.);
#19053=ORIENTED_EDGE('',*,*,#13522,.T.);
#19054=ORIENTED_EDGE('',*,*,#13793,.F.);
#19055=ORIENTED_EDGE('',*,*,#13533,.T.);
#19056=ORIENTED_EDGE('',*,*,#13527,.T.);
#19057=ORIENTED_EDGE('',*,*,#13530,.T.);
#19058=ORIENTED_EDGE('',*,*,#13794,.F.);
#19059=ORIENTED_EDGE('',*,*,#13541,.T.);
#19060=ORIENTED_EDGE('',*,*,#13535,.T.);
#19061=ORIENTED_EDGE('',*,*,#13538,.T.);
#19062=ORIENTED_EDGE('',*,*,#13795,.F.);
#19063=ORIENTED_EDGE('',*,*,#13549,.T.);
#19064=ORIENTED_EDGE('',*,*,#13543,.T.);
#19065=ORIENTED_EDGE('',*,*,#13546,.T.);
#19066=ORIENTED_EDGE('',*,*,#13796,.F.);
#19067=ORIENTED_EDGE('',*,*,#13557,.T.);
#19068=ORIENTED_EDGE('',*,*,#13551,.T.);
#19069=ORIENTED_EDGE('',*,*,#13554,.T.);
#19070=ORIENTED_EDGE('',*,*,#13797,.F.);
#19071=ORIENTED_EDGE('',*,*,#13565,.T.);
#19072=ORIENTED_EDGE('',*,*,#13559,.T.);
#19073=ORIENTED_EDGE('',*,*,#13562,.T.);
#19074=ORIENTED_EDGE('',*,*,#13798,.F.);
#19075=ORIENTED_EDGE('',*,*,#13573,.T.);
#19076=ORIENTED_EDGE('',*,*,#13567,.T.);
#19077=ORIENTED_EDGE('',*,*,#13570,.T.);
#19078=ORIENTED_EDGE('',*,*,#13799,.F.);
#19079=ORIENTED_EDGE('',*,*,#13581,.T.);
#19080=ORIENTED_EDGE('',*,*,#13575,.T.);
#19081=ORIENTED_EDGE('',*,*,#13578,.T.);
#19082=ORIENTED_EDGE('',*,*,#13800,.F.);
#19083=ORIENTED_EDGE('',*,*,#13589,.T.);
#19084=ORIENTED_EDGE('',*,*,#13583,.T.);
#19085=ORIENTED_EDGE('',*,*,#13586,.T.);
#19086=ORIENTED_EDGE('',*,*,#13801,.F.);
#19087=ORIENTED_EDGE('',*,*,#13597,.T.);
#19088=ORIENTED_EDGE('',*,*,#13591,.T.);
#19089=ORIENTED_EDGE('',*,*,#13594,.T.);
#19090=ORIENTED_EDGE('',*,*,#13802,.F.);
#19091=ORIENTED_EDGE('',*,*,#13605,.T.);
#19092=ORIENTED_EDGE('',*,*,#13599,.T.);
#19093=ORIENTED_EDGE('',*,*,#13602,.T.);
#19094=ORIENTED_EDGE('',*,*,#13803,.F.);
#19095=ORIENTED_EDGE('',*,*,#13613,.T.);
#19096=ORIENTED_EDGE('',*,*,#13607,.T.);
#19097=ORIENTED_EDGE('',*,*,#13610,.T.);
#19098=ORIENTED_EDGE('',*,*,#13804,.F.);
#19099=ORIENTED_EDGE('',*,*,#13621,.T.);
#19100=ORIENTED_EDGE('',*,*,#13615,.T.);
#19101=ORIENTED_EDGE('',*,*,#13618,.T.);
#19102=ORIENTED_EDGE('',*,*,#13805,.F.);
#19103=ORIENTED_EDGE('',*,*,#13629,.T.);
#19104=ORIENTED_EDGE('',*,*,#13623,.T.);
#19105=ORIENTED_EDGE('',*,*,#13626,.T.);
#19106=ORIENTED_EDGE('',*,*,#13806,.F.);
#19107=ORIENTED_EDGE('',*,*,#13637,.T.);
#19108=ORIENTED_EDGE('',*,*,#13631,.T.);
#19109=ORIENTED_EDGE('',*,*,#13634,.T.);
#19110=ORIENTED_EDGE('',*,*,#13807,.F.);
#19111=ORIENTED_EDGE('',*,*,#13645,.T.);
#19112=ORIENTED_EDGE('',*,*,#13639,.T.);
#19113=ORIENTED_EDGE('',*,*,#13642,.T.);
#19114=ORIENTED_EDGE('',*,*,#13808,.F.);
#19115=ORIENTED_EDGE('',*,*,#13654,.T.);
#19116=ORIENTED_EDGE('',*,*,#13647,.T.);
#19117=ORIENTED_EDGE('',*,*,#13809,.T.);
#19118=ORIENTED_EDGE('',*,*,#13810,.T.);
#19119=ORIENTED_EDGE('',*,*,#13809,.F.);
#19120=ORIENTED_EDGE('',*,*,#13650,.T.);
#19121=ORIENTED_EDGE('',*,*,#13651,.T.);
#19122=ORIENTED_EDGE('',*,*,#13811,.F.);
#19123=ORIENTED_EDGE('',*,*,#13662,.T.);
#19124=ORIENTED_EDGE('',*,*,#13656,.T.);
#19125=ORIENTED_EDGE('',*,*,#13659,.T.);
#19126=ORIENTED_EDGE('',*,*,#13812,.F.);
#19127=ORIENTED_EDGE('',*,*,#13670,.T.);
#19128=ORIENTED_EDGE('',*,*,#13664,.T.);
#19129=ORIENTED_EDGE('',*,*,#13667,.T.);
#19130=ORIENTED_EDGE('',*,*,#13813,.F.);
#19131=ORIENTED_EDGE('',*,*,#13678,.T.);
#19132=ORIENTED_EDGE('',*,*,#13672,.T.);
#19133=ORIENTED_EDGE('',*,*,#13675,.T.);
#19134=ORIENTED_EDGE('',*,*,#13814,.F.);
#19135=ORIENTED_EDGE('',*,*,#13686,.T.);
#19136=ORIENTED_EDGE('',*,*,#13680,.T.);
#19137=ORIENTED_EDGE('',*,*,#13683,.T.);
#19138=ORIENTED_EDGE('',*,*,#13815,.F.);
#19139=ORIENTED_EDGE('',*,*,#13694,.T.);
#19140=ORIENTED_EDGE('',*,*,#13688,.T.);
#19141=ORIENTED_EDGE('',*,*,#13691,.T.);
#19142=ORIENTED_EDGE('',*,*,#13816,.F.);
#19143=ORIENTED_EDGE('',*,*,#13702,.T.);
#19144=ORIENTED_EDGE('',*,*,#13696,.T.);
#19145=ORIENTED_EDGE('',*,*,#13699,.T.);
#19146=ORIENTED_EDGE('',*,*,#13817,.F.);
#19147=ORIENTED_EDGE('',*,*,#13710,.T.);
#19148=ORIENTED_EDGE('',*,*,#13704,.T.);
#19149=ORIENTED_EDGE('',*,*,#13707,.T.);
#19150=ORIENTED_EDGE('',*,*,#13818,.F.);
#19151=ORIENTED_EDGE('',*,*,#13718,.T.);
#19152=ORIENTED_EDGE('',*,*,#13712,.T.);
#19153=ORIENTED_EDGE('',*,*,#13715,.T.);
#19154=ORIENTED_EDGE('',*,*,#13819,.F.);
#19155=ORIENTED_EDGE('',*,*,#13726,.T.);
#19156=ORIENTED_EDGE('',*,*,#13720,.T.);
#19157=ORIENTED_EDGE('',*,*,#13723,.T.);
#19158=ORIENTED_EDGE('',*,*,#13820,.F.);
#19159=ORIENTED_EDGE('',*,*,#13734,.T.);
#19160=ORIENTED_EDGE('',*,*,#13728,.T.);
#19161=ORIENTED_EDGE('',*,*,#13731,.T.);
#19162=ORIENTED_EDGE('',*,*,#13821,.F.);
#19163=ORIENTED_EDGE('',*,*,#13742,.T.);
#19164=ORIENTED_EDGE('',*,*,#13736,.T.);
#19165=ORIENTED_EDGE('',*,*,#13739,.T.);
#19166=ORIENTED_EDGE('',*,*,#13822,.F.);
#19167=ORIENTED_EDGE('',*,*,#13750,.T.);
#19168=ORIENTED_EDGE('',*,*,#13744,.T.);
#19169=ORIENTED_EDGE('',*,*,#13747,.T.);
#19170=ORIENTED_EDGE('',*,*,#13823,.F.);
#19171=ORIENTED_EDGE('',*,*,#13758,.T.);
#19172=ORIENTED_EDGE('',*,*,#13752,.T.);
#19173=ORIENTED_EDGE('',*,*,#13755,.T.);
#19174=ORIENTED_EDGE('',*,*,#13824,.F.);
#19175=ORIENTED_EDGE('',*,*,#13766,.T.);
#19176=ORIENTED_EDGE('',*,*,#13760,.T.);
#19177=ORIENTED_EDGE('',*,*,#13763,.T.);
#19178=ORIENTED_EDGE('',*,*,#13825,.F.);
#19179=ORIENTED_EDGE('',*,*,#13774,.T.);
#19180=ORIENTED_EDGE('',*,*,#13768,.T.);
#19181=ORIENTED_EDGE('',*,*,#13771,.T.);
#19182=ORIENTED_EDGE('',*,*,#13826,.F.);
#19183=ORIENTED_EDGE('',*,*,#13782,.T.);
#19184=ORIENTED_EDGE('',*,*,#13776,.T.);
#19185=ORIENTED_EDGE('',*,*,#13779,.T.);
#19186=ORIENTED_EDGE('',*,*,#13827,.F.);
#19187=ORIENTED_EDGE('',*,*,#13790,.T.);
#19188=ORIENTED_EDGE('',*,*,#13784,.T.);
#19189=ORIENTED_EDGE('',*,*,#13787,.T.);
#19190=ORIENTED_EDGE('',*,*,#13828,.F.);
#19191=ORIENTED_EDGE('',*,*,#13829,.T.);
#19192=ORIENTED_EDGE('',*,*,#13830,.T.);
#19193=ORIENTED_EDGE('',*,*,#13831,.T.);
#19194=ORIENTED_EDGE('',*,*,#13832,.F.);
#19195=ORIENTED_EDGE('',*,*,#13831,.F.);
#19196=ORIENTED_EDGE('',*,*,#13833,.F.);
#19197=ORIENTED_EDGE('',*,*,#13834,.T.);
#19198=ORIENTED_EDGE('',*,*,#13835,.F.);
#19199=ORIENTED_EDGE('',*,*,#13836,.F.);
#19200=ORIENTED_EDGE('',*,*,#13834,.F.);
#19201=ORIENTED_EDGE('',*,*,#13837,.F.);
#19202=ORIENTED_EDGE('',*,*,#13829,.F.);
#19203=ORIENTED_EDGE('',*,*,#13830,.F.);
#19204=ORIENTED_EDGE('',*,*,#13837,.T.);
#19205=ORIENTED_EDGE('',*,*,#13833,.T.);
#19206=ORIENTED_EDGE('',*,*,#13838,.F.);
#19207=ORIENTED_EDGE('',*,*,#13839,.T.);
#19208=ORIENTED_EDGE('',*,*,#13655,.T.);
#19209=ORIENTED_EDGE('',*,*,#13808,.T.);
#19210=ORIENTED_EDGE('',*,*,#13644,.T.);
#19211=ORIENTED_EDGE('',*,*,#13646,.T.);
#19212=ORIENTED_EDGE('',*,*,#13807,.T.);
#19213=ORIENTED_EDGE('',*,*,#13636,.T.);
#19214=ORIENTED_EDGE('',*,*,#13638,.T.);
#19215=ORIENTED_EDGE('',*,*,#13806,.T.);
#19216=ORIENTED_EDGE('',*,*,#13628,.T.);
#19217=ORIENTED_EDGE('',*,*,#13630,.T.);
#19218=ORIENTED_EDGE('',*,*,#13805,.T.);
#19219=ORIENTED_EDGE('',*,*,#13620,.T.);
#19220=ORIENTED_EDGE('',*,*,#13622,.T.);
#19221=ORIENTED_EDGE('',*,*,#13804,.T.);
#19222=ORIENTED_EDGE('',*,*,#13612,.T.);
#19223=ORIENTED_EDGE('',*,*,#13614,.T.);
#19224=ORIENTED_EDGE('',*,*,#13803,.T.);
#19225=ORIENTED_EDGE('',*,*,#13604,.T.);
#19226=ORIENTED_EDGE('',*,*,#13606,.T.);
#19227=ORIENTED_EDGE('',*,*,#13802,.T.);
#19228=ORIENTED_EDGE('',*,*,#13596,.T.);
#19229=ORIENTED_EDGE('',*,*,#13598,.T.);
#19230=ORIENTED_EDGE('',*,*,#13801,.T.);
#19231=ORIENTED_EDGE('',*,*,#13588,.T.);
#19232=ORIENTED_EDGE('',*,*,#13590,.T.);
#19233=ORIENTED_EDGE('',*,*,#13800,.T.);
#19234=ORIENTED_EDGE('',*,*,#13580,.T.);
#19235=ORIENTED_EDGE('',*,*,#13582,.T.);
#19236=ORIENTED_EDGE('',*,*,#13799,.T.);
#19237=ORIENTED_EDGE('',*,*,#13572,.T.);
#19238=ORIENTED_EDGE('',*,*,#13574,.T.);
#19239=ORIENTED_EDGE('',*,*,#13798,.T.);
#19240=ORIENTED_EDGE('',*,*,#13564,.T.);
#19241=ORIENTED_EDGE('',*,*,#13566,.T.);
#19242=ORIENTED_EDGE('',*,*,#13797,.T.);
#19243=ORIENTED_EDGE('',*,*,#13556,.T.);
#19244=ORIENTED_EDGE('',*,*,#13558,.T.);
#19245=ORIENTED_EDGE('',*,*,#13796,.T.);
#19246=ORIENTED_EDGE('',*,*,#13548,.T.);
#19247=ORIENTED_EDGE('',*,*,#13550,.T.);
#19248=ORIENTED_EDGE('',*,*,#13795,.T.);
#19249=ORIENTED_EDGE('',*,*,#13540,.T.);
#19250=ORIENTED_EDGE('',*,*,#13542,.T.);
#19251=ORIENTED_EDGE('',*,*,#13794,.T.);
#19252=ORIENTED_EDGE('',*,*,#13532,.T.);
#19253=ORIENTED_EDGE('',*,*,#13534,.T.);
#19254=ORIENTED_EDGE('',*,*,#13793,.T.);
#19255=ORIENTED_EDGE('',*,*,#13524,.T.);
#19256=ORIENTED_EDGE('',*,*,#13526,.T.);
#19257=ORIENTED_EDGE('',*,*,#13792,.T.);
#19258=ORIENTED_EDGE('',*,*,#13516,.T.);
#19259=ORIENTED_EDGE('',*,*,#13518,.T.);
#19260=ORIENTED_EDGE('',*,*,#13832,.T.);
#19261=ORIENTED_EDGE('',*,*,#13835,.T.);
#19262=ORIENTED_EDGE('',*,*,#13836,.T.);
#19263=ORIENTED_EDGE('',*,*,#13828,.T.);
#19264=ORIENTED_EDGE('',*,*,#13789,.T.);
#19265=ORIENTED_EDGE('',*,*,#13791,.T.);
#19266=ORIENTED_EDGE('',*,*,#13827,.T.);
#19267=ORIENTED_EDGE('',*,*,#13781,.T.);
#19268=ORIENTED_EDGE('',*,*,#13783,.T.);
#19269=ORIENTED_EDGE('',*,*,#13826,.T.);
#19270=ORIENTED_EDGE('',*,*,#13773,.T.);
#19271=ORIENTED_EDGE('',*,*,#13775,.T.);
#19272=ORIENTED_EDGE('',*,*,#13825,.T.);
#19273=ORIENTED_EDGE('',*,*,#13765,.T.);
#19274=ORIENTED_EDGE('',*,*,#13767,.T.);
#19275=ORIENTED_EDGE('',*,*,#13824,.T.);
#19276=ORIENTED_EDGE('',*,*,#13757,.T.);
#19277=ORIENTED_EDGE('',*,*,#13759,.T.);
#19278=ORIENTED_EDGE('',*,*,#13823,.T.);
#19279=ORIENTED_EDGE('',*,*,#13749,.T.);
#19280=ORIENTED_EDGE('',*,*,#13751,.T.);
#19281=ORIENTED_EDGE('',*,*,#13822,.T.);
#19282=ORIENTED_EDGE('',*,*,#13741,.T.);
#19283=ORIENTED_EDGE('',*,*,#13743,.T.);
#19284=ORIENTED_EDGE('',*,*,#13821,.T.);
#19285=ORIENTED_EDGE('',*,*,#13733,.T.);
#19286=ORIENTED_EDGE('',*,*,#13735,.T.);
#19287=ORIENTED_EDGE('',*,*,#13820,.T.);
#19288=ORIENTED_EDGE('',*,*,#13725,.T.);
#19289=ORIENTED_EDGE('',*,*,#13727,.T.);
#19290=ORIENTED_EDGE('',*,*,#13819,.T.);
#19291=ORIENTED_EDGE('',*,*,#13717,.T.);
#19292=ORIENTED_EDGE('',*,*,#13719,.T.);
#19293=ORIENTED_EDGE('',*,*,#13818,.T.);
#19294=ORIENTED_EDGE('',*,*,#13709,.T.);
#19295=ORIENTED_EDGE('',*,*,#13711,.T.);
#19296=ORIENTED_EDGE('',*,*,#13817,.T.);
#19297=ORIENTED_EDGE('',*,*,#13701,.T.);
#19298=ORIENTED_EDGE('',*,*,#13703,.T.);
#19299=ORIENTED_EDGE('',*,*,#13816,.T.);
#19300=ORIENTED_EDGE('',*,*,#13693,.T.);
#19301=ORIENTED_EDGE('',*,*,#13695,.T.);
#19302=ORIENTED_EDGE('',*,*,#13815,.T.);
#19303=ORIENTED_EDGE('',*,*,#13685,.T.);
#19304=ORIENTED_EDGE('',*,*,#13687,.T.);
#19305=ORIENTED_EDGE('',*,*,#13814,.T.);
#19306=ORIENTED_EDGE('',*,*,#13677,.T.);
#19307=ORIENTED_EDGE('',*,*,#13679,.T.);
#19308=ORIENTED_EDGE('',*,*,#13813,.T.);
#19309=ORIENTED_EDGE('',*,*,#13669,.T.);
#19310=ORIENTED_EDGE('',*,*,#13671,.T.);
#19311=ORIENTED_EDGE('',*,*,#13812,.T.);
#19312=ORIENTED_EDGE('',*,*,#13661,.T.);
#19313=ORIENTED_EDGE('',*,*,#13663,.T.);
#19314=ORIENTED_EDGE('',*,*,#13811,.T.);
#19315=ORIENTED_EDGE('',*,*,#13653,.T.);
#19316=ORIENTED_EDGE('',*,*,#13839,.F.);
#19317=ORIENTED_EDGE('',*,*,#13840,.T.);
#19318=ORIENTED_EDGE('',*,*,#13841,.F.);
#19319=ORIENTED_EDGE('',*,*,#13840,.F.);
#19320=ORIENTED_EDGE('',*,*,#13842,.F.);
#19321=ORIENTED_EDGE('',*,*,#13843,.T.);
#19322=ORIENTED_EDGE('',*,*,#13844,.T.);
#19323=ORIENTED_EDGE('',*,*,#13845,.F.);
#19324=ORIENTED_EDGE('',*,*,#13846,.F.);
#19325=ORIENTED_EDGE('',*,*,#13847,.T.);
#19326=ORIENTED_EDGE('',*,*,#13848,.T.);
#19327=ORIENTED_EDGE('',*,*,#13843,.F.);
#19328=ORIENTED_EDGE('',*,*,#13849,.F.);
#19329=ORIENTED_EDGE('',*,*,#13850,.T.);
#19330=ORIENTED_EDGE('',*,*,#13851,.T.);
#19331=ORIENTED_EDGE('',*,*,#13847,.F.);
#19332=ORIENTED_EDGE('',*,*,#13852,.F.);
#19333=ORIENTED_EDGE('',*,*,#13853,.T.);
#19334=ORIENTED_EDGE('',*,*,#13854,.T.);
#19335=ORIENTED_EDGE('',*,*,#13850,.F.);
#19336=ORIENTED_EDGE('',*,*,#13855,.F.);
#19337=ORIENTED_EDGE('',*,*,#13856,.T.);
#19338=ORIENTED_EDGE('',*,*,#13857,.T.);
#19339=ORIENTED_EDGE('',*,*,#13853,.F.);
#19340=ORIENTED_EDGE('',*,*,#13858,.F.);
#19341=ORIENTED_EDGE('',*,*,#13845,.T.);
#19342=ORIENTED_EDGE('',*,*,#13859,.T.);
#19343=ORIENTED_EDGE('',*,*,#13856,.F.);
#19344=ORIENTED_EDGE('',*,*,#13859,.F.);
#19345=ORIENTED_EDGE('',*,*,#13844,.F.);
#19346=ORIENTED_EDGE('',*,*,#13848,.F.);
#19347=ORIENTED_EDGE('',*,*,#13851,.F.);
#19348=ORIENTED_EDGE('',*,*,#13854,.F.);
#19349=ORIENTED_EDGE('',*,*,#13857,.F.);
#19350=ORIENTED_EDGE('',*,*,#13841,.T.);
#19351=ORIENTED_EDGE('',*,*,#13860,.F.);
#19352=ORIENTED_EDGE('',*,*,#13412,.F.);
#19353=ORIENTED_EDGE('',*,*,#13861,.T.);
#19354=ORIENTED_EDGE('',*,*,#13860,.T.);
#19355=ORIENTED_EDGE('',*,*,#13861,.F.);
#19356=ORIENTED_EDGE('',*,*,#13451,.T.);
#19357=ORIENTED_EDGE('',*,*,#13504,.T.);
#19358=ORIENTED_EDGE('',*,*,#13862,.F.);
#19359=ORIENTED_EDGE('',*,*,#13510,.T.);
#19360=ORIENTED_EDGE('',*,*,#13863,.F.);
#19361=ORIENTED_EDGE('',*,*,#13864,.T.);
#19362=ORIENTED_EDGE('',*,*,#13501,.T.);
#19363=ORIENTED_EDGE('',*,*,#13862,.T.);
#19364=ORIENTED_EDGE('',*,*,#13502,.T.);
#19365=ORIENTED_EDGE('',*,*,#13864,.F.);
#19366=ORIENTED_EDGE('',*,*,#13810,.F.);
#19367=ORIENTED_EDGE('',*,*,#13863,.T.);
#19368=ORIENTED_EDGE('',*,*,#13838,.T.);
#19369=ORIENTED_EDGE('',*,*,#13842,.T.);
#19370=ORIENTED_EDGE('',*,*,#13858,.T.);
#19371=ORIENTED_EDGE('',*,*,#13855,.T.);
#19372=ORIENTED_EDGE('',*,*,#13852,.T.);
#19373=ORIENTED_EDGE('',*,*,#13849,.T.);
#19374=ORIENTED_EDGE('',*,*,#13846,.T.);
#19375=ORIENTED_EDGE('',*,*,#13865,.F.);
#19376=ORIENTED_EDGE('',*,*,#13866,.T.);
#19377=ORIENTED_EDGE('',*,*,#13867,.T.);
#19378=ORIENTED_EDGE('',*,*,#13868,.T.);
#19379=ORIENTED_EDGE('',*,*,#13869,.T.);
#19380=ORIENTED_EDGE('',*,*,#13868,.F.);
#19381=ORIENTED_EDGE('',*,*,#13870,.T.);
#19382=ORIENTED_EDGE('',*,*,#13871,.T.);
#19383=ORIENTED_EDGE('',*,*,#13872,.F.);
#19384=ORIENTED_EDGE('',*,*,#13873,.T.);
#19385=ORIENTED_EDGE('',*,*,#13865,.T.);
#19386=ORIENTED_EDGE('',*,*,#13874,.T.);
#19387=ORIENTED_EDGE('',*,*,#13875,.F.);
#19388=ORIENTED_EDGE('',*,*,#13876,.T.);
#19389=ORIENTED_EDGE('',*,*,#13872,.T.);
#19390=ORIENTED_EDGE('',*,*,#13877,.T.);
#19391=ORIENTED_EDGE('',*,*,#13878,.F.);
#19392=ORIENTED_EDGE('',*,*,#13879,.T.);
#19393=ORIENTED_EDGE('',*,*,#13875,.T.);
#19394=ORIENTED_EDGE('',*,*,#13880,.T.);
#19395=ORIENTED_EDGE('',*,*,#13881,.F.);
#19396=ORIENTED_EDGE('',*,*,#13882,.T.);
#19397=ORIENTED_EDGE('',*,*,#13878,.T.);
#19398=ORIENTED_EDGE('',*,*,#13883,.T.);
#19399=ORIENTED_EDGE('',*,*,#13884,.F.);
#19400=ORIENTED_EDGE('',*,*,#13885,.T.);
#19401=ORIENTED_EDGE('',*,*,#13881,.T.);
#19402=ORIENTED_EDGE('',*,*,#13886,.T.);
#19403=ORIENTED_EDGE('',*,*,#13887,.F.);
#19404=ORIENTED_EDGE('',*,*,#13888,.T.);
#19405=ORIENTED_EDGE('',*,*,#13884,.T.);
#19406=ORIENTED_EDGE('',*,*,#13889,.T.);
#19407=ORIENTED_EDGE('',*,*,#13890,.F.);
#19408=ORIENTED_EDGE('',*,*,#13891,.T.);
#19409=ORIENTED_EDGE('',*,*,#13887,.T.);
#19410=ORIENTED_EDGE('',*,*,#13892,.T.);
#19411=ORIENTED_EDGE('',*,*,#13893,.F.);
#19412=ORIENTED_EDGE('',*,*,#13894,.T.);
#19413=ORIENTED_EDGE('',*,*,#13890,.T.);
#19414=ORIENTED_EDGE('',*,*,#13895,.T.);
#19415=ORIENTED_EDGE('',*,*,#13896,.F.);
#19416=ORIENTED_EDGE('',*,*,#13897,.T.);
#19417=ORIENTED_EDGE('',*,*,#13893,.T.);
#19418=ORIENTED_EDGE('',*,*,#13898,.T.);
#19419=ORIENTED_EDGE('',*,*,#13899,.F.);
#19420=ORIENTED_EDGE('',*,*,#13900,.T.);
#19421=ORIENTED_EDGE('',*,*,#13896,.T.);
#19422=ORIENTED_EDGE('',*,*,#13901,.T.);
#19423=ORIENTED_EDGE('',*,*,#13902,.F.);
#19424=ORIENTED_EDGE('',*,*,#13903,.T.);
#19425=ORIENTED_EDGE('',*,*,#13899,.T.);
#19426=ORIENTED_EDGE('',*,*,#13904,.T.);
#19427=ORIENTED_EDGE('',*,*,#13905,.F.);
#19428=ORIENTED_EDGE('',*,*,#13906,.T.);
#19429=ORIENTED_EDGE('',*,*,#13902,.T.);
#19430=ORIENTED_EDGE('',*,*,#13907,.T.);
#19431=ORIENTED_EDGE('',*,*,#13908,.F.);
#19432=ORIENTED_EDGE('',*,*,#13909,.T.);
#19433=ORIENTED_EDGE('',*,*,#13905,.T.);
#19434=ORIENTED_EDGE('',*,*,#13910,.T.);
#19435=ORIENTED_EDGE('',*,*,#13911,.F.);
#19436=ORIENTED_EDGE('',*,*,#13912,.T.);
#19437=ORIENTED_EDGE('',*,*,#13908,.T.);
#19438=ORIENTED_EDGE('',*,*,#13913,.T.);
#19439=ORIENTED_EDGE('',*,*,#13914,.F.);
#19440=ORIENTED_EDGE('',*,*,#13915,.T.);
#19441=ORIENTED_EDGE('',*,*,#13911,.T.);
#19442=ORIENTED_EDGE('',*,*,#13916,.T.);
#19443=ORIENTED_EDGE('',*,*,#13917,.F.);
#19444=ORIENTED_EDGE('',*,*,#13918,.T.);
#19445=ORIENTED_EDGE('',*,*,#13914,.T.);
#19446=ORIENTED_EDGE('',*,*,#13919,.T.);
#19447=ORIENTED_EDGE('',*,*,#13920,.F.);
#19448=ORIENTED_EDGE('',*,*,#13921,.T.);
#19449=ORIENTED_EDGE('',*,*,#13917,.T.);
#19450=ORIENTED_EDGE('',*,*,#13922,.T.);
#19451=ORIENTED_EDGE('',*,*,#13923,.F.);
#19452=ORIENTED_EDGE('',*,*,#13924,.T.);
#19453=ORIENTED_EDGE('',*,*,#13920,.T.);
#19454=ORIENTED_EDGE('',*,*,#13925,.T.);
#19455=ORIENTED_EDGE('',*,*,#13926,.F.);
#19456=ORIENTED_EDGE('',*,*,#13927,.T.);
#19457=ORIENTED_EDGE('',*,*,#13923,.T.);
#19458=ORIENTED_EDGE('',*,*,#13928,.T.);
#19459=ORIENTED_EDGE('',*,*,#13929,.F.);
#19460=ORIENTED_EDGE('',*,*,#13930,.T.);
#19461=ORIENTED_EDGE('',*,*,#13926,.T.);
#19462=ORIENTED_EDGE('',*,*,#13931,.T.);
#19463=ORIENTED_EDGE('',*,*,#13932,.F.);
#19464=ORIENTED_EDGE('',*,*,#13933,.T.);
#19465=ORIENTED_EDGE('',*,*,#13929,.T.);
#19466=ORIENTED_EDGE('',*,*,#13934,.T.);
#19467=ORIENTED_EDGE('',*,*,#13935,.F.);
#19468=ORIENTED_EDGE('',*,*,#13936,.T.);
#19469=ORIENTED_EDGE('',*,*,#13932,.T.);
#19470=ORIENTED_EDGE('',*,*,#13937,.T.);
#19471=ORIENTED_EDGE('',*,*,#13938,.F.);
#19472=ORIENTED_EDGE('',*,*,#13939,.T.);
#19473=ORIENTED_EDGE('',*,*,#13935,.T.);
#19474=ORIENTED_EDGE('',*,*,#13940,.T.);
#19475=ORIENTED_EDGE('',*,*,#13941,.F.);
#19476=ORIENTED_EDGE('',*,*,#13942,.T.);
#19477=ORIENTED_EDGE('',*,*,#13938,.T.);
#19478=ORIENTED_EDGE('',*,*,#13943,.T.);
#19479=ORIENTED_EDGE('',*,*,#13944,.F.);
#19480=ORIENTED_EDGE('',*,*,#13945,.T.);
#19481=ORIENTED_EDGE('',*,*,#13941,.T.);
#19482=ORIENTED_EDGE('',*,*,#13946,.T.);
#19483=ORIENTED_EDGE('',*,*,#13947,.F.);
#19484=ORIENTED_EDGE('',*,*,#13948,.T.);
#19485=ORIENTED_EDGE('',*,*,#13944,.T.);
#19486=ORIENTED_EDGE('',*,*,#13949,.T.);
#19487=ORIENTED_EDGE('',*,*,#13950,.F.);
#19488=ORIENTED_EDGE('',*,*,#13951,.T.);
#19489=ORIENTED_EDGE('',*,*,#13947,.T.);
#19490=ORIENTED_EDGE('',*,*,#13952,.T.);
#19491=ORIENTED_EDGE('',*,*,#13953,.F.);
#19492=ORIENTED_EDGE('',*,*,#13954,.T.);
#19493=ORIENTED_EDGE('',*,*,#13950,.T.);
#19494=ORIENTED_EDGE('',*,*,#13955,.T.);
#19495=ORIENTED_EDGE('',*,*,#13956,.F.);
#19496=ORIENTED_EDGE('',*,*,#13957,.T.);
#19497=ORIENTED_EDGE('',*,*,#13953,.T.);
#19498=ORIENTED_EDGE('',*,*,#13958,.T.);
#19499=ORIENTED_EDGE('',*,*,#13959,.F.);
#19500=ORIENTED_EDGE('',*,*,#13960,.T.);
#19501=ORIENTED_EDGE('',*,*,#13956,.T.);
#19502=ORIENTED_EDGE('',*,*,#13961,.T.);
#19503=ORIENTED_EDGE('',*,*,#13962,.F.);
#19504=ORIENTED_EDGE('',*,*,#13963,.T.);
#19505=ORIENTED_EDGE('',*,*,#13959,.T.);
#19506=ORIENTED_EDGE('',*,*,#13964,.T.);
#19507=ORIENTED_EDGE('',*,*,#13965,.F.);
#19508=ORIENTED_EDGE('',*,*,#13966,.T.);
#19509=ORIENTED_EDGE('',*,*,#13962,.T.);
#19510=ORIENTED_EDGE('',*,*,#13967,.T.);
#19511=ORIENTED_EDGE('',*,*,#13968,.F.);
#19512=ORIENTED_EDGE('',*,*,#13969,.T.);
#19513=ORIENTED_EDGE('',*,*,#13965,.T.);
#19514=ORIENTED_EDGE('',*,*,#13970,.T.);
#19515=ORIENTED_EDGE('',*,*,#13971,.F.);
#19516=ORIENTED_EDGE('',*,*,#13972,.T.);
#19517=ORIENTED_EDGE('',*,*,#13968,.T.);
#19518=ORIENTED_EDGE('',*,*,#13973,.T.);
#19519=ORIENTED_EDGE('',*,*,#13974,.F.);
#19520=ORIENTED_EDGE('',*,*,#13975,.T.);
#19521=ORIENTED_EDGE('',*,*,#13971,.T.);
#19522=ORIENTED_EDGE('',*,*,#13976,.T.);
#19523=ORIENTED_EDGE('',*,*,#13977,.F.);
#19524=ORIENTED_EDGE('',*,*,#13978,.T.);
#19525=ORIENTED_EDGE('',*,*,#13974,.T.);
#19526=ORIENTED_EDGE('',*,*,#13979,.T.);
#19527=ORIENTED_EDGE('',*,*,#13980,.F.);
#19528=ORIENTED_EDGE('',*,*,#13981,.T.);
#19529=ORIENTED_EDGE('',*,*,#13977,.T.);
#19530=ORIENTED_EDGE('',*,*,#13982,.T.);
#19531=ORIENTED_EDGE('',*,*,#13983,.F.);
#19532=ORIENTED_EDGE('',*,*,#13984,.T.);
#19533=ORIENTED_EDGE('',*,*,#13980,.T.);
#19534=ORIENTED_EDGE('',*,*,#13985,.T.);
#19535=ORIENTED_EDGE('',*,*,#13986,.F.);
#19536=ORIENTED_EDGE('',*,*,#13987,.T.);
#19537=ORIENTED_EDGE('',*,*,#13983,.T.);
#19538=ORIENTED_EDGE('',*,*,#13988,.T.);
#19539=ORIENTED_EDGE('',*,*,#13989,.F.);
#19540=ORIENTED_EDGE('',*,*,#13990,.T.);
#19541=ORIENTED_EDGE('',*,*,#13986,.T.);
#19542=ORIENTED_EDGE('',*,*,#13991,.T.);
#19543=ORIENTED_EDGE('',*,*,#13992,.F.);
#19544=ORIENTED_EDGE('',*,*,#13993,.T.);
#19545=ORIENTED_EDGE('',*,*,#13989,.T.);
#19546=ORIENTED_EDGE('',*,*,#13994,.T.);
#19547=ORIENTED_EDGE('',*,*,#13995,.F.);
#19548=ORIENTED_EDGE('',*,*,#13996,.T.);
#19549=ORIENTED_EDGE('',*,*,#13992,.T.);
#19550=ORIENTED_EDGE('',*,*,#13997,.T.);
#19551=ORIENTED_EDGE('',*,*,#13998,.F.);
#19552=ORIENTED_EDGE('',*,*,#13999,.T.);
#19553=ORIENTED_EDGE('',*,*,#13995,.T.);
#19554=ORIENTED_EDGE('',*,*,#14000,.T.);
#19555=ORIENTED_EDGE('',*,*,#14001,.F.);
#19556=ORIENTED_EDGE('',*,*,#14002,.T.);
#19557=ORIENTED_EDGE('',*,*,#13998,.T.);
#19558=ORIENTED_EDGE('',*,*,#14003,.T.);
#19559=ORIENTED_EDGE('',*,*,#14004,.F.);
#19560=ORIENTED_EDGE('',*,*,#14005,.T.);
#19561=ORIENTED_EDGE('',*,*,#14001,.T.);
#19562=ORIENTED_EDGE('',*,*,#14006,.T.);
#19563=ORIENTED_EDGE('',*,*,#14007,.F.);
#19564=ORIENTED_EDGE('',*,*,#14008,.T.);
#19565=ORIENTED_EDGE('',*,*,#14004,.T.);
#19566=ORIENTED_EDGE('',*,*,#14009,.T.);
#19567=ORIENTED_EDGE('',*,*,#14010,.F.);
#19568=ORIENTED_EDGE('',*,*,#14011,.T.);
#19569=ORIENTED_EDGE('',*,*,#14007,.T.);
#19570=ORIENTED_EDGE('',*,*,#14012,.T.);
#19571=ORIENTED_EDGE('',*,*,#14013,.F.);
#19572=ORIENTED_EDGE('',*,*,#14014,.T.);
#19573=ORIENTED_EDGE('',*,*,#14010,.T.);
#19574=ORIENTED_EDGE('',*,*,#14015,.T.);
#19575=ORIENTED_EDGE('',*,*,#14016,.F.);
#19576=ORIENTED_EDGE('',*,*,#14017,.T.);
#19577=ORIENTED_EDGE('',*,*,#14013,.T.);
#19578=ORIENTED_EDGE('',*,*,#14018,.T.);
#19579=ORIENTED_EDGE('',*,*,#14019,.F.);
#19580=ORIENTED_EDGE('',*,*,#14020,.T.);
#19581=ORIENTED_EDGE('',*,*,#14016,.T.);
#19582=ORIENTED_EDGE('',*,*,#14021,.T.);
#19583=ORIENTED_EDGE('',*,*,#14022,.F.);
#19584=ORIENTED_EDGE('',*,*,#14023,.T.);
#19585=ORIENTED_EDGE('',*,*,#14019,.T.);
#19586=ORIENTED_EDGE('',*,*,#14024,.T.);
#19587=ORIENTED_EDGE('',*,*,#14025,.F.);
#19588=ORIENTED_EDGE('',*,*,#14026,.T.);
#19589=ORIENTED_EDGE('',*,*,#14022,.T.);
#19590=ORIENTED_EDGE('',*,*,#14027,.T.);
#19591=ORIENTED_EDGE('',*,*,#14028,.F.);
#19592=ORIENTED_EDGE('',*,*,#14029,.T.);
#19593=ORIENTED_EDGE('',*,*,#14025,.T.);
#19594=ORIENTED_EDGE('',*,*,#14030,.T.);
#19595=ORIENTED_EDGE('',*,*,#14031,.F.);
#19596=ORIENTED_EDGE('',*,*,#14032,.T.);
#19597=ORIENTED_EDGE('',*,*,#14028,.T.);
#19598=ORIENTED_EDGE('',*,*,#14033,.T.);
#19599=ORIENTED_EDGE('',*,*,#14034,.F.);
#19600=ORIENTED_EDGE('',*,*,#14035,.T.);
#19601=ORIENTED_EDGE('',*,*,#14031,.T.);
#19602=ORIENTED_EDGE('',*,*,#14036,.T.);
#19603=ORIENTED_EDGE('',*,*,#14037,.F.);
#19604=ORIENTED_EDGE('',*,*,#14038,.T.);
#19605=ORIENTED_EDGE('',*,*,#14034,.T.);
#19606=ORIENTED_EDGE('',*,*,#14039,.T.);
#19607=ORIENTED_EDGE('',*,*,#14040,.F.);
#19608=ORIENTED_EDGE('',*,*,#14041,.T.);
#19609=ORIENTED_EDGE('',*,*,#14037,.T.);
#19610=ORIENTED_EDGE('',*,*,#14042,.T.);
#19611=ORIENTED_EDGE('',*,*,#14043,.F.);
#19612=ORIENTED_EDGE('',*,*,#14044,.T.);
#19613=ORIENTED_EDGE('',*,*,#14045,.F.);
#19614=ORIENTED_EDGE('',*,*,#14046,.F.);
#19615=ORIENTED_EDGE('',*,*,#14047,.F.);
#19616=ORIENTED_EDGE('',*,*,#14048,.T.);
#19617=ORIENTED_EDGE('',*,*,#14043,.T.);
#19618=ORIENTED_EDGE('',*,*,#14049,.F.);
#19619=ORIENTED_EDGE('',*,*,#14050,.F.);
#19620=ORIENTED_EDGE('',*,*,#14051,.T.);
#19621=ORIENTED_EDGE('',*,*,#14047,.T.);
#19622=ORIENTED_EDGE('',*,*,#14052,.F.);
#19623=ORIENTED_EDGE('',*,*,#14053,.F.);
#19624=ORIENTED_EDGE('',*,*,#14054,.T.);
#19625=ORIENTED_EDGE('',*,*,#14050,.T.);
#19626=ORIENTED_EDGE('',*,*,#14055,.F.);
#19627=ORIENTED_EDGE('',*,*,#14056,.F.);
#19628=ORIENTED_EDGE('',*,*,#14057,.T.);
#19629=ORIENTED_EDGE('',*,*,#14053,.T.);
#19630=ORIENTED_EDGE('',*,*,#14058,.F.);
#19631=ORIENTED_EDGE('',*,*,#14059,.F.);
#19632=ORIENTED_EDGE('',*,*,#14060,.T.);
#19633=ORIENTED_EDGE('',*,*,#14056,.T.);
#19634=ORIENTED_EDGE('',*,*,#14061,.F.);
#19635=ORIENTED_EDGE('',*,*,#14062,.F.);
#19636=ORIENTED_EDGE('',*,*,#14063,.T.);
#19637=ORIENTED_EDGE('',*,*,#14059,.T.);
#19638=ORIENTED_EDGE('',*,*,#14064,.F.);
#19639=ORIENTED_EDGE('',*,*,#14065,.F.);
#19640=ORIENTED_EDGE('',*,*,#14066,.T.);
#19641=ORIENTED_EDGE('',*,*,#14062,.T.);
#19642=ORIENTED_EDGE('',*,*,#14067,.F.);
#19643=ORIENTED_EDGE('',*,*,#14068,.F.);
#19644=ORIENTED_EDGE('',*,*,#14069,.T.);
#19645=ORIENTED_EDGE('',*,*,#14065,.T.);
#19646=ORIENTED_EDGE('',*,*,#14070,.F.);
#19647=ORIENTED_EDGE('',*,*,#14071,.F.);
#19648=ORIENTED_EDGE('',*,*,#14072,.T.);
#19649=ORIENTED_EDGE('',*,*,#14068,.T.);
#19650=ORIENTED_EDGE('',*,*,#14073,.F.);
#19651=ORIENTED_EDGE('',*,*,#14074,.F.);
#19652=ORIENTED_EDGE('',*,*,#14075,.T.);
#19653=ORIENTED_EDGE('',*,*,#14071,.T.);
#19654=ORIENTED_EDGE('',*,*,#14076,.F.);
#19655=ORIENTED_EDGE('',*,*,#14077,.F.);
#19656=ORIENTED_EDGE('',*,*,#14078,.T.);
#19657=ORIENTED_EDGE('',*,*,#14074,.T.);
#19658=ORIENTED_EDGE('',*,*,#14079,.F.);
#19659=ORIENTED_EDGE('',*,*,#14080,.F.);
#19660=ORIENTED_EDGE('',*,*,#14081,.T.);
#19661=ORIENTED_EDGE('',*,*,#14077,.T.);
#19662=ORIENTED_EDGE('',*,*,#14082,.F.);
#19663=ORIENTED_EDGE('',*,*,#14083,.F.);
#19664=ORIENTED_EDGE('',*,*,#14084,.T.);
#19665=ORIENTED_EDGE('',*,*,#14080,.T.);
#19666=ORIENTED_EDGE('',*,*,#14085,.F.);
#19667=ORIENTED_EDGE('',*,*,#14086,.F.);
#19668=ORIENTED_EDGE('',*,*,#14087,.T.);
#19669=ORIENTED_EDGE('',*,*,#14083,.T.);
#19670=ORIENTED_EDGE('',*,*,#14088,.F.);
#19671=ORIENTED_EDGE('',*,*,#14089,.F.);
#19672=ORIENTED_EDGE('',*,*,#14090,.T.);
#19673=ORIENTED_EDGE('',*,*,#14086,.T.);
#19674=ORIENTED_EDGE('',*,*,#14091,.F.);
#19675=ORIENTED_EDGE('',*,*,#14092,.F.);
#19676=ORIENTED_EDGE('',*,*,#14093,.T.);
#19677=ORIENTED_EDGE('',*,*,#14089,.T.);
#19678=ORIENTED_EDGE('',*,*,#14094,.F.);
#19679=ORIENTED_EDGE('',*,*,#14095,.F.);
#19680=ORIENTED_EDGE('',*,*,#14096,.T.);
#19681=ORIENTED_EDGE('',*,*,#14092,.T.);
#19682=ORIENTED_EDGE('',*,*,#14097,.F.);
#19683=ORIENTED_EDGE('',*,*,#14098,.F.);
#19684=ORIENTED_EDGE('',*,*,#14099,.T.);
#19685=ORIENTED_EDGE('',*,*,#14095,.T.);
#19686=ORIENTED_EDGE('',*,*,#14100,.F.);
#19687=ORIENTED_EDGE('',*,*,#14101,.F.);
#19688=ORIENTED_EDGE('',*,*,#14102,.T.);
#19689=ORIENTED_EDGE('',*,*,#14098,.T.);
#19690=ORIENTED_EDGE('',*,*,#14103,.F.);
#19691=ORIENTED_EDGE('',*,*,#14104,.F.);
#19692=ORIENTED_EDGE('',*,*,#14105,.T.);
#19693=ORIENTED_EDGE('',*,*,#14101,.T.);
#19694=ORIENTED_EDGE('',*,*,#14106,.F.);
#19695=ORIENTED_EDGE('',*,*,#14107,.F.);
#19696=ORIENTED_EDGE('',*,*,#14108,.T.);
#19697=ORIENTED_EDGE('',*,*,#14104,.T.);
#19698=ORIENTED_EDGE('',*,*,#14109,.F.);
#19699=ORIENTED_EDGE('',*,*,#14110,.F.);
#19700=ORIENTED_EDGE('',*,*,#14111,.T.);
#19701=ORIENTED_EDGE('',*,*,#14107,.T.);
#19702=ORIENTED_EDGE('',*,*,#14112,.F.);
#19703=ORIENTED_EDGE('',*,*,#14113,.F.);
#19704=ORIENTED_EDGE('',*,*,#14114,.T.);
#19705=ORIENTED_EDGE('',*,*,#14110,.T.);
#19706=ORIENTED_EDGE('',*,*,#14115,.F.);
#19707=ORIENTED_EDGE('',*,*,#14116,.F.);
#19708=ORIENTED_EDGE('',*,*,#14117,.T.);
#19709=ORIENTED_EDGE('',*,*,#14113,.T.);
#19710=ORIENTED_EDGE('',*,*,#14118,.F.);
#19711=ORIENTED_EDGE('',*,*,#14119,.F.);
#19712=ORIENTED_EDGE('',*,*,#14120,.T.);
#19713=ORIENTED_EDGE('',*,*,#14116,.T.);
#19714=ORIENTED_EDGE('',*,*,#14121,.F.);
#19715=ORIENTED_EDGE('',*,*,#14122,.F.);
#19716=ORIENTED_EDGE('',*,*,#14123,.T.);
#19717=ORIENTED_EDGE('',*,*,#14119,.T.);
#19718=ORIENTED_EDGE('',*,*,#14124,.F.);
#19719=ORIENTED_EDGE('',*,*,#14125,.F.);
#19720=ORIENTED_EDGE('',*,*,#14126,.T.);
#19721=ORIENTED_EDGE('',*,*,#14122,.T.);
#19722=ORIENTED_EDGE('',*,*,#14127,.F.);
#19723=ORIENTED_EDGE('',*,*,#14128,.F.);
#19724=ORIENTED_EDGE('',*,*,#14129,.T.);
#19725=ORIENTED_EDGE('',*,*,#14125,.T.);
#19726=ORIENTED_EDGE('',*,*,#14130,.F.);
#19727=ORIENTED_EDGE('',*,*,#14131,.F.);
#19728=ORIENTED_EDGE('',*,*,#14132,.T.);
#19729=ORIENTED_EDGE('',*,*,#14128,.T.);
#19730=ORIENTED_EDGE('',*,*,#14133,.F.);
#19731=ORIENTED_EDGE('',*,*,#14134,.F.);
#19732=ORIENTED_EDGE('',*,*,#14135,.T.);
#19733=ORIENTED_EDGE('',*,*,#14131,.T.);
#19734=ORIENTED_EDGE('',*,*,#14136,.F.);
#19735=ORIENTED_EDGE('',*,*,#14137,.F.);
#19736=ORIENTED_EDGE('',*,*,#14138,.T.);
#19737=ORIENTED_EDGE('',*,*,#14134,.T.);
#19738=ORIENTED_EDGE('',*,*,#14139,.F.);
#19739=ORIENTED_EDGE('',*,*,#14140,.F.);
#19740=ORIENTED_EDGE('',*,*,#14141,.T.);
#19741=ORIENTED_EDGE('',*,*,#14137,.T.);
#19742=ORIENTED_EDGE('',*,*,#14142,.F.);
#19743=ORIENTED_EDGE('',*,*,#14143,.F.);
#19744=ORIENTED_EDGE('',*,*,#14144,.T.);
#19745=ORIENTED_EDGE('',*,*,#14140,.T.);
#19746=ORIENTED_EDGE('',*,*,#14145,.F.);
#19747=ORIENTED_EDGE('',*,*,#14146,.F.);
#19748=ORIENTED_EDGE('',*,*,#14147,.T.);
#19749=ORIENTED_EDGE('',*,*,#14143,.T.);
#19750=ORIENTED_EDGE('',*,*,#14148,.F.);
#19751=ORIENTED_EDGE('',*,*,#14149,.F.);
#19752=ORIENTED_EDGE('',*,*,#14150,.T.);
#19753=ORIENTED_EDGE('',*,*,#14146,.T.);
#19754=ORIENTED_EDGE('',*,*,#14151,.F.);
#19755=ORIENTED_EDGE('',*,*,#14152,.F.);
#19756=ORIENTED_EDGE('',*,*,#14153,.T.);
#19757=ORIENTED_EDGE('',*,*,#14149,.T.);
#19758=ORIENTED_EDGE('',*,*,#14154,.F.);
#19759=ORIENTED_EDGE('',*,*,#14155,.F.);
#19760=ORIENTED_EDGE('',*,*,#14156,.T.);
#19761=ORIENTED_EDGE('',*,*,#14152,.T.);
#19762=ORIENTED_EDGE('',*,*,#14157,.F.);
#19763=ORIENTED_EDGE('',*,*,#14158,.F.);
#19764=ORIENTED_EDGE('',*,*,#14159,.T.);
#19765=ORIENTED_EDGE('',*,*,#14155,.T.);
#19766=ORIENTED_EDGE('',*,*,#14160,.F.);
#19767=ORIENTED_EDGE('',*,*,#14161,.F.);
#19768=ORIENTED_EDGE('',*,*,#14162,.T.);
#19769=ORIENTED_EDGE('',*,*,#14158,.T.);
#19770=ORIENTED_EDGE('',*,*,#14163,.F.);
#19771=ORIENTED_EDGE('',*,*,#14164,.F.);
#19772=ORIENTED_EDGE('',*,*,#14165,.T.);
#19773=ORIENTED_EDGE('',*,*,#14161,.T.);
#19774=ORIENTED_EDGE('',*,*,#14166,.F.);
#19775=ORIENTED_EDGE('',*,*,#14167,.F.);
#19776=ORIENTED_EDGE('',*,*,#14168,.T.);
#19777=ORIENTED_EDGE('',*,*,#14164,.T.);
#19778=ORIENTED_EDGE('',*,*,#14169,.F.);
#19779=ORIENTED_EDGE('',*,*,#14170,.F.);
#19780=ORIENTED_EDGE('',*,*,#14171,.T.);
#19781=ORIENTED_EDGE('',*,*,#14167,.T.);
#19782=ORIENTED_EDGE('',*,*,#14172,.F.);
#19783=ORIENTED_EDGE('',*,*,#14173,.F.);
#19784=ORIENTED_EDGE('',*,*,#14174,.T.);
#19785=ORIENTED_EDGE('',*,*,#14170,.T.);
#19786=ORIENTED_EDGE('',*,*,#14175,.F.);
#19787=ORIENTED_EDGE('',*,*,#14176,.F.);
#19788=ORIENTED_EDGE('',*,*,#14177,.T.);
#19789=ORIENTED_EDGE('',*,*,#14173,.T.);
#19790=ORIENTED_EDGE('',*,*,#14178,.F.);
#19791=ORIENTED_EDGE('',*,*,#14179,.F.);
#19792=ORIENTED_EDGE('',*,*,#14180,.T.);
#19793=ORIENTED_EDGE('',*,*,#14176,.T.);
#19794=ORIENTED_EDGE('',*,*,#14181,.F.);
#19795=ORIENTED_EDGE('',*,*,#14182,.F.);
#19796=ORIENTED_EDGE('',*,*,#14183,.T.);
#19797=ORIENTED_EDGE('',*,*,#14179,.T.);
#19798=ORIENTED_EDGE('',*,*,#14184,.F.);
#19799=ORIENTED_EDGE('',*,*,#14185,.F.);
#19800=ORIENTED_EDGE('',*,*,#14186,.T.);
#19801=ORIENTED_EDGE('',*,*,#14182,.T.);
#19802=ORIENTED_EDGE('',*,*,#14187,.F.);
#19803=ORIENTED_EDGE('',*,*,#14188,.F.);
#19804=ORIENTED_EDGE('',*,*,#14189,.T.);
#19805=ORIENTED_EDGE('',*,*,#14185,.T.);
#19806=ORIENTED_EDGE('',*,*,#14190,.F.);
#19807=ORIENTED_EDGE('',*,*,#14191,.F.);
#19808=ORIENTED_EDGE('',*,*,#14192,.T.);
#19809=ORIENTED_EDGE('',*,*,#14188,.T.);
#19810=ORIENTED_EDGE('',*,*,#14193,.F.);
#19811=ORIENTED_EDGE('',*,*,#14194,.F.);
#19812=ORIENTED_EDGE('',*,*,#14195,.T.);
#19813=ORIENTED_EDGE('',*,*,#14191,.T.);
#19814=ORIENTED_EDGE('',*,*,#14196,.F.);
#19815=ORIENTED_EDGE('',*,*,#14197,.F.);
#19816=ORIENTED_EDGE('',*,*,#14198,.T.);
#19817=ORIENTED_EDGE('',*,*,#14194,.T.);
#19818=ORIENTED_EDGE('',*,*,#14199,.F.);
#19819=ORIENTED_EDGE('',*,*,#14200,.F.);
#19820=ORIENTED_EDGE('',*,*,#14201,.T.);
#19821=ORIENTED_EDGE('',*,*,#14197,.T.);
#19822=ORIENTED_EDGE('',*,*,#14202,.F.);
#19823=ORIENTED_EDGE('',*,*,#14203,.F.);
#19824=ORIENTED_EDGE('',*,*,#14204,.T.);
#19825=ORIENTED_EDGE('',*,*,#14200,.T.);
#19826=ORIENTED_EDGE('',*,*,#14205,.F.);
#19827=ORIENTED_EDGE('',*,*,#14206,.F.);
#19828=ORIENTED_EDGE('',*,*,#14207,.T.);
#19829=ORIENTED_EDGE('',*,*,#14203,.T.);
#19830=ORIENTED_EDGE('',*,*,#14208,.F.);
#19831=ORIENTED_EDGE('',*,*,#14209,.F.);
#19832=ORIENTED_EDGE('',*,*,#14210,.T.);
#19833=ORIENTED_EDGE('',*,*,#14206,.T.);
#19834=ORIENTED_EDGE('',*,*,#14211,.F.);
#19835=ORIENTED_EDGE('',*,*,#14212,.F.);
#19836=ORIENTED_EDGE('',*,*,#14213,.T.);
#19837=ORIENTED_EDGE('',*,*,#14209,.T.);
#19838=ORIENTED_EDGE('',*,*,#14214,.F.);
#19839=ORIENTED_EDGE('',*,*,#14215,.F.);
#19840=ORIENTED_EDGE('',*,*,#14216,.T.);
#19841=ORIENTED_EDGE('',*,*,#14212,.T.);
#19842=ORIENTED_EDGE('',*,*,#14217,.F.);
#19843=ORIENTED_EDGE('',*,*,#14218,.F.);
#19844=ORIENTED_EDGE('',*,*,#14219,.T.);
#19845=ORIENTED_EDGE('',*,*,#14215,.T.);
#19846=ORIENTED_EDGE('',*,*,#14220,.F.);
#19847=ORIENTED_EDGE('',*,*,#14045,.T.);
#19848=ORIENTED_EDGE('',*,*,#14221,.T.);
#19849=ORIENTED_EDGE('',*,*,#14222,.F.);
#19850=ORIENTED_EDGE('',*,*,#14223,.F.);
#19851=ORIENTED_EDGE('',*,*,#14224,.T.);
#19852=ORIENTED_EDGE('',*,*,#14224,.F.);
#19853=ORIENTED_EDGE('',*,*,#14225,.F.);
#19854=ORIENTED_EDGE('',*,*,#14042,.F.);
#19855=ORIENTED_EDGE('',*,*,#14039,.F.);
#19856=ORIENTED_EDGE('',*,*,#14036,.F.);
#19857=ORIENTED_EDGE('',*,*,#14033,.F.);
#19858=ORIENTED_EDGE('',*,*,#14030,.F.);
#19859=ORIENTED_EDGE('',*,*,#14027,.F.);
#19860=ORIENTED_EDGE('',*,*,#14024,.F.);
#19861=ORIENTED_EDGE('',*,*,#14021,.F.);
#19862=ORIENTED_EDGE('',*,*,#14018,.F.);
#19863=ORIENTED_EDGE('',*,*,#14015,.F.);
#19864=ORIENTED_EDGE('',*,*,#14012,.F.);
#19865=ORIENTED_EDGE('',*,*,#14009,.F.);
#19866=ORIENTED_EDGE('',*,*,#14006,.F.);
#19867=ORIENTED_EDGE('',*,*,#14003,.F.);
#19868=ORIENTED_EDGE('',*,*,#14000,.F.);
#19869=ORIENTED_EDGE('',*,*,#13997,.F.);
#19870=ORIENTED_EDGE('',*,*,#13994,.F.);
#19871=ORIENTED_EDGE('',*,*,#13991,.F.);
#19872=ORIENTED_EDGE('',*,*,#13988,.F.);
#19873=ORIENTED_EDGE('',*,*,#13985,.F.);
#19874=ORIENTED_EDGE('',*,*,#13982,.F.);
#19875=ORIENTED_EDGE('',*,*,#13979,.F.);
#19876=ORIENTED_EDGE('',*,*,#13976,.F.);
#19877=ORIENTED_EDGE('',*,*,#13973,.F.);
#19878=ORIENTED_EDGE('',*,*,#13970,.F.);
#19879=ORIENTED_EDGE('',*,*,#13967,.F.);
#19880=ORIENTED_EDGE('',*,*,#13964,.F.);
#19881=ORIENTED_EDGE('',*,*,#13961,.F.);
#19882=ORIENTED_EDGE('',*,*,#13958,.F.);
#19883=ORIENTED_EDGE('',*,*,#13955,.F.);
#19884=ORIENTED_EDGE('',*,*,#13952,.F.);
#19885=ORIENTED_EDGE('',*,*,#13949,.F.);
#19886=ORIENTED_EDGE('',*,*,#13946,.F.);
#19887=ORIENTED_EDGE('',*,*,#13943,.F.);
#19888=ORIENTED_EDGE('',*,*,#13940,.F.);
#19889=ORIENTED_EDGE('',*,*,#13937,.F.);
#19890=ORIENTED_EDGE('',*,*,#13934,.F.);
#19891=ORIENTED_EDGE('',*,*,#13931,.F.);
#19892=ORIENTED_EDGE('',*,*,#13928,.F.);
#19893=ORIENTED_EDGE('',*,*,#13925,.F.);
#19894=ORIENTED_EDGE('',*,*,#13922,.F.);
#19895=ORIENTED_EDGE('',*,*,#13919,.F.);
#19896=ORIENTED_EDGE('',*,*,#13916,.F.);
#19897=ORIENTED_EDGE('',*,*,#13913,.F.);
#19898=ORIENTED_EDGE('',*,*,#13910,.F.);
#19899=ORIENTED_EDGE('',*,*,#13907,.F.);
#19900=ORIENTED_EDGE('',*,*,#13904,.F.);
#19901=ORIENTED_EDGE('',*,*,#13901,.F.);
#19902=ORIENTED_EDGE('',*,*,#13898,.F.);
#19903=ORIENTED_EDGE('',*,*,#13895,.F.);
#19904=ORIENTED_EDGE('',*,*,#13892,.F.);
#19905=ORIENTED_EDGE('',*,*,#13889,.F.);
#19906=ORIENTED_EDGE('',*,*,#13886,.F.);
#19907=ORIENTED_EDGE('',*,*,#13883,.F.);
#19908=ORIENTED_EDGE('',*,*,#13880,.F.);
#19909=ORIENTED_EDGE('',*,*,#13877,.F.);
#19910=ORIENTED_EDGE('',*,*,#13874,.F.);
#19911=ORIENTED_EDGE('',*,*,#13871,.F.);
#19912=ORIENTED_EDGE('',*,*,#14226,.F.);
#19913=ORIENTED_EDGE('',*,*,#14227,.T.);
#19914=ORIENTED_EDGE('',*,*,#14220,.T.);
#19915=ORIENTED_EDGE('',*,*,#14217,.T.);
#19916=ORIENTED_EDGE('',*,*,#14214,.T.);
#19917=ORIENTED_EDGE('',*,*,#14211,.T.);
#19918=ORIENTED_EDGE('',*,*,#14208,.T.);
#19919=ORIENTED_EDGE('',*,*,#14205,.T.);
#19920=ORIENTED_EDGE('',*,*,#14202,.T.);
#19921=ORIENTED_EDGE('',*,*,#14199,.T.);
#19922=ORIENTED_EDGE('',*,*,#14196,.T.);
#19923=ORIENTED_EDGE('',*,*,#14193,.T.);
#19924=ORIENTED_EDGE('',*,*,#14190,.T.);
#19925=ORIENTED_EDGE('',*,*,#14187,.T.);
#19926=ORIENTED_EDGE('',*,*,#14184,.T.);
#19927=ORIENTED_EDGE('',*,*,#14181,.T.);
#19928=ORIENTED_EDGE('',*,*,#14178,.T.);
#19929=ORIENTED_EDGE('',*,*,#14175,.T.);
#19930=ORIENTED_EDGE('',*,*,#14172,.T.);
#19931=ORIENTED_EDGE('',*,*,#14169,.T.);
#19932=ORIENTED_EDGE('',*,*,#14166,.T.);
#19933=ORIENTED_EDGE('',*,*,#14163,.T.);
#19934=ORIENTED_EDGE('',*,*,#14160,.T.);
#19935=ORIENTED_EDGE('',*,*,#14157,.T.);
#19936=ORIENTED_EDGE('',*,*,#14154,.T.);
#19937=ORIENTED_EDGE('',*,*,#14151,.T.);
#19938=ORIENTED_EDGE('',*,*,#14148,.T.);
#19939=ORIENTED_EDGE('',*,*,#14145,.T.);
#19940=ORIENTED_EDGE('',*,*,#14142,.T.);
#19941=ORIENTED_EDGE('',*,*,#14139,.T.);
#19942=ORIENTED_EDGE('',*,*,#14136,.T.);
#19943=ORIENTED_EDGE('',*,*,#14133,.T.);
#19944=ORIENTED_EDGE('',*,*,#14130,.T.);
#19945=ORIENTED_EDGE('',*,*,#14127,.T.);
#19946=ORIENTED_EDGE('',*,*,#14124,.T.);
#19947=ORIENTED_EDGE('',*,*,#14121,.T.);
#19948=ORIENTED_EDGE('',*,*,#14118,.T.);
#19949=ORIENTED_EDGE('',*,*,#14115,.T.);
#19950=ORIENTED_EDGE('',*,*,#14112,.T.);
#19951=ORIENTED_EDGE('',*,*,#14109,.T.);
#19952=ORIENTED_EDGE('',*,*,#14106,.T.);
#19953=ORIENTED_EDGE('',*,*,#14103,.T.);
#19954=ORIENTED_EDGE('',*,*,#14100,.T.);
#19955=ORIENTED_EDGE('',*,*,#14097,.T.);
#19956=ORIENTED_EDGE('',*,*,#14094,.T.);
#19957=ORIENTED_EDGE('',*,*,#14091,.T.);
#19958=ORIENTED_EDGE('',*,*,#14088,.T.);
#19959=ORIENTED_EDGE('',*,*,#14085,.T.);
#19960=ORIENTED_EDGE('',*,*,#14082,.T.);
#19961=ORIENTED_EDGE('',*,*,#14079,.T.);
#19962=ORIENTED_EDGE('',*,*,#14076,.T.);
#19963=ORIENTED_EDGE('',*,*,#14073,.T.);
#19964=ORIENTED_EDGE('',*,*,#14070,.T.);
#19965=ORIENTED_EDGE('',*,*,#14067,.T.);
#19966=ORIENTED_EDGE('',*,*,#14064,.T.);
#19967=ORIENTED_EDGE('',*,*,#14061,.T.);
#19968=ORIENTED_EDGE('',*,*,#14058,.T.);
#19969=ORIENTED_EDGE('',*,*,#14055,.T.);
#19970=ORIENTED_EDGE('',*,*,#14052,.T.);
#19971=ORIENTED_EDGE('',*,*,#14049,.T.);
#19972=ORIENTED_EDGE('',*,*,#14046,.T.);
#19973=ORIENTED_EDGE('',*,*,#13867,.F.);
#19974=ORIENTED_EDGE('',*,*,#14228,.T.);
#19975=ORIENTED_EDGE('',*,*,#14229,.T.);
#19976=ORIENTED_EDGE('',*,*,#14226,.T.);
#19977=ORIENTED_EDGE('',*,*,#13870,.F.);
#19978=ORIENTED_EDGE('',*,*,#14218,.T.);
#19979=ORIENTED_EDGE('',*,*,#14227,.F.);
#19980=ORIENTED_EDGE('',*,*,#14229,.F.);
#19981=ORIENTED_EDGE('',*,*,#14230,.T.);
#19982=ORIENTED_EDGE('',*,*,#14221,.F.);
#19983=ORIENTED_EDGE('',*,*,#14044,.F.);
#19984=ORIENTED_EDGE('',*,*,#14048,.F.);
#19985=ORIENTED_EDGE('',*,*,#14051,.F.);
#19986=ORIENTED_EDGE('',*,*,#14054,.F.);
#19987=ORIENTED_EDGE('',*,*,#14057,.F.);
#19988=ORIENTED_EDGE('',*,*,#14060,.F.);
#19989=ORIENTED_EDGE('',*,*,#14063,.F.);
#19990=ORIENTED_EDGE('',*,*,#14066,.F.);
#19991=ORIENTED_EDGE('',*,*,#14069,.F.);
#19992=ORIENTED_EDGE('',*,*,#14072,.F.);
#19993=ORIENTED_EDGE('',*,*,#14075,.F.);
#19994=ORIENTED_EDGE('',*,*,#14078,.F.);
#19995=ORIENTED_EDGE('',*,*,#14081,.F.);
#19996=ORIENTED_EDGE('',*,*,#14084,.F.);
#19997=ORIENTED_EDGE('',*,*,#14087,.F.);
#19998=ORIENTED_EDGE('',*,*,#14090,.F.);
#19999=ORIENTED_EDGE('',*,*,#14093,.F.);
#20000=ORIENTED_EDGE('',*,*,#14096,.F.);
#20001=ORIENTED_EDGE('',*,*,#14099,.F.);
#20002=ORIENTED_EDGE('',*,*,#14102,.F.);
#20003=ORIENTED_EDGE('',*,*,#14105,.F.);
#20004=ORIENTED_EDGE('',*,*,#14108,.F.);
#20005=ORIENTED_EDGE('',*,*,#14111,.F.);
#20006=ORIENTED_EDGE('',*,*,#14114,.F.);
#20007=ORIENTED_EDGE('',*,*,#14117,.F.);
#20008=ORIENTED_EDGE('',*,*,#14120,.F.);
#20009=ORIENTED_EDGE('',*,*,#14123,.F.);
#20010=ORIENTED_EDGE('',*,*,#14126,.F.);
#20011=ORIENTED_EDGE('',*,*,#14129,.F.);
#20012=ORIENTED_EDGE('',*,*,#14132,.F.);
#20013=ORIENTED_EDGE('',*,*,#14135,.F.);
#20014=ORIENTED_EDGE('',*,*,#14138,.F.);
#20015=ORIENTED_EDGE('',*,*,#14141,.F.);
#20016=ORIENTED_EDGE('',*,*,#14144,.F.);
#20017=ORIENTED_EDGE('',*,*,#14147,.F.);
#20018=ORIENTED_EDGE('',*,*,#14150,.F.);
#20019=ORIENTED_EDGE('',*,*,#14153,.F.);
#20020=ORIENTED_EDGE('',*,*,#14156,.F.);
#20021=ORIENTED_EDGE('',*,*,#14159,.F.);
#20022=ORIENTED_EDGE('',*,*,#14162,.F.);
#20023=ORIENTED_EDGE('',*,*,#14165,.F.);
#20024=ORIENTED_EDGE('',*,*,#14168,.F.);
#20025=ORIENTED_EDGE('',*,*,#14171,.F.);
#20026=ORIENTED_EDGE('',*,*,#14174,.F.);
#20027=ORIENTED_EDGE('',*,*,#14177,.F.);
#20028=ORIENTED_EDGE('',*,*,#14180,.F.);
#20029=ORIENTED_EDGE('',*,*,#14183,.F.);
#20030=ORIENTED_EDGE('',*,*,#14186,.F.);
#20031=ORIENTED_EDGE('',*,*,#14189,.F.);
#20032=ORIENTED_EDGE('',*,*,#14192,.F.);
#20033=ORIENTED_EDGE('',*,*,#14195,.F.);
#20034=ORIENTED_EDGE('',*,*,#14198,.F.);
#20035=ORIENTED_EDGE('',*,*,#14201,.F.);
#20036=ORIENTED_EDGE('',*,*,#14204,.F.);
#20037=ORIENTED_EDGE('',*,*,#14207,.F.);
#20038=ORIENTED_EDGE('',*,*,#14210,.F.);
#20039=ORIENTED_EDGE('',*,*,#14213,.F.);
#20040=ORIENTED_EDGE('',*,*,#14216,.F.);
#20041=ORIENTED_EDGE('',*,*,#14219,.F.);
#20042=ORIENTED_EDGE('',*,*,#14230,.F.);
#20043=ORIENTED_EDGE('',*,*,#14228,.F.);
#20044=ORIENTED_EDGE('',*,*,#13866,.F.);
#20045=ORIENTED_EDGE('',*,*,#13873,.F.);
#20046=ORIENTED_EDGE('',*,*,#13876,.F.);
#20047=ORIENTED_EDGE('',*,*,#13879,.F.);
#20048=ORIENTED_EDGE('',*,*,#13882,.F.);
#20049=ORIENTED_EDGE('',*,*,#13885,.F.);
#20050=ORIENTED_EDGE('',*,*,#13888,.F.);
#20051=ORIENTED_EDGE('',*,*,#13891,.F.);
#20052=ORIENTED_EDGE('',*,*,#13894,.F.);
#20053=ORIENTED_EDGE('',*,*,#13897,.F.);
#20054=ORIENTED_EDGE('',*,*,#13900,.F.);
#20055=ORIENTED_EDGE('',*,*,#13903,.F.);
#20056=ORIENTED_EDGE('',*,*,#13906,.F.);
#20057=ORIENTED_EDGE('',*,*,#13909,.F.);
#20058=ORIENTED_EDGE('',*,*,#13912,.F.);
#20059=ORIENTED_EDGE('',*,*,#13915,.F.);
#20060=ORIENTED_EDGE('',*,*,#13918,.F.);
#20061=ORIENTED_EDGE('',*,*,#13921,.F.);
#20062=ORIENTED_EDGE('',*,*,#13924,.F.);
#20063=ORIENTED_EDGE('',*,*,#13927,.F.);
#20064=ORIENTED_EDGE('',*,*,#13930,.F.);
#20065=ORIENTED_EDGE('',*,*,#13933,.F.);
#20066=ORIENTED_EDGE('',*,*,#13936,.F.);
#20067=ORIENTED_EDGE('',*,*,#13939,.F.);
#20068=ORIENTED_EDGE('',*,*,#13942,.F.);
#20069=ORIENTED_EDGE('',*,*,#13945,.F.);
#20070=ORIENTED_EDGE('',*,*,#13948,.F.);
#20071=ORIENTED_EDGE('',*,*,#13951,.F.);
#20072=ORIENTED_EDGE('',*,*,#13954,.F.);
#20073=ORIENTED_EDGE('',*,*,#13957,.F.);
#20074=ORIENTED_EDGE('',*,*,#13960,.F.);
#20075=ORIENTED_EDGE('',*,*,#13963,.F.);
#20076=ORIENTED_EDGE('',*,*,#13966,.F.);
#20077=ORIENTED_EDGE('',*,*,#13969,.F.);
#20078=ORIENTED_EDGE('',*,*,#13972,.F.);
#20079=ORIENTED_EDGE('',*,*,#13975,.F.);
#20080=ORIENTED_EDGE('',*,*,#13978,.F.);
#20081=ORIENTED_EDGE('',*,*,#13981,.F.);
#20082=ORIENTED_EDGE('',*,*,#13984,.F.);
#20083=ORIENTED_EDGE('',*,*,#13987,.F.);
#20084=ORIENTED_EDGE('',*,*,#13990,.F.);
#20085=ORIENTED_EDGE('',*,*,#13993,.F.);
#20086=ORIENTED_EDGE('',*,*,#13996,.F.);
#20087=ORIENTED_EDGE('',*,*,#13999,.F.);
#20088=ORIENTED_EDGE('',*,*,#14002,.F.);
#20089=ORIENTED_EDGE('',*,*,#14005,.F.);
#20090=ORIENTED_EDGE('',*,*,#14008,.F.);
#20091=ORIENTED_EDGE('',*,*,#14011,.F.);
#20092=ORIENTED_EDGE('',*,*,#14014,.F.);
#20093=ORIENTED_EDGE('',*,*,#14017,.F.);
#20094=ORIENTED_EDGE('',*,*,#14020,.F.);
#20095=ORIENTED_EDGE('',*,*,#14023,.F.);
#20096=ORIENTED_EDGE('',*,*,#14026,.F.);
#20097=ORIENTED_EDGE('',*,*,#14029,.F.);
#20098=ORIENTED_EDGE('',*,*,#14032,.F.);
#20099=ORIENTED_EDGE('',*,*,#14035,.F.);
#20100=ORIENTED_EDGE('',*,*,#14038,.F.);
#20101=ORIENTED_EDGE('',*,*,#14041,.F.);
#20102=ORIENTED_EDGE('',*,*,#14231,.F.);
#20103=ORIENTED_EDGE('',*,*,#14232,.F.);
#20104=ORIENTED_EDGE('',*,*,#14233,.T.);
#20105=ORIENTED_EDGE('',*,*,#14234,.T.);
#20106=ORIENTED_EDGE('',*,*,#14235,.F.);
#20107=ORIENTED_EDGE('',*,*,#14234,.F.);
#20108=ORIENTED_EDGE('',*,*,#14236,.T.);
#20109=ORIENTED_EDGE('',*,*,#14237,.F.);
#20110=ORIENTED_EDGE('',*,*,#14238,.F.);
#20111=ORIENTED_EDGE('',*,*,#14239,.F.);
#20112=ORIENTED_EDGE('',*,*,#14236,.F.);
#20113=ORIENTED_EDGE('',*,*,#14233,.F.);
#20114=ORIENTED_EDGE('',*,*,#14240,.F.);
#20115=ORIENTED_EDGE('',*,*,#14241,.T.);
#20116=ORIENTED_EDGE('',*,*,#14242,.T.);
#20117=ORIENTED_EDGE('',*,*,#14243,.F.);
#20118=ORIENTED_EDGE('',*,*,#14242,.F.);
#20119=ORIENTED_EDGE('',*,*,#14244,.T.);
#20120=ORIENTED_EDGE('',*,*,#14245,.F.);
#20121=ORIENTED_EDGE('',*,*,#14246,.F.);
#20122=ORIENTED_EDGE('',*,*,#14247,.F.);
#20123=ORIENTED_EDGE('',*,*,#14244,.F.);
#20124=ORIENTED_EDGE('',*,*,#14241,.F.);
#20125=ORIENTED_EDGE('',*,*,#14248,.F.);
#20126=ORIENTED_EDGE('',*,*,#14249,.T.);
#20127=ORIENTED_EDGE('',*,*,#14250,.T.);
#20128=ORIENTED_EDGE('',*,*,#14251,.F.);
#20129=ORIENTED_EDGE('',*,*,#14250,.F.);
#20130=ORIENTED_EDGE('',*,*,#14252,.T.);
#20131=ORIENTED_EDGE('',*,*,#14253,.F.);
#20132=ORIENTED_EDGE('',*,*,#14254,.F.);
#20133=ORIENTED_EDGE('',*,*,#14255,.F.);
#20134=ORIENTED_EDGE('',*,*,#14252,.F.);
#20135=ORIENTED_EDGE('',*,*,#14249,.F.);
#20136=ORIENTED_EDGE('',*,*,#14256,.F.);
#20137=ORIENTED_EDGE('',*,*,#14257,.T.);
#20138=ORIENTED_EDGE('',*,*,#14258,.T.);
#20139=ORIENTED_EDGE('',*,*,#14259,.F.);
#20140=ORIENTED_EDGE('',*,*,#14258,.F.);
#20141=ORIENTED_EDGE('',*,*,#14260,.T.);
#20142=ORIENTED_EDGE('',*,*,#14261,.F.);
#20143=ORIENTED_EDGE('',*,*,#14262,.F.);
#20144=ORIENTED_EDGE('',*,*,#14263,.F.);
#20145=ORIENTED_EDGE('',*,*,#14260,.F.);
#20146=ORIENTED_EDGE('',*,*,#14257,.F.);
#20147=ORIENTED_EDGE('',*,*,#14264,.F.);
#20148=ORIENTED_EDGE('',*,*,#14265,.T.);
#20149=ORIENTED_EDGE('',*,*,#14266,.T.);
#20150=ORIENTED_EDGE('',*,*,#14267,.F.);
#20151=ORIENTED_EDGE('',*,*,#14266,.F.);
#20152=ORIENTED_EDGE('',*,*,#14268,.T.);
#20153=ORIENTED_EDGE('',*,*,#14269,.F.);
#20154=ORIENTED_EDGE('',*,*,#14270,.F.);
#20155=ORIENTED_EDGE('',*,*,#14271,.F.);
#20156=ORIENTED_EDGE('',*,*,#14268,.F.);
#20157=ORIENTED_EDGE('',*,*,#14265,.F.);
#20158=ORIENTED_EDGE('',*,*,#14272,.F.);
#20159=ORIENTED_EDGE('',*,*,#14273,.T.);
#20160=ORIENTED_EDGE('',*,*,#14274,.T.);
#20161=ORIENTED_EDGE('',*,*,#14275,.F.);
#20162=ORIENTED_EDGE('',*,*,#14274,.F.);
#20163=ORIENTED_EDGE('',*,*,#14276,.T.);
#20164=ORIENTED_EDGE('',*,*,#14277,.F.);
#20165=ORIENTED_EDGE('',*,*,#14278,.F.);
#20166=ORIENTED_EDGE('',*,*,#14279,.F.);
#20167=ORIENTED_EDGE('',*,*,#14276,.F.);
#20168=ORIENTED_EDGE('',*,*,#14273,.F.);
#20169=ORIENTED_EDGE('',*,*,#14280,.F.);
#20170=ORIENTED_EDGE('',*,*,#14281,.T.);
#20171=ORIENTED_EDGE('',*,*,#14282,.T.);
#20172=ORIENTED_EDGE('',*,*,#14283,.F.);
#20173=ORIENTED_EDGE('',*,*,#14282,.F.);
#20174=ORIENTED_EDGE('',*,*,#14284,.T.);
#20175=ORIENTED_EDGE('',*,*,#14285,.F.);
#20176=ORIENTED_EDGE('',*,*,#14286,.F.);
#20177=ORIENTED_EDGE('',*,*,#14287,.F.);
#20178=ORIENTED_EDGE('',*,*,#14284,.F.);
#20179=ORIENTED_EDGE('',*,*,#14281,.F.);
#20180=ORIENTED_EDGE('',*,*,#14288,.F.);
#20181=ORIENTED_EDGE('',*,*,#14289,.T.);
#20182=ORIENTED_EDGE('',*,*,#14290,.T.);
#20183=ORIENTED_EDGE('',*,*,#14291,.F.);
#20184=ORIENTED_EDGE('',*,*,#14290,.F.);
#20185=ORIENTED_EDGE('',*,*,#14292,.T.);
#20186=ORIENTED_EDGE('',*,*,#14293,.F.);
#20187=ORIENTED_EDGE('',*,*,#14294,.F.);
#20188=ORIENTED_EDGE('',*,*,#14295,.F.);
#20189=ORIENTED_EDGE('',*,*,#14292,.F.);
#20190=ORIENTED_EDGE('',*,*,#14289,.F.);
#20191=ORIENTED_EDGE('',*,*,#14296,.F.);
#20192=ORIENTED_EDGE('',*,*,#14297,.T.);
#20193=ORIENTED_EDGE('',*,*,#14298,.T.);
#20194=ORIENTED_EDGE('',*,*,#14299,.F.);
#20195=ORIENTED_EDGE('',*,*,#14298,.F.);
#20196=ORIENTED_EDGE('',*,*,#14300,.T.);
#20197=ORIENTED_EDGE('',*,*,#14301,.F.);
#20198=ORIENTED_EDGE('',*,*,#14302,.F.);
#20199=ORIENTED_EDGE('',*,*,#14303,.F.);
#20200=ORIENTED_EDGE('',*,*,#14300,.F.);
#20201=ORIENTED_EDGE('',*,*,#14297,.F.);
#20202=ORIENTED_EDGE('',*,*,#14304,.F.);
#20203=ORIENTED_EDGE('',*,*,#14305,.T.);
#20204=ORIENTED_EDGE('',*,*,#14306,.T.);
#20205=ORIENTED_EDGE('',*,*,#14307,.F.);
#20206=ORIENTED_EDGE('',*,*,#14306,.F.);
#20207=ORIENTED_EDGE('',*,*,#14308,.T.);
#20208=ORIENTED_EDGE('',*,*,#14309,.F.);
#20209=ORIENTED_EDGE('',*,*,#14310,.F.);
#20210=ORIENTED_EDGE('',*,*,#14311,.F.);
#20211=ORIENTED_EDGE('',*,*,#14308,.F.);
#20212=ORIENTED_EDGE('',*,*,#14305,.F.);
#20213=ORIENTED_EDGE('',*,*,#14312,.F.);
#20214=ORIENTED_EDGE('',*,*,#14313,.T.);
#20215=ORIENTED_EDGE('',*,*,#14314,.T.);
#20216=ORIENTED_EDGE('',*,*,#14315,.F.);
#20217=ORIENTED_EDGE('',*,*,#14314,.F.);
#20218=ORIENTED_EDGE('',*,*,#14316,.T.);
#20219=ORIENTED_EDGE('',*,*,#14317,.F.);
#20220=ORIENTED_EDGE('',*,*,#14318,.F.);
#20221=ORIENTED_EDGE('',*,*,#14319,.F.);
#20222=ORIENTED_EDGE('',*,*,#14316,.F.);
#20223=ORIENTED_EDGE('',*,*,#14313,.F.);
#20224=ORIENTED_EDGE('',*,*,#14320,.F.);
#20225=ORIENTED_EDGE('',*,*,#14321,.T.);
#20226=ORIENTED_EDGE('',*,*,#14322,.T.);
#20227=ORIENTED_EDGE('',*,*,#14323,.F.);
#20228=ORIENTED_EDGE('',*,*,#14322,.F.);
#20229=ORIENTED_EDGE('',*,*,#14324,.T.);
#20230=ORIENTED_EDGE('',*,*,#14325,.F.);
#20231=ORIENTED_EDGE('',*,*,#14326,.F.);
#20232=ORIENTED_EDGE('',*,*,#14327,.F.);
#20233=ORIENTED_EDGE('',*,*,#14324,.F.);
#20234=ORIENTED_EDGE('',*,*,#14321,.F.);
#20235=ORIENTED_EDGE('',*,*,#14328,.F.);
#20236=ORIENTED_EDGE('',*,*,#14329,.T.);
#20237=ORIENTED_EDGE('',*,*,#14330,.T.);
#20238=ORIENTED_EDGE('',*,*,#14331,.F.);
#20239=ORIENTED_EDGE('',*,*,#14330,.F.);
#20240=ORIENTED_EDGE('',*,*,#14332,.T.);
#20241=ORIENTED_EDGE('',*,*,#14333,.F.);
#20242=ORIENTED_EDGE('',*,*,#14334,.F.);
#20243=ORIENTED_EDGE('',*,*,#14335,.F.);
#20244=ORIENTED_EDGE('',*,*,#14332,.F.);
#20245=ORIENTED_EDGE('',*,*,#14329,.F.);
#20246=ORIENTED_EDGE('',*,*,#14336,.F.);
#20247=ORIENTED_EDGE('',*,*,#14337,.T.);
#20248=ORIENTED_EDGE('',*,*,#14338,.T.);
#20249=ORIENTED_EDGE('',*,*,#14339,.F.);
#20250=ORIENTED_EDGE('',*,*,#14338,.F.);
#20251=ORIENTED_EDGE('',*,*,#14340,.T.);
#20252=ORIENTED_EDGE('',*,*,#14341,.F.);
#20253=ORIENTED_EDGE('',*,*,#14342,.F.);
#20254=ORIENTED_EDGE('',*,*,#14343,.F.);
#20255=ORIENTED_EDGE('',*,*,#14340,.F.);
#20256=ORIENTED_EDGE('',*,*,#14337,.F.);
#20257=ORIENTED_EDGE('',*,*,#14344,.F.);
#20258=ORIENTED_EDGE('',*,*,#14345,.T.);
#20259=ORIENTED_EDGE('',*,*,#14346,.T.);
#20260=ORIENTED_EDGE('',*,*,#14347,.F.);
#20261=ORIENTED_EDGE('',*,*,#14346,.F.);
#20262=ORIENTED_EDGE('',*,*,#14348,.T.);
#20263=ORIENTED_EDGE('',*,*,#14349,.F.);
#20264=ORIENTED_EDGE('',*,*,#14350,.F.);
#20265=ORIENTED_EDGE('',*,*,#14351,.F.);
#20266=ORIENTED_EDGE('',*,*,#14348,.F.);
#20267=ORIENTED_EDGE('',*,*,#14345,.F.);
#20268=ORIENTED_EDGE('',*,*,#14352,.F.);
#20269=ORIENTED_EDGE('',*,*,#14353,.T.);
#20270=ORIENTED_EDGE('',*,*,#14354,.T.);
#20271=ORIENTED_EDGE('',*,*,#14355,.F.);
#20272=ORIENTED_EDGE('',*,*,#14354,.F.);
#20273=ORIENTED_EDGE('',*,*,#14356,.T.);
#20274=ORIENTED_EDGE('',*,*,#14357,.F.);
#20275=ORIENTED_EDGE('',*,*,#14358,.F.);
#20276=ORIENTED_EDGE('',*,*,#14359,.F.);
#20277=ORIENTED_EDGE('',*,*,#14356,.F.);
#20278=ORIENTED_EDGE('',*,*,#14353,.F.);
#20279=ORIENTED_EDGE('',*,*,#14360,.F.);
#20280=ORIENTED_EDGE('',*,*,#14361,.T.);
#20281=ORIENTED_EDGE('',*,*,#14362,.T.);
#20282=ORIENTED_EDGE('',*,*,#14363,.F.);
#20283=ORIENTED_EDGE('',*,*,#14362,.F.);
#20284=ORIENTED_EDGE('',*,*,#14364,.T.);
#20285=ORIENTED_EDGE('',*,*,#14365,.F.);
#20286=ORIENTED_EDGE('',*,*,#14366,.F.);
#20287=ORIENTED_EDGE('',*,*,#14367,.F.);
#20288=ORIENTED_EDGE('',*,*,#14364,.F.);
#20289=ORIENTED_EDGE('',*,*,#14361,.F.);
#20290=ORIENTED_EDGE('',*,*,#14368,.F.);
#20291=ORIENTED_EDGE('',*,*,#14369,.T.);
#20292=ORIENTED_EDGE('',*,*,#14370,.T.);
#20293=ORIENTED_EDGE('',*,*,#14371,.F.);
#20294=ORIENTED_EDGE('',*,*,#14372,.F.);
#20295=ORIENTED_EDGE('',*,*,#14370,.F.);
#20296=ORIENTED_EDGE('',*,*,#14373,.T.);
#20297=ORIENTED_EDGE('',*,*,#14374,.F.);
#20298=ORIENTED_EDGE('',*,*,#14375,.F.);
#20299=ORIENTED_EDGE('',*,*,#14376,.F.);
#20300=ORIENTED_EDGE('',*,*,#14373,.F.);
#20301=ORIENTED_EDGE('',*,*,#14369,.F.);
#20302=ORIENTED_EDGE('',*,*,#14377,.F.);
#20303=ORIENTED_EDGE('',*,*,#14378,.T.);
#20304=ORIENTED_EDGE('',*,*,#14379,.T.);
#20305=ORIENTED_EDGE('',*,*,#14380,.F.);
#20306=ORIENTED_EDGE('',*,*,#14379,.F.);
#20307=ORIENTED_EDGE('',*,*,#14381,.T.);
#20308=ORIENTED_EDGE('',*,*,#14382,.F.);
#20309=ORIENTED_EDGE('',*,*,#14383,.F.);
#20310=ORIENTED_EDGE('',*,*,#14384,.F.);
#20311=ORIENTED_EDGE('',*,*,#14381,.F.);
#20312=ORIENTED_EDGE('',*,*,#14378,.F.);
#20313=ORIENTED_EDGE('',*,*,#14385,.F.);
#20314=ORIENTED_EDGE('',*,*,#14386,.T.);
#20315=ORIENTED_EDGE('',*,*,#14387,.T.);
#20316=ORIENTED_EDGE('',*,*,#14388,.F.);
#20317=ORIENTED_EDGE('',*,*,#14387,.F.);
#20318=ORIENTED_EDGE('',*,*,#14389,.T.);
#20319=ORIENTED_EDGE('',*,*,#14390,.F.);
#20320=ORIENTED_EDGE('',*,*,#14391,.F.);
#20321=ORIENTED_EDGE('',*,*,#14392,.F.);
#20322=ORIENTED_EDGE('',*,*,#14389,.F.);
#20323=ORIENTED_EDGE('',*,*,#14386,.F.);
#20324=ORIENTED_EDGE('',*,*,#14393,.F.);
#20325=ORIENTED_EDGE('',*,*,#14394,.T.);
#20326=ORIENTED_EDGE('',*,*,#14395,.T.);
#20327=ORIENTED_EDGE('',*,*,#14396,.F.);
#20328=ORIENTED_EDGE('',*,*,#14395,.F.);
#20329=ORIENTED_EDGE('',*,*,#14397,.T.);
#20330=ORIENTED_EDGE('',*,*,#14398,.F.);
#20331=ORIENTED_EDGE('',*,*,#14399,.F.);
#20332=ORIENTED_EDGE('',*,*,#14400,.F.);
#20333=ORIENTED_EDGE('',*,*,#14397,.F.);
#20334=ORIENTED_EDGE('',*,*,#14394,.F.);
#20335=ORIENTED_EDGE('',*,*,#14401,.F.);
#20336=ORIENTED_EDGE('',*,*,#14402,.T.);
#20337=ORIENTED_EDGE('',*,*,#14403,.T.);
#20338=ORIENTED_EDGE('',*,*,#14404,.F.);
#20339=ORIENTED_EDGE('',*,*,#14403,.F.);
#20340=ORIENTED_EDGE('',*,*,#14405,.T.);
#20341=ORIENTED_EDGE('',*,*,#14406,.F.);
#20342=ORIENTED_EDGE('',*,*,#14407,.F.);
#20343=ORIENTED_EDGE('',*,*,#14408,.F.);
#20344=ORIENTED_EDGE('',*,*,#14405,.F.);
#20345=ORIENTED_EDGE('',*,*,#14402,.F.);
#20346=ORIENTED_EDGE('',*,*,#14409,.F.);
#20347=ORIENTED_EDGE('',*,*,#14410,.T.);
#20348=ORIENTED_EDGE('',*,*,#14411,.T.);
#20349=ORIENTED_EDGE('',*,*,#14412,.F.);
#20350=ORIENTED_EDGE('',*,*,#14411,.F.);
#20351=ORIENTED_EDGE('',*,*,#14413,.T.);
#20352=ORIENTED_EDGE('',*,*,#14414,.F.);
#20353=ORIENTED_EDGE('',*,*,#14415,.F.);
#20354=ORIENTED_EDGE('',*,*,#14416,.F.);
#20355=ORIENTED_EDGE('',*,*,#14413,.F.);
#20356=ORIENTED_EDGE('',*,*,#14410,.F.);
#20357=ORIENTED_EDGE('',*,*,#14417,.F.);
#20358=ORIENTED_EDGE('',*,*,#14418,.T.);
#20359=ORIENTED_EDGE('',*,*,#14419,.T.);
#20360=ORIENTED_EDGE('',*,*,#14420,.F.);
#20361=ORIENTED_EDGE('',*,*,#14419,.F.);
#20362=ORIENTED_EDGE('',*,*,#14421,.T.);
#20363=ORIENTED_EDGE('',*,*,#14422,.F.);
#20364=ORIENTED_EDGE('',*,*,#14423,.F.);
#20365=ORIENTED_EDGE('',*,*,#14424,.F.);
#20366=ORIENTED_EDGE('',*,*,#14421,.F.);
#20367=ORIENTED_EDGE('',*,*,#14418,.F.);
#20368=ORIENTED_EDGE('',*,*,#14425,.F.);
#20369=ORIENTED_EDGE('',*,*,#14426,.T.);
#20370=ORIENTED_EDGE('',*,*,#14427,.T.);
#20371=ORIENTED_EDGE('',*,*,#14428,.F.);
#20372=ORIENTED_EDGE('',*,*,#14427,.F.);
#20373=ORIENTED_EDGE('',*,*,#14429,.T.);
#20374=ORIENTED_EDGE('',*,*,#14430,.F.);
#20375=ORIENTED_EDGE('',*,*,#14431,.F.);
#20376=ORIENTED_EDGE('',*,*,#14432,.F.);
#20377=ORIENTED_EDGE('',*,*,#14429,.F.);
#20378=ORIENTED_EDGE('',*,*,#14426,.F.);
#20379=ORIENTED_EDGE('',*,*,#14433,.F.);
#20380=ORIENTED_EDGE('',*,*,#14434,.T.);
#20381=ORIENTED_EDGE('',*,*,#14435,.T.);
#20382=ORIENTED_EDGE('',*,*,#14436,.F.);
#20383=ORIENTED_EDGE('',*,*,#14435,.F.);
#20384=ORIENTED_EDGE('',*,*,#14437,.T.);
#20385=ORIENTED_EDGE('',*,*,#14438,.F.);
#20386=ORIENTED_EDGE('',*,*,#14439,.F.);
#20387=ORIENTED_EDGE('',*,*,#14440,.F.);
#20388=ORIENTED_EDGE('',*,*,#14437,.F.);
#20389=ORIENTED_EDGE('',*,*,#14434,.F.);
#20390=ORIENTED_EDGE('',*,*,#14441,.F.);
#20391=ORIENTED_EDGE('',*,*,#14442,.T.);
#20392=ORIENTED_EDGE('',*,*,#14443,.T.);
#20393=ORIENTED_EDGE('',*,*,#14444,.F.);
#20394=ORIENTED_EDGE('',*,*,#14443,.F.);
#20395=ORIENTED_EDGE('',*,*,#14445,.T.);
#20396=ORIENTED_EDGE('',*,*,#14446,.F.);
#20397=ORIENTED_EDGE('',*,*,#14447,.F.);
#20398=ORIENTED_EDGE('',*,*,#14448,.F.);
#20399=ORIENTED_EDGE('',*,*,#14445,.F.);
#20400=ORIENTED_EDGE('',*,*,#14442,.F.);
#20401=ORIENTED_EDGE('',*,*,#14449,.F.);
#20402=ORIENTED_EDGE('',*,*,#14450,.T.);
#20403=ORIENTED_EDGE('',*,*,#14451,.T.);
#20404=ORIENTED_EDGE('',*,*,#14452,.F.);
#20405=ORIENTED_EDGE('',*,*,#14451,.F.);
#20406=ORIENTED_EDGE('',*,*,#14453,.T.);
#20407=ORIENTED_EDGE('',*,*,#14454,.F.);
#20408=ORIENTED_EDGE('',*,*,#14455,.F.);
#20409=ORIENTED_EDGE('',*,*,#14456,.F.);
#20410=ORIENTED_EDGE('',*,*,#14453,.F.);
#20411=ORIENTED_EDGE('',*,*,#14450,.F.);
#20412=ORIENTED_EDGE('',*,*,#14457,.F.);
#20413=ORIENTED_EDGE('',*,*,#14458,.T.);
#20414=ORIENTED_EDGE('',*,*,#14459,.T.);
#20415=ORIENTED_EDGE('',*,*,#14460,.F.);
#20416=ORIENTED_EDGE('',*,*,#14459,.F.);
#20417=ORIENTED_EDGE('',*,*,#14461,.T.);
#20418=ORIENTED_EDGE('',*,*,#14462,.F.);
#20419=ORIENTED_EDGE('',*,*,#14463,.F.);
#20420=ORIENTED_EDGE('',*,*,#14464,.F.);
#20421=ORIENTED_EDGE('',*,*,#14461,.F.);
#20422=ORIENTED_EDGE('',*,*,#14458,.F.);
#20423=ORIENTED_EDGE('',*,*,#14465,.F.);
#20424=ORIENTED_EDGE('',*,*,#14466,.T.);
#20425=ORIENTED_EDGE('',*,*,#14467,.T.);
#20426=ORIENTED_EDGE('',*,*,#14468,.F.);
#20427=ORIENTED_EDGE('',*,*,#14467,.F.);
#20428=ORIENTED_EDGE('',*,*,#14469,.T.);
#20429=ORIENTED_EDGE('',*,*,#14470,.F.);
#20430=ORIENTED_EDGE('',*,*,#14471,.F.);
#20431=ORIENTED_EDGE('',*,*,#14472,.F.);
#20432=ORIENTED_EDGE('',*,*,#14469,.F.);
#20433=ORIENTED_EDGE('',*,*,#14466,.F.);
#20434=ORIENTED_EDGE('',*,*,#14473,.F.);
#20435=ORIENTED_EDGE('',*,*,#14474,.T.);
#20436=ORIENTED_EDGE('',*,*,#14475,.T.);
#20437=ORIENTED_EDGE('',*,*,#14476,.F.);
#20438=ORIENTED_EDGE('',*,*,#14475,.F.);
#20439=ORIENTED_EDGE('',*,*,#14477,.T.);
#20440=ORIENTED_EDGE('',*,*,#14478,.F.);
#20441=ORIENTED_EDGE('',*,*,#14479,.F.);
#20442=ORIENTED_EDGE('',*,*,#14480,.F.);
#20443=ORIENTED_EDGE('',*,*,#14477,.F.);
#20444=ORIENTED_EDGE('',*,*,#14474,.F.);
#20445=ORIENTED_EDGE('',*,*,#14481,.F.);
#20446=ORIENTED_EDGE('',*,*,#14482,.T.);
#20447=ORIENTED_EDGE('',*,*,#14483,.T.);
#20448=ORIENTED_EDGE('',*,*,#14484,.F.);
#20449=ORIENTED_EDGE('',*,*,#14483,.F.);
#20450=ORIENTED_EDGE('',*,*,#14485,.T.);
#20451=ORIENTED_EDGE('',*,*,#14486,.F.);
#20452=ORIENTED_EDGE('',*,*,#14487,.F.);
#20453=ORIENTED_EDGE('',*,*,#14488,.F.);
#20454=ORIENTED_EDGE('',*,*,#14485,.F.);
#20455=ORIENTED_EDGE('',*,*,#14482,.F.);
#20456=ORIENTED_EDGE('',*,*,#14489,.F.);
#20457=ORIENTED_EDGE('',*,*,#14490,.T.);
#20458=ORIENTED_EDGE('',*,*,#14491,.T.);
#20459=ORIENTED_EDGE('',*,*,#14492,.F.);
#20460=ORIENTED_EDGE('',*,*,#14491,.F.);
#20461=ORIENTED_EDGE('',*,*,#14493,.T.);
#20462=ORIENTED_EDGE('',*,*,#14494,.F.);
#20463=ORIENTED_EDGE('',*,*,#14495,.F.);
#20464=ORIENTED_EDGE('',*,*,#14496,.F.);
#20465=ORIENTED_EDGE('',*,*,#14493,.F.);
#20466=ORIENTED_EDGE('',*,*,#14490,.F.);
#20467=ORIENTED_EDGE('',*,*,#14497,.F.);
#20468=ORIENTED_EDGE('',*,*,#14498,.T.);
#20469=ORIENTED_EDGE('',*,*,#14499,.T.);
#20470=ORIENTED_EDGE('',*,*,#14500,.F.);
#20471=ORIENTED_EDGE('',*,*,#14499,.F.);
#20472=ORIENTED_EDGE('',*,*,#14501,.T.);
#20473=ORIENTED_EDGE('',*,*,#14502,.F.);
#20474=ORIENTED_EDGE('',*,*,#14503,.F.);
#20475=ORIENTED_EDGE('',*,*,#14504,.F.);
#20476=ORIENTED_EDGE('',*,*,#14501,.F.);
#20477=ORIENTED_EDGE('',*,*,#14498,.F.);
#20478=ORIENTED_EDGE('',*,*,#14505,.F.);
#20479=ORIENTED_EDGE('',*,*,#14506,.T.);
#20480=ORIENTED_EDGE('',*,*,#14507,.T.);
#20481=ORIENTED_EDGE('',*,*,#14508,.F.);
#20482=ORIENTED_EDGE('',*,*,#14507,.F.);
#20483=ORIENTED_EDGE('',*,*,#14509,.T.);
#20484=ORIENTED_EDGE('',*,*,#14510,.F.);
#20485=ORIENTED_EDGE('',*,*,#14511,.F.);
#20486=ORIENTED_EDGE('',*,*,#14512,.F.);
#20487=ORIENTED_EDGE('',*,*,#14509,.F.);
#20488=ORIENTED_EDGE('',*,*,#14506,.F.);
#20489=ORIENTED_EDGE('',*,*,#14238,.T.);
#20490=ORIENTED_EDGE('',*,*,#14232,.T.);
#20491=ORIENTED_EDGE('',*,*,#14235,.T.);
#20492=ORIENTED_EDGE('',*,*,#14513,.F.);
#20493=ORIENTED_EDGE('',*,*,#14246,.T.);
#20494=ORIENTED_EDGE('',*,*,#14240,.T.);
#20495=ORIENTED_EDGE('',*,*,#14243,.T.);
#20496=ORIENTED_EDGE('',*,*,#14514,.F.);
#20497=ORIENTED_EDGE('',*,*,#14254,.T.);
#20498=ORIENTED_EDGE('',*,*,#14248,.T.);
#20499=ORIENTED_EDGE('',*,*,#14251,.T.);
#20500=ORIENTED_EDGE('',*,*,#14515,.F.);
#20501=ORIENTED_EDGE('',*,*,#14262,.T.);
#20502=ORIENTED_EDGE('',*,*,#14256,.T.);
#20503=ORIENTED_EDGE('',*,*,#14259,.T.);
#20504=ORIENTED_EDGE('',*,*,#14516,.F.);
#20505=ORIENTED_EDGE('',*,*,#14270,.T.);
#20506=ORIENTED_EDGE('',*,*,#14264,.T.);
#20507=ORIENTED_EDGE('',*,*,#14267,.T.);
#20508=ORIENTED_EDGE('',*,*,#14517,.F.);
#20509=ORIENTED_EDGE('',*,*,#14278,.T.);
#20510=ORIENTED_EDGE('',*,*,#14272,.T.);
#20511=ORIENTED_EDGE('',*,*,#14275,.T.);
#20512=ORIENTED_EDGE('',*,*,#14518,.F.);
#20513=ORIENTED_EDGE('',*,*,#14286,.T.);
#20514=ORIENTED_EDGE('',*,*,#14280,.T.);
#20515=ORIENTED_EDGE('',*,*,#14283,.T.);
#20516=ORIENTED_EDGE('',*,*,#14519,.F.);
#20517=ORIENTED_EDGE('',*,*,#14294,.T.);
#20518=ORIENTED_EDGE('',*,*,#14288,.T.);
#20519=ORIENTED_EDGE('',*,*,#14291,.T.);
#20520=ORIENTED_EDGE('',*,*,#14520,.F.);
#20521=ORIENTED_EDGE('',*,*,#14302,.T.);
#20522=ORIENTED_EDGE('',*,*,#14296,.T.);
#20523=ORIENTED_EDGE('',*,*,#14299,.T.);
#20524=ORIENTED_EDGE('',*,*,#14521,.F.);
#20525=ORIENTED_EDGE('',*,*,#14310,.T.);
#20526=ORIENTED_EDGE('',*,*,#14304,.T.);
#20527=ORIENTED_EDGE('',*,*,#14307,.T.);
#20528=ORIENTED_EDGE('',*,*,#14522,.F.);
#20529=ORIENTED_EDGE('',*,*,#14318,.T.);
#20530=ORIENTED_EDGE('',*,*,#14312,.T.);
#20531=ORIENTED_EDGE('',*,*,#14315,.T.);
#20532=ORIENTED_EDGE('',*,*,#14523,.F.);
#20533=ORIENTED_EDGE('',*,*,#14326,.T.);
#20534=ORIENTED_EDGE('',*,*,#14320,.T.);
#20535=ORIENTED_EDGE('',*,*,#14323,.T.);
#20536=ORIENTED_EDGE('',*,*,#14524,.F.);
#20537=ORIENTED_EDGE('',*,*,#14334,.T.);
#20538=ORIENTED_EDGE('',*,*,#14328,.T.);
#20539=ORIENTED_EDGE('',*,*,#14331,.T.);
#20540=ORIENTED_EDGE('',*,*,#14525,.F.);
#20541=ORIENTED_EDGE('',*,*,#14342,.T.);
#20542=ORIENTED_EDGE('',*,*,#14336,.T.);
#20543=ORIENTED_EDGE('',*,*,#14339,.T.);
#20544=ORIENTED_EDGE('',*,*,#14526,.F.);
#20545=ORIENTED_EDGE('',*,*,#14350,.T.);
#20546=ORIENTED_EDGE('',*,*,#14344,.T.);
#20547=ORIENTED_EDGE('',*,*,#14347,.T.);
#20548=ORIENTED_EDGE('',*,*,#14527,.F.);
#20549=ORIENTED_EDGE('',*,*,#14358,.T.);
#20550=ORIENTED_EDGE('',*,*,#14352,.T.);
#20551=ORIENTED_EDGE('',*,*,#14355,.T.);
#20552=ORIENTED_EDGE('',*,*,#14528,.F.);
#20553=ORIENTED_EDGE('',*,*,#14366,.T.);
#20554=ORIENTED_EDGE('',*,*,#14360,.T.);
#20555=ORIENTED_EDGE('',*,*,#14363,.T.);
#20556=ORIENTED_EDGE('',*,*,#14529,.F.);
#20557=ORIENTED_EDGE('',*,*,#14375,.T.);
#20558=ORIENTED_EDGE('',*,*,#14368,.T.);
#20559=ORIENTED_EDGE('',*,*,#14530,.T.);
#20560=ORIENTED_EDGE('',*,*,#14531,.T.);
#20561=ORIENTED_EDGE('',*,*,#14530,.F.);
#20562=ORIENTED_EDGE('',*,*,#14371,.T.);
#20563=ORIENTED_EDGE('',*,*,#14372,.T.);
#20564=ORIENTED_EDGE('',*,*,#14532,.F.);
#20565=ORIENTED_EDGE('',*,*,#14383,.T.);
#20566=ORIENTED_EDGE('',*,*,#14377,.T.);
#20567=ORIENTED_EDGE('',*,*,#14380,.T.);
#20568=ORIENTED_EDGE('',*,*,#14533,.F.);
#20569=ORIENTED_EDGE('',*,*,#14391,.T.);
#20570=ORIENTED_EDGE('',*,*,#14385,.T.);
#20571=ORIENTED_EDGE('',*,*,#14388,.T.);
#20572=ORIENTED_EDGE('',*,*,#14534,.F.);
#20573=ORIENTED_EDGE('',*,*,#14399,.T.);
#20574=ORIENTED_EDGE('',*,*,#14393,.T.);
#20575=ORIENTED_EDGE('',*,*,#14396,.T.);
#20576=ORIENTED_EDGE('',*,*,#14535,.F.);
#20577=ORIENTED_EDGE('',*,*,#14407,.T.);
#20578=ORIENTED_EDGE('',*,*,#14401,.T.);
#20579=ORIENTED_EDGE('',*,*,#14404,.T.);
#20580=ORIENTED_EDGE('',*,*,#14536,.F.);
#20581=ORIENTED_EDGE('',*,*,#14415,.T.);
#20582=ORIENTED_EDGE('',*,*,#14409,.T.);
#20583=ORIENTED_EDGE('',*,*,#14412,.T.);
#20584=ORIENTED_EDGE('',*,*,#14537,.F.);
#20585=ORIENTED_EDGE('',*,*,#14423,.T.);
#20586=ORIENTED_EDGE('',*,*,#14417,.T.);
#20587=ORIENTED_EDGE('',*,*,#14420,.T.);
#20588=ORIENTED_EDGE('',*,*,#14538,.F.);
#20589=ORIENTED_EDGE('',*,*,#14431,.T.);
#20590=ORIENTED_EDGE('',*,*,#14425,.T.);
#20591=ORIENTED_EDGE('',*,*,#14428,.T.);
#20592=ORIENTED_EDGE('',*,*,#14539,.F.);
#20593=ORIENTED_EDGE('',*,*,#14439,.T.);
#20594=ORIENTED_EDGE('',*,*,#14433,.T.);
#20595=ORIENTED_EDGE('',*,*,#14436,.T.);
#20596=ORIENTED_EDGE('',*,*,#14540,.F.);
#20597=ORIENTED_EDGE('',*,*,#14447,.T.);
#20598=ORIENTED_EDGE('',*,*,#14441,.T.);
#20599=ORIENTED_EDGE('',*,*,#14444,.T.);
#20600=ORIENTED_EDGE('',*,*,#14541,.F.);
#20601=ORIENTED_EDGE('',*,*,#14455,.T.);
#20602=ORIENTED_EDGE('',*,*,#14449,.T.);
#20603=ORIENTED_EDGE('',*,*,#14452,.T.);
#20604=ORIENTED_EDGE('',*,*,#14542,.F.);
#20605=ORIENTED_EDGE('',*,*,#14463,.T.);
#20606=ORIENTED_EDGE('',*,*,#14457,.T.);
#20607=ORIENTED_EDGE('',*,*,#14460,.T.);
#20608=ORIENTED_EDGE('',*,*,#14543,.F.);
#20609=ORIENTED_EDGE('',*,*,#14471,.T.);
#20610=ORIENTED_EDGE('',*,*,#14465,.T.);
#20611=ORIENTED_EDGE('',*,*,#14468,.T.);
#20612=ORIENTED_EDGE('',*,*,#14544,.F.);
#20613=ORIENTED_EDGE('',*,*,#14479,.T.);
#20614=ORIENTED_EDGE('',*,*,#14473,.T.);
#20615=ORIENTED_EDGE('',*,*,#14476,.T.);
#20616=ORIENTED_EDGE('',*,*,#14545,.F.);
#20617=ORIENTED_EDGE('',*,*,#14487,.T.);
#20618=ORIENTED_EDGE('',*,*,#14481,.T.);
#20619=ORIENTED_EDGE('',*,*,#14484,.T.);
#20620=ORIENTED_EDGE('',*,*,#14546,.F.);
#20621=ORIENTED_EDGE('',*,*,#14495,.T.);
#20622=ORIENTED_EDGE('',*,*,#14489,.T.);
#20623=ORIENTED_EDGE('',*,*,#14492,.T.);
#20624=ORIENTED_EDGE('',*,*,#14547,.F.);
#20625=ORIENTED_EDGE('',*,*,#14503,.T.);
#20626=ORIENTED_EDGE('',*,*,#14497,.T.);
#20627=ORIENTED_EDGE('',*,*,#14500,.T.);
#20628=ORIENTED_EDGE('',*,*,#14548,.F.);
#20629=ORIENTED_EDGE('',*,*,#14511,.T.);
#20630=ORIENTED_EDGE('',*,*,#14505,.T.);
#20631=ORIENTED_EDGE('',*,*,#14508,.T.);
#20632=ORIENTED_EDGE('',*,*,#14549,.F.);
#20633=ORIENTED_EDGE('',*,*,#14550,.T.);
#20634=ORIENTED_EDGE('',*,*,#14551,.T.);
#20635=ORIENTED_EDGE('',*,*,#14552,.T.);
#20636=ORIENTED_EDGE('',*,*,#14553,.F.);
#20637=ORIENTED_EDGE('',*,*,#14552,.F.);
#20638=ORIENTED_EDGE('',*,*,#14554,.F.);
#20639=ORIENTED_EDGE('',*,*,#14555,.T.);
#20640=ORIENTED_EDGE('',*,*,#14556,.F.);
#20641=ORIENTED_EDGE('',*,*,#14557,.F.);
#20642=ORIENTED_EDGE('',*,*,#14555,.F.);
#20643=ORIENTED_EDGE('',*,*,#14558,.F.);
#20644=ORIENTED_EDGE('',*,*,#14550,.F.);
#20645=ORIENTED_EDGE('',*,*,#14551,.F.);
#20646=ORIENTED_EDGE('',*,*,#14558,.T.);
#20647=ORIENTED_EDGE('',*,*,#14554,.T.);
#20648=ORIENTED_EDGE('',*,*,#14559,.F.);
#20649=ORIENTED_EDGE('',*,*,#14560,.T.);
#20650=ORIENTED_EDGE('',*,*,#14376,.T.);
#20651=ORIENTED_EDGE('',*,*,#14529,.T.);
#20652=ORIENTED_EDGE('',*,*,#14365,.T.);
#20653=ORIENTED_EDGE('',*,*,#14367,.T.);
#20654=ORIENTED_EDGE('',*,*,#14528,.T.);
#20655=ORIENTED_EDGE('',*,*,#14357,.T.);
#20656=ORIENTED_EDGE('',*,*,#14359,.T.);
#20657=ORIENTED_EDGE('',*,*,#14527,.T.);
#20658=ORIENTED_EDGE('',*,*,#14349,.T.);
#20659=ORIENTED_EDGE('',*,*,#14351,.T.);
#20660=ORIENTED_EDGE('',*,*,#14526,.T.);
#20661=ORIENTED_EDGE('',*,*,#14341,.T.);
#20662=ORIENTED_EDGE('',*,*,#14343,.T.);
#20663=ORIENTED_EDGE('',*,*,#14525,.T.);
#20664=ORIENTED_EDGE('',*,*,#14333,.T.);
#20665=ORIENTED_EDGE('',*,*,#14335,.T.);
#20666=ORIENTED_EDGE('',*,*,#14524,.T.);
#20667=ORIENTED_EDGE('',*,*,#14325,.T.);
#20668=ORIENTED_EDGE('',*,*,#14327,.T.);
#20669=ORIENTED_EDGE('',*,*,#14523,.T.);
#20670=ORIENTED_EDGE('',*,*,#14317,.T.);
#20671=ORIENTED_EDGE('',*,*,#14319,.T.);
#20672=ORIENTED_EDGE('',*,*,#14522,.T.);
#20673=ORIENTED_EDGE('',*,*,#14309,.T.);
#20674=ORIENTED_EDGE('',*,*,#14311,.T.);
#20675=ORIENTED_EDGE('',*,*,#14521,.T.);
#20676=ORIENTED_EDGE('',*,*,#14301,.T.);
#20677=ORIENTED_EDGE('',*,*,#14303,.T.);
#20678=ORIENTED_EDGE('',*,*,#14520,.T.);
#20679=ORIENTED_EDGE('',*,*,#14293,.T.);
#20680=ORIENTED_EDGE('',*,*,#14295,.T.);
#20681=ORIENTED_EDGE('',*,*,#14519,.T.);
#20682=ORIENTED_EDGE('',*,*,#14285,.T.);
#20683=ORIENTED_EDGE('',*,*,#14287,.T.);
#20684=ORIENTED_EDGE('',*,*,#14518,.T.);
#20685=ORIENTED_EDGE('',*,*,#14277,.T.);
#20686=ORIENTED_EDGE('',*,*,#14279,.T.);
#20687=ORIENTED_EDGE('',*,*,#14517,.T.);
#20688=ORIENTED_EDGE('',*,*,#14269,.T.);
#20689=ORIENTED_EDGE('',*,*,#14271,.T.);
#20690=ORIENTED_EDGE('',*,*,#14516,.T.);
#20691=ORIENTED_EDGE('',*,*,#14261,.T.);
#20692=ORIENTED_EDGE('',*,*,#14263,.T.);
#20693=ORIENTED_EDGE('',*,*,#14515,.T.);
#20694=ORIENTED_EDGE('',*,*,#14253,.T.);
#20695=ORIENTED_EDGE('',*,*,#14255,.T.);
#20696=ORIENTED_EDGE('',*,*,#14514,.T.);
#20697=ORIENTED_EDGE('',*,*,#14245,.T.);
#20698=ORIENTED_EDGE('',*,*,#14247,.T.);
#20699=ORIENTED_EDGE('',*,*,#14513,.T.);
#20700=ORIENTED_EDGE('',*,*,#14237,.T.);
#20701=ORIENTED_EDGE('',*,*,#14239,.T.);
#20702=ORIENTED_EDGE('',*,*,#14553,.T.);
#20703=ORIENTED_EDGE('',*,*,#14556,.T.);
#20704=ORIENTED_EDGE('',*,*,#14557,.T.);
#20705=ORIENTED_EDGE('',*,*,#14549,.T.);
#20706=ORIENTED_EDGE('',*,*,#14510,.T.);
#20707=ORIENTED_EDGE('',*,*,#14512,.T.);
#20708=ORIENTED_EDGE('',*,*,#14548,.T.);
#20709=ORIENTED_EDGE('',*,*,#14502,.T.);
#20710=ORIENTED_EDGE('',*,*,#14504,.T.);
#20711=ORIENTED_EDGE('',*,*,#14547,.T.);
#20712=ORIENTED_EDGE('',*,*,#14494,.T.);
#20713=ORIENTED_EDGE('',*,*,#14496,.T.);
#20714=ORIENTED_EDGE('',*,*,#14546,.T.);
#20715=ORIENTED_EDGE('',*,*,#14486,.T.);
#20716=ORIENTED_EDGE('',*,*,#14488,.T.);
#20717=ORIENTED_EDGE('',*,*,#14545,.T.);
#20718=ORIENTED_EDGE('',*,*,#14478,.T.);
#20719=ORIENTED_EDGE('',*,*,#14480,.T.);
#20720=ORIENTED_EDGE('',*,*,#14544,.T.);
#20721=ORIENTED_EDGE('',*,*,#14470,.T.);
#20722=ORIENTED_EDGE('',*,*,#14472,.T.);
#20723=ORIENTED_EDGE('',*,*,#14543,.T.);
#20724=ORIENTED_EDGE('',*,*,#14462,.T.);
#20725=ORIENTED_EDGE('',*,*,#14464,.T.);
#20726=ORIENTED_EDGE('',*,*,#14542,.T.);
#20727=ORIENTED_EDGE('',*,*,#14454,.T.);
#20728=ORIENTED_EDGE('',*,*,#14456,.T.);
#20729=ORIENTED_EDGE('',*,*,#14541,.T.);
#20730=ORIENTED_EDGE('',*,*,#14446,.T.);
#20731=ORIENTED_EDGE('',*,*,#14448,.T.);
#20732=ORIENTED_EDGE('',*,*,#14540,.T.);
#20733=ORIENTED_EDGE('',*,*,#14438,.T.);
#20734=ORIENTED_EDGE('',*,*,#14440,.T.);
#20735=ORIENTED_EDGE('',*,*,#14539,.T.);
#20736=ORIENTED_EDGE('',*,*,#14430,.T.);
#20737=ORIENTED_EDGE('',*,*,#14432,.T.);
#20738=ORIENTED_EDGE('',*,*,#14538,.T.);
#20739=ORIENTED_EDGE('',*,*,#14422,.T.);
#20740=ORIENTED_EDGE('',*,*,#14424,.T.);
#20741=ORIENTED_EDGE('',*,*,#14537,.T.);
#20742=ORIENTED_EDGE('',*,*,#14414,.T.);
#20743=ORIENTED_EDGE('',*,*,#14416,.T.);
#20744=ORIENTED_EDGE('',*,*,#14536,.T.);
#20745=ORIENTED_EDGE('',*,*,#14406,.T.);
#20746=ORIENTED_EDGE('',*,*,#14408,.T.);
#20747=ORIENTED_EDGE('',*,*,#14535,.T.);
#20748=ORIENTED_EDGE('',*,*,#14398,.T.);
#20749=ORIENTED_EDGE('',*,*,#14400,.T.);
#20750=ORIENTED_EDGE('',*,*,#14534,.T.);
#20751=ORIENTED_EDGE('',*,*,#14390,.T.);
#20752=ORIENTED_EDGE('',*,*,#14392,.T.);
#20753=ORIENTED_EDGE('',*,*,#14533,.T.);
#20754=ORIENTED_EDGE('',*,*,#14382,.T.);
#20755=ORIENTED_EDGE('',*,*,#14384,.T.);
#20756=ORIENTED_EDGE('',*,*,#14532,.T.);
#20757=ORIENTED_EDGE('',*,*,#14374,.T.);
#20758=ORIENTED_EDGE('',*,*,#14560,.F.);
#20759=ORIENTED_EDGE('',*,*,#14561,.T.);
#20760=ORIENTED_EDGE('',*,*,#14562,.F.);
#20761=ORIENTED_EDGE('',*,*,#14561,.F.);
#20762=ORIENTED_EDGE('',*,*,#14563,.F.);
#20763=ORIENTED_EDGE('',*,*,#14564,.T.);
#20764=ORIENTED_EDGE('',*,*,#14565,.T.);
#20765=ORIENTED_EDGE('',*,*,#14566,.F.);
#20766=ORIENTED_EDGE('',*,*,#14567,.F.);
#20767=ORIENTED_EDGE('',*,*,#14568,.T.);
#20768=ORIENTED_EDGE('',*,*,#14569,.T.);
#20769=ORIENTED_EDGE('',*,*,#14564,.F.);
#20770=ORIENTED_EDGE('',*,*,#14570,.F.);
#20771=ORIENTED_EDGE('',*,*,#14571,.T.);
#20772=ORIENTED_EDGE('',*,*,#14572,.T.);
#20773=ORIENTED_EDGE('',*,*,#14568,.F.);
#20774=ORIENTED_EDGE('',*,*,#14573,.F.);
#20775=ORIENTED_EDGE('',*,*,#14574,.T.);
#20776=ORIENTED_EDGE('',*,*,#14575,.T.);
#20777=ORIENTED_EDGE('',*,*,#14571,.F.);
#20778=ORIENTED_EDGE('',*,*,#14576,.F.);
#20779=ORIENTED_EDGE('',*,*,#14577,.T.);
#20780=ORIENTED_EDGE('',*,*,#14578,.T.);
#20781=ORIENTED_EDGE('',*,*,#14574,.F.);
#20782=ORIENTED_EDGE('',*,*,#14579,.F.);
#20783=ORIENTED_EDGE('',*,*,#14566,.T.);
#20784=ORIENTED_EDGE('',*,*,#14580,.T.);
#20785=ORIENTED_EDGE('',*,*,#14577,.F.);
#20786=ORIENTED_EDGE('',*,*,#14580,.F.);
#20787=ORIENTED_EDGE('',*,*,#14565,.F.);
#20788=ORIENTED_EDGE('',*,*,#14569,.F.);
#20789=ORIENTED_EDGE('',*,*,#14572,.F.);
#20790=ORIENTED_EDGE('',*,*,#14575,.F.);
#20791=ORIENTED_EDGE('',*,*,#14578,.F.);
#20792=ORIENTED_EDGE('',*,*,#14562,.T.);
#20793=ORIENTED_EDGE('',*,*,#14581,.F.);
#20794=ORIENTED_EDGE('',*,*,#13869,.F.);
#20795=ORIENTED_EDGE('',*,*,#14582,.T.);
#20796=ORIENTED_EDGE('',*,*,#14581,.T.);
#20797=ORIENTED_EDGE('',*,*,#14582,.F.);
#20798=ORIENTED_EDGE('',*,*,#14040,.T.);
#20799=ORIENTED_EDGE('',*,*,#14225,.T.);
#20800=ORIENTED_EDGE('',*,*,#14583,.F.);
#20801=ORIENTED_EDGE('',*,*,#14231,.T.);
#20802=ORIENTED_EDGE('',*,*,#14584,.F.);
#20803=ORIENTED_EDGE('',*,*,#14585,.T.);
#20804=ORIENTED_EDGE('',*,*,#14222,.T.);
#20805=ORIENTED_EDGE('',*,*,#14583,.T.);
#20806=ORIENTED_EDGE('',*,*,#14223,.T.);
#20807=ORIENTED_EDGE('',*,*,#14585,.F.);
#20808=ORIENTED_EDGE('',*,*,#14531,.F.);
#20809=ORIENTED_EDGE('',*,*,#14584,.T.);
#20810=ORIENTED_EDGE('',*,*,#14559,.T.);
#20811=ORIENTED_EDGE('',*,*,#14563,.T.);
#20812=ORIENTED_EDGE('',*,*,#14579,.T.);
#20813=ORIENTED_EDGE('',*,*,#14576,.T.);
#20814=ORIENTED_EDGE('',*,*,#14573,.T.);
#20815=ORIENTED_EDGE('',*,*,#14570,.T.);
#20816=ORIENTED_EDGE('',*,*,#14567,.T.);
#20817=ORIENTED_EDGE('',*,*,#14586,.F.);
#20818=ORIENTED_EDGE('',*,*,#14587,.T.);
#20819=ORIENTED_EDGE('',*,*,#14588,.T.);
#20820=ORIENTED_EDGE('',*,*,#14589,.T.);
#20821=ORIENTED_EDGE('',*,*,#14590,.T.);
#20822=ORIENTED_EDGE('',*,*,#14589,.F.);
#20823=ORIENTED_EDGE('',*,*,#14591,.T.);
#20824=ORIENTED_EDGE('',*,*,#14592,.T.);
#20825=ORIENTED_EDGE('',*,*,#14593,.F.);
#20826=ORIENTED_EDGE('',*,*,#14594,.T.);
#20827=ORIENTED_EDGE('',*,*,#14586,.T.);
#20828=ORIENTED_EDGE('',*,*,#14595,.T.);
#20829=ORIENTED_EDGE('',*,*,#14596,.F.);
#20830=ORIENTED_EDGE('',*,*,#14597,.T.);
#20831=ORIENTED_EDGE('',*,*,#14593,.T.);
#20832=ORIENTED_EDGE('',*,*,#14598,.T.);
#20833=ORIENTED_EDGE('',*,*,#14599,.F.);
#20834=ORIENTED_EDGE('',*,*,#14600,.T.);
#20835=ORIENTED_EDGE('',*,*,#14596,.T.);
#20836=ORIENTED_EDGE('',*,*,#14601,.T.);
#20837=ORIENTED_EDGE('',*,*,#14602,.F.);
#20838=ORIENTED_EDGE('',*,*,#14603,.T.);
#20839=ORIENTED_EDGE('',*,*,#14599,.T.);
#20840=ORIENTED_EDGE('',*,*,#14604,.T.);
#20841=ORIENTED_EDGE('',*,*,#14605,.F.);
#20842=ORIENTED_EDGE('',*,*,#14606,.T.);
#20843=ORIENTED_EDGE('',*,*,#14602,.T.);
#20844=ORIENTED_EDGE('',*,*,#14607,.T.);
#20845=ORIENTED_EDGE('',*,*,#14608,.F.);
#20846=ORIENTED_EDGE('',*,*,#14609,.T.);
#20847=ORIENTED_EDGE('',*,*,#14605,.T.);
#20848=ORIENTED_EDGE('',*,*,#14610,.T.);
#20849=ORIENTED_EDGE('',*,*,#14611,.F.);
#20850=ORIENTED_EDGE('',*,*,#14612,.T.);
#20851=ORIENTED_EDGE('',*,*,#14608,.T.);
#20852=ORIENTED_EDGE('',*,*,#14613,.T.);
#20853=ORIENTED_EDGE('',*,*,#14614,.F.);
#20854=ORIENTED_EDGE('',*,*,#14615,.T.);
#20855=ORIENTED_EDGE('',*,*,#14611,.T.);
#20856=ORIENTED_EDGE('',*,*,#14616,.T.);
#20857=ORIENTED_EDGE('',*,*,#14617,.F.);
#20858=ORIENTED_EDGE('',*,*,#14618,.T.);
#20859=ORIENTED_EDGE('',*,*,#14614,.T.);
#20860=ORIENTED_EDGE('',*,*,#14619,.T.);
#20861=ORIENTED_EDGE('',*,*,#14620,.F.);
#20862=ORIENTED_EDGE('',*,*,#14621,.T.);
#20863=ORIENTED_EDGE('',*,*,#14617,.T.);
#20864=ORIENTED_EDGE('',*,*,#14622,.T.);
#20865=ORIENTED_EDGE('',*,*,#14623,.F.);
#20866=ORIENTED_EDGE('',*,*,#14624,.T.);
#20867=ORIENTED_EDGE('',*,*,#14620,.T.);
#20868=ORIENTED_EDGE('',*,*,#14625,.T.);
#20869=ORIENTED_EDGE('',*,*,#14626,.F.);
#20870=ORIENTED_EDGE('',*,*,#14627,.T.);
#20871=ORIENTED_EDGE('',*,*,#14623,.T.);
#20872=ORIENTED_EDGE('',*,*,#14628,.T.);
#20873=ORIENTED_EDGE('',*,*,#14629,.F.);
#20874=ORIENTED_EDGE('',*,*,#14630,.T.);
#20875=ORIENTED_EDGE('',*,*,#14626,.T.);
#20876=ORIENTED_EDGE('',*,*,#14631,.T.);
#20877=ORIENTED_EDGE('',*,*,#14632,.F.);
#20878=ORIENTED_EDGE('',*,*,#14633,.T.);
#20879=ORIENTED_EDGE('',*,*,#14629,.T.);
#20880=ORIENTED_EDGE('',*,*,#14634,.T.);
#20881=ORIENTED_EDGE('',*,*,#14635,.F.);
#20882=ORIENTED_EDGE('',*,*,#14636,.T.);
#20883=ORIENTED_EDGE('',*,*,#14632,.T.);
#20884=ORIENTED_EDGE('',*,*,#14637,.T.);
#20885=ORIENTED_EDGE('',*,*,#14638,.F.);
#20886=ORIENTED_EDGE('',*,*,#14639,.T.);
#20887=ORIENTED_EDGE('',*,*,#14635,.T.);
#20888=ORIENTED_EDGE('',*,*,#14640,.T.);
#20889=ORIENTED_EDGE('',*,*,#14641,.F.);
#20890=ORIENTED_EDGE('',*,*,#14642,.T.);
#20891=ORIENTED_EDGE('',*,*,#14638,.T.);
#20892=ORIENTED_EDGE('',*,*,#14643,.T.);
#20893=ORIENTED_EDGE('',*,*,#14644,.F.);
#20894=ORIENTED_EDGE('',*,*,#14645,.T.);
#20895=ORIENTED_EDGE('',*,*,#14646,.F.);
#20896=ORIENTED_EDGE('',*,*,#14647,.F.);
#20897=ORIENTED_EDGE('',*,*,#14648,.F.);
#20898=ORIENTED_EDGE('',*,*,#14649,.T.);
#20899=ORIENTED_EDGE('',*,*,#14644,.T.);
#20900=ORIENTED_EDGE('',*,*,#14650,.F.);
#20901=ORIENTED_EDGE('',*,*,#14651,.F.);
#20902=ORIENTED_EDGE('',*,*,#14652,.T.);
#20903=ORIENTED_EDGE('',*,*,#14648,.T.);
#20904=ORIENTED_EDGE('',*,*,#14653,.F.);
#20905=ORIENTED_EDGE('',*,*,#14654,.F.);
#20906=ORIENTED_EDGE('',*,*,#14655,.T.);
#20907=ORIENTED_EDGE('',*,*,#14651,.T.);
#20908=ORIENTED_EDGE('',*,*,#14656,.F.);
#20909=ORIENTED_EDGE('',*,*,#14657,.F.);
#20910=ORIENTED_EDGE('',*,*,#14658,.T.);
#20911=ORIENTED_EDGE('',*,*,#14654,.T.);
#20912=ORIENTED_EDGE('',*,*,#14659,.F.);
#20913=ORIENTED_EDGE('',*,*,#14660,.F.);
#20914=ORIENTED_EDGE('',*,*,#14661,.T.);
#20915=ORIENTED_EDGE('',*,*,#14657,.T.);
#20916=ORIENTED_EDGE('',*,*,#14662,.F.);
#20917=ORIENTED_EDGE('',*,*,#14663,.F.);
#20918=ORIENTED_EDGE('',*,*,#14664,.T.);
#20919=ORIENTED_EDGE('',*,*,#14660,.T.);
#20920=ORIENTED_EDGE('',*,*,#14665,.F.);
#20921=ORIENTED_EDGE('',*,*,#14666,.F.);
#20922=ORIENTED_EDGE('',*,*,#14667,.T.);
#20923=ORIENTED_EDGE('',*,*,#14663,.T.);
#20924=ORIENTED_EDGE('',*,*,#14668,.F.);
#20925=ORIENTED_EDGE('',*,*,#14669,.F.);
#20926=ORIENTED_EDGE('',*,*,#14670,.T.);
#20927=ORIENTED_EDGE('',*,*,#14666,.T.);
#20928=ORIENTED_EDGE('',*,*,#14671,.F.);
#20929=ORIENTED_EDGE('',*,*,#14672,.F.);
#20930=ORIENTED_EDGE('',*,*,#14673,.T.);
#20931=ORIENTED_EDGE('',*,*,#14669,.T.);
#20932=ORIENTED_EDGE('',*,*,#14674,.F.);
#20933=ORIENTED_EDGE('',*,*,#14675,.F.);
#20934=ORIENTED_EDGE('',*,*,#14676,.T.);
#20935=ORIENTED_EDGE('',*,*,#14672,.T.);
#20936=ORIENTED_EDGE('',*,*,#14677,.F.);
#20937=ORIENTED_EDGE('',*,*,#14678,.F.);
#20938=ORIENTED_EDGE('',*,*,#14679,.T.);
#20939=ORIENTED_EDGE('',*,*,#14675,.T.);
#20940=ORIENTED_EDGE('',*,*,#14680,.F.);
#20941=ORIENTED_EDGE('',*,*,#14681,.F.);
#20942=ORIENTED_EDGE('',*,*,#14682,.T.);
#20943=ORIENTED_EDGE('',*,*,#14678,.T.);
#20944=ORIENTED_EDGE('',*,*,#14683,.F.);
#20945=ORIENTED_EDGE('',*,*,#14684,.F.);
#20946=ORIENTED_EDGE('',*,*,#14685,.T.);
#20947=ORIENTED_EDGE('',*,*,#14681,.T.);
#20948=ORIENTED_EDGE('',*,*,#14686,.F.);
#20949=ORIENTED_EDGE('',*,*,#14687,.F.);
#20950=ORIENTED_EDGE('',*,*,#14688,.T.);
#20951=ORIENTED_EDGE('',*,*,#14684,.T.);
#20952=ORIENTED_EDGE('',*,*,#14689,.F.);
#20953=ORIENTED_EDGE('',*,*,#14690,.F.);
#20954=ORIENTED_EDGE('',*,*,#14691,.T.);
#20955=ORIENTED_EDGE('',*,*,#14687,.T.);
#20956=ORIENTED_EDGE('',*,*,#14692,.F.);
#20957=ORIENTED_EDGE('',*,*,#14693,.F.);
#20958=ORIENTED_EDGE('',*,*,#14694,.T.);
#20959=ORIENTED_EDGE('',*,*,#14690,.T.);
#20960=ORIENTED_EDGE('',*,*,#14695,.F.);
#20961=ORIENTED_EDGE('',*,*,#14696,.F.);
#20962=ORIENTED_EDGE('',*,*,#14697,.T.);
#20963=ORIENTED_EDGE('',*,*,#14693,.T.);
#20964=ORIENTED_EDGE('',*,*,#14698,.F.);
#20965=ORIENTED_EDGE('',*,*,#14699,.F.);
#20966=ORIENTED_EDGE('',*,*,#14700,.T.);
#20967=ORIENTED_EDGE('',*,*,#14696,.T.);
#20968=ORIENTED_EDGE('',*,*,#14701,.F.);
#20969=ORIENTED_EDGE('',*,*,#14646,.T.);
#20970=ORIENTED_EDGE('',*,*,#14702,.T.);
#20971=ORIENTED_EDGE('',*,*,#14703,.F.);
#20972=ORIENTED_EDGE('',*,*,#14704,.F.);
#20973=ORIENTED_EDGE('',*,*,#14705,.T.);
#20974=ORIENTED_EDGE('',*,*,#14705,.F.);
#20975=ORIENTED_EDGE('',*,*,#14706,.F.);
#20976=ORIENTED_EDGE('',*,*,#14643,.F.);
#20977=ORIENTED_EDGE('',*,*,#14640,.F.);
#20978=ORIENTED_EDGE('',*,*,#14637,.F.);
#20979=ORIENTED_EDGE('',*,*,#14634,.F.);
#20980=ORIENTED_EDGE('',*,*,#14631,.F.);
#20981=ORIENTED_EDGE('',*,*,#14628,.F.);
#20982=ORIENTED_EDGE('',*,*,#14625,.F.);
#20983=ORIENTED_EDGE('',*,*,#14622,.F.);
#20984=ORIENTED_EDGE('',*,*,#14619,.F.);
#20985=ORIENTED_EDGE('',*,*,#14616,.F.);
#20986=ORIENTED_EDGE('',*,*,#14613,.F.);
#20987=ORIENTED_EDGE('',*,*,#14610,.F.);
#20988=ORIENTED_EDGE('',*,*,#14607,.F.);
#20989=ORIENTED_EDGE('',*,*,#14604,.F.);
#20990=ORIENTED_EDGE('',*,*,#14601,.F.);
#20991=ORIENTED_EDGE('',*,*,#14598,.F.);
#20992=ORIENTED_EDGE('',*,*,#14595,.F.);
#20993=ORIENTED_EDGE('',*,*,#14592,.F.);
#20994=ORIENTED_EDGE('',*,*,#14707,.F.);
#20995=ORIENTED_EDGE('',*,*,#14708,.T.);
#20996=ORIENTED_EDGE('',*,*,#14701,.T.);
#20997=ORIENTED_EDGE('',*,*,#14698,.T.);
#20998=ORIENTED_EDGE('',*,*,#14695,.T.);
#20999=ORIENTED_EDGE('',*,*,#14692,.T.);
#21000=ORIENTED_EDGE('',*,*,#14689,.T.);
#21001=ORIENTED_EDGE('',*,*,#14686,.T.);
#21002=ORIENTED_EDGE('',*,*,#14683,.T.);
#21003=ORIENTED_EDGE('',*,*,#14680,.T.);
#21004=ORIENTED_EDGE('',*,*,#14677,.T.);
#21005=ORIENTED_EDGE('',*,*,#14674,.T.);
#21006=ORIENTED_EDGE('',*,*,#14671,.T.);
#21007=ORIENTED_EDGE('',*,*,#14668,.T.);
#21008=ORIENTED_EDGE('',*,*,#14665,.T.);
#21009=ORIENTED_EDGE('',*,*,#14662,.T.);
#21010=ORIENTED_EDGE('',*,*,#14659,.T.);
#21011=ORIENTED_EDGE('',*,*,#14656,.T.);
#21012=ORIENTED_EDGE('',*,*,#14653,.T.);
#21013=ORIENTED_EDGE('',*,*,#14650,.T.);
#21014=ORIENTED_EDGE('',*,*,#14647,.T.);
#21015=ORIENTED_EDGE('',*,*,#14588,.F.);
#21016=ORIENTED_EDGE('',*,*,#14709,.T.);
#21017=ORIENTED_EDGE('',*,*,#14710,.T.);
#21018=ORIENTED_EDGE('',*,*,#14707,.T.);
#21019=ORIENTED_EDGE('',*,*,#14591,.F.);
#21020=ORIENTED_EDGE('',*,*,#14699,.T.);
#21021=ORIENTED_EDGE('',*,*,#14708,.F.);
#21022=ORIENTED_EDGE('',*,*,#14710,.F.);
#21023=ORIENTED_EDGE('',*,*,#14711,.T.);
#21024=ORIENTED_EDGE('',*,*,#14702,.F.);
#21025=ORIENTED_EDGE('',*,*,#14645,.F.);
#21026=ORIENTED_EDGE('',*,*,#14649,.F.);
#21027=ORIENTED_EDGE('',*,*,#14652,.F.);
#21028=ORIENTED_EDGE('',*,*,#14655,.F.);
#21029=ORIENTED_EDGE('',*,*,#14658,.F.);
#21030=ORIENTED_EDGE('',*,*,#14661,.F.);
#21031=ORIENTED_EDGE('',*,*,#14664,.F.);
#21032=ORIENTED_EDGE('',*,*,#14667,.F.);
#21033=ORIENTED_EDGE('',*,*,#14670,.F.);
#21034=ORIENTED_EDGE('',*,*,#14673,.F.);
#21035=ORIENTED_EDGE('',*,*,#14676,.F.);
#21036=ORIENTED_EDGE('',*,*,#14679,.F.);
#21037=ORIENTED_EDGE('',*,*,#14682,.F.);
#21038=ORIENTED_EDGE('',*,*,#14685,.F.);
#21039=ORIENTED_EDGE('',*,*,#14688,.F.);
#21040=ORIENTED_EDGE('',*,*,#14691,.F.);
#21041=ORIENTED_EDGE('',*,*,#14694,.F.);
#21042=ORIENTED_EDGE('',*,*,#14697,.F.);
#21043=ORIENTED_EDGE('',*,*,#14700,.F.);
#21044=ORIENTED_EDGE('',*,*,#14711,.F.);
#21045=ORIENTED_EDGE('',*,*,#14709,.F.);
#21046=ORIENTED_EDGE('',*,*,#14587,.F.);
#21047=ORIENTED_EDGE('',*,*,#14594,.F.);
#21048=ORIENTED_EDGE('',*,*,#14597,.F.);
#21049=ORIENTED_EDGE('',*,*,#14600,.F.);
#21050=ORIENTED_EDGE('',*,*,#14603,.F.);
#21051=ORIENTED_EDGE('',*,*,#14606,.F.);
#21052=ORIENTED_EDGE('',*,*,#14609,.F.);
#21053=ORIENTED_EDGE('',*,*,#14612,.F.);
#21054=ORIENTED_EDGE('',*,*,#14615,.F.);
#21055=ORIENTED_EDGE('',*,*,#14618,.F.);
#21056=ORIENTED_EDGE('',*,*,#14621,.F.);
#21057=ORIENTED_EDGE('',*,*,#14624,.F.);
#21058=ORIENTED_EDGE('',*,*,#14627,.F.);
#21059=ORIENTED_EDGE('',*,*,#14630,.F.);
#21060=ORIENTED_EDGE('',*,*,#14633,.F.);
#21061=ORIENTED_EDGE('',*,*,#14636,.F.);
#21062=ORIENTED_EDGE('',*,*,#14639,.F.);
#21063=ORIENTED_EDGE('',*,*,#14642,.F.);
#21064=ORIENTED_EDGE('',*,*,#14712,.F.);
#21065=ORIENTED_EDGE('',*,*,#14713,.F.);
#21066=ORIENTED_EDGE('',*,*,#14714,.T.);
#21067=ORIENTED_EDGE('',*,*,#14715,.T.);
#21068=ORIENTED_EDGE('',*,*,#14716,.F.);
#21069=ORIENTED_EDGE('',*,*,#14715,.F.);
#21070=ORIENTED_EDGE('',*,*,#14717,.T.);
#21071=ORIENTED_EDGE('',*,*,#14718,.F.);
#21072=ORIENTED_EDGE('',*,*,#14719,.F.);
#21073=ORIENTED_EDGE('',*,*,#14720,.F.);
#21074=ORIENTED_EDGE('',*,*,#14717,.F.);
#21075=ORIENTED_EDGE('',*,*,#14714,.F.);
#21076=ORIENTED_EDGE('',*,*,#14721,.F.);
#21077=ORIENTED_EDGE('',*,*,#14722,.T.);
#21078=ORIENTED_EDGE('',*,*,#14723,.T.);
#21079=ORIENTED_EDGE('',*,*,#14724,.F.);
#21080=ORIENTED_EDGE('',*,*,#14723,.F.);
#21081=ORIENTED_EDGE('',*,*,#14725,.T.);
#21082=ORIENTED_EDGE('',*,*,#14726,.F.);
#21083=ORIENTED_EDGE('',*,*,#14727,.F.);
#21084=ORIENTED_EDGE('',*,*,#14728,.F.);
#21085=ORIENTED_EDGE('',*,*,#14725,.F.);
#21086=ORIENTED_EDGE('',*,*,#14722,.F.);
#21087=ORIENTED_EDGE('',*,*,#14729,.F.);
#21088=ORIENTED_EDGE('',*,*,#14730,.T.);
#21089=ORIENTED_EDGE('',*,*,#14731,.T.);
#21090=ORIENTED_EDGE('',*,*,#14732,.F.);
#21091=ORIENTED_EDGE('',*,*,#14731,.F.);
#21092=ORIENTED_EDGE('',*,*,#14733,.T.);
#21093=ORIENTED_EDGE('',*,*,#14734,.F.);
#21094=ORIENTED_EDGE('',*,*,#14735,.F.);
#21095=ORIENTED_EDGE('',*,*,#14736,.F.);
#21096=ORIENTED_EDGE('',*,*,#14733,.F.);
#21097=ORIENTED_EDGE('',*,*,#14730,.F.);
#21098=ORIENTED_EDGE('',*,*,#14737,.F.);
#21099=ORIENTED_EDGE('',*,*,#14738,.T.);
#21100=ORIENTED_EDGE('',*,*,#14739,.T.);
#21101=ORIENTED_EDGE('',*,*,#14740,.F.);
#21102=ORIENTED_EDGE('',*,*,#14739,.F.);
#21103=ORIENTED_EDGE('',*,*,#14741,.T.);
#21104=ORIENTED_EDGE('',*,*,#14742,.F.);
#21105=ORIENTED_EDGE('',*,*,#14743,.F.);
#21106=ORIENTED_EDGE('',*,*,#14744,.F.);
#21107=ORIENTED_EDGE('',*,*,#14741,.F.);
#21108=ORIENTED_EDGE('',*,*,#14738,.F.);
#21109=ORIENTED_EDGE('',*,*,#14745,.F.);
#21110=ORIENTED_EDGE('',*,*,#14746,.T.);
#21111=ORIENTED_EDGE('',*,*,#14747,.T.);
#21112=ORIENTED_EDGE('',*,*,#14748,.F.);
#21113=ORIENTED_EDGE('',*,*,#14747,.F.);
#21114=ORIENTED_EDGE('',*,*,#14749,.T.);
#21115=ORIENTED_EDGE('',*,*,#14750,.F.);
#21116=ORIENTED_EDGE('',*,*,#14751,.F.);
#21117=ORIENTED_EDGE('',*,*,#14752,.F.);
#21118=ORIENTED_EDGE('',*,*,#14749,.F.);
#21119=ORIENTED_EDGE('',*,*,#14746,.F.);
#21120=ORIENTED_EDGE('',*,*,#14753,.F.);
#21121=ORIENTED_EDGE('',*,*,#14754,.T.);
#21122=ORIENTED_EDGE('',*,*,#14755,.T.);
#21123=ORIENTED_EDGE('',*,*,#14756,.F.);
#21124=ORIENTED_EDGE('',*,*,#14755,.F.);
#21125=ORIENTED_EDGE('',*,*,#14757,.T.);
#21126=ORIENTED_EDGE('',*,*,#14758,.F.);
#21127=ORIENTED_EDGE('',*,*,#14759,.F.);
#21128=ORIENTED_EDGE('',*,*,#14760,.F.);
#21129=ORIENTED_EDGE('',*,*,#14757,.F.);
#21130=ORIENTED_EDGE('',*,*,#14754,.F.);
#21131=ORIENTED_EDGE('',*,*,#14761,.F.);
#21132=ORIENTED_EDGE('',*,*,#14762,.T.);
#21133=ORIENTED_EDGE('',*,*,#14763,.T.);
#21134=ORIENTED_EDGE('',*,*,#14764,.F.);
#21135=ORIENTED_EDGE('',*,*,#14763,.F.);
#21136=ORIENTED_EDGE('',*,*,#14765,.T.);
#21137=ORIENTED_EDGE('',*,*,#14766,.F.);
#21138=ORIENTED_EDGE('',*,*,#14767,.F.);
#21139=ORIENTED_EDGE('',*,*,#14768,.F.);
#21140=ORIENTED_EDGE('',*,*,#14765,.F.);
#21141=ORIENTED_EDGE('',*,*,#14762,.F.);
#21142=ORIENTED_EDGE('',*,*,#14769,.F.);
#21143=ORIENTED_EDGE('',*,*,#14770,.T.);
#21144=ORIENTED_EDGE('',*,*,#14771,.T.);
#21145=ORIENTED_EDGE('',*,*,#14772,.F.);
#21146=ORIENTED_EDGE('',*,*,#14771,.F.);
#21147=ORIENTED_EDGE('',*,*,#14773,.T.);
#21148=ORIENTED_EDGE('',*,*,#14774,.F.);
#21149=ORIENTED_EDGE('',*,*,#14775,.F.);
#21150=ORIENTED_EDGE('',*,*,#14776,.F.);
#21151=ORIENTED_EDGE('',*,*,#14773,.F.);
#21152=ORIENTED_EDGE('',*,*,#14770,.F.);
#21153=ORIENTED_EDGE('',*,*,#14777,.F.);
#21154=ORIENTED_EDGE('',*,*,#14778,.T.);
#21155=ORIENTED_EDGE('',*,*,#14779,.T.);
#21156=ORIENTED_EDGE('',*,*,#14780,.F.);
#21157=ORIENTED_EDGE('',*,*,#14779,.F.);
#21158=ORIENTED_EDGE('',*,*,#14781,.T.);
#21159=ORIENTED_EDGE('',*,*,#14782,.F.);
#21160=ORIENTED_EDGE('',*,*,#14783,.F.);
#21161=ORIENTED_EDGE('',*,*,#14784,.F.);
#21162=ORIENTED_EDGE('',*,*,#14781,.F.);
#21163=ORIENTED_EDGE('',*,*,#14778,.F.);
#21164=ORIENTED_EDGE('',*,*,#14785,.F.);
#21165=ORIENTED_EDGE('',*,*,#14786,.T.);
#21166=ORIENTED_EDGE('',*,*,#14787,.T.);
#21167=ORIENTED_EDGE('',*,*,#14788,.F.);
#21168=ORIENTED_EDGE('',*,*,#14787,.F.);
#21169=ORIENTED_EDGE('',*,*,#14789,.T.);
#21170=ORIENTED_EDGE('',*,*,#14790,.F.);
#21171=ORIENTED_EDGE('',*,*,#14791,.F.);
#21172=ORIENTED_EDGE('',*,*,#14792,.F.);
#21173=ORIENTED_EDGE('',*,*,#14789,.F.);
#21174=ORIENTED_EDGE('',*,*,#14786,.F.);
#21175=ORIENTED_EDGE('',*,*,#14793,.F.);
#21176=ORIENTED_EDGE('',*,*,#14794,.T.);
#21177=ORIENTED_EDGE('',*,*,#14795,.T.);
#21178=ORIENTED_EDGE('',*,*,#14796,.F.);
#21179=ORIENTED_EDGE('',*,*,#14795,.F.);
#21180=ORIENTED_EDGE('',*,*,#14797,.T.);
#21181=ORIENTED_EDGE('',*,*,#14798,.F.);
#21182=ORIENTED_EDGE('',*,*,#14799,.F.);
#21183=ORIENTED_EDGE('',*,*,#14800,.F.);
#21184=ORIENTED_EDGE('',*,*,#14797,.F.);
#21185=ORIENTED_EDGE('',*,*,#14794,.F.);
#21186=ORIENTED_EDGE('',*,*,#14801,.F.);
#21187=ORIENTED_EDGE('',*,*,#14802,.T.);
#21188=ORIENTED_EDGE('',*,*,#14803,.T.);
#21189=ORIENTED_EDGE('',*,*,#14804,.F.);
#21190=ORIENTED_EDGE('',*,*,#14803,.F.);
#21191=ORIENTED_EDGE('',*,*,#14805,.T.);
#21192=ORIENTED_EDGE('',*,*,#14806,.F.);
#21193=ORIENTED_EDGE('',*,*,#14807,.F.);
#21194=ORIENTED_EDGE('',*,*,#14808,.F.);
#21195=ORIENTED_EDGE('',*,*,#14805,.F.);
#21196=ORIENTED_EDGE('',*,*,#14802,.F.);
#21197=ORIENTED_EDGE('',*,*,#14809,.F.);
#21198=ORIENTED_EDGE('',*,*,#14810,.T.);
#21199=ORIENTED_EDGE('',*,*,#14811,.T.);
#21200=ORIENTED_EDGE('',*,*,#14812,.F.);
#21201=ORIENTED_EDGE('',*,*,#14811,.F.);
#21202=ORIENTED_EDGE('',*,*,#14813,.T.);
#21203=ORIENTED_EDGE('',*,*,#14814,.F.);
#21204=ORIENTED_EDGE('',*,*,#14815,.F.);
#21205=ORIENTED_EDGE('',*,*,#14816,.F.);
#21206=ORIENTED_EDGE('',*,*,#14813,.F.);
#21207=ORIENTED_EDGE('',*,*,#14810,.F.);
#21208=ORIENTED_EDGE('',*,*,#14817,.F.);
#21209=ORIENTED_EDGE('',*,*,#14818,.T.);
#21210=ORIENTED_EDGE('',*,*,#14819,.T.);
#21211=ORIENTED_EDGE('',*,*,#14820,.F.);
#21212=ORIENTED_EDGE('',*,*,#14819,.F.);
#21213=ORIENTED_EDGE('',*,*,#14821,.T.);
#21214=ORIENTED_EDGE('',*,*,#14822,.F.);
#21215=ORIENTED_EDGE('',*,*,#14823,.F.);
#21216=ORIENTED_EDGE('',*,*,#14824,.F.);
#21217=ORIENTED_EDGE('',*,*,#14821,.F.);
#21218=ORIENTED_EDGE('',*,*,#14818,.F.);
#21219=ORIENTED_EDGE('',*,*,#14825,.F.);
#21220=ORIENTED_EDGE('',*,*,#14826,.T.);
#21221=ORIENTED_EDGE('',*,*,#14827,.T.);
#21222=ORIENTED_EDGE('',*,*,#14828,.F.);
#21223=ORIENTED_EDGE('',*,*,#14827,.F.);
#21224=ORIENTED_EDGE('',*,*,#14829,.T.);
#21225=ORIENTED_EDGE('',*,*,#14830,.F.);
#21226=ORIENTED_EDGE('',*,*,#14831,.F.);
#21227=ORIENTED_EDGE('',*,*,#14832,.F.);
#21228=ORIENTED_EDGE('',*,*,#14829,.F.);
#21229=ORIENTED_EDGE('',*,*,#14826,.F.);
#21230=ORIENTED_EDGE('',*,*,#14833,.F.);
#21231=ORIENTED_EDGE('',*,*,#14834,.T.);
#21232=ORIENTED_EDGE('',*,*,#14835,.T.);
#21233=ORIENTED_EDGE('',*,*,#14836,.F.);
#21234=ORIENTED_EDGE('',*,*,#14835,.F.);
#21235=ORIENTED_EDGE('',*,*,#14837,.T.);
#21236=ORIENTED_EDGE('',*,*,#14838,.F.);
#21237=ORIENTED_EDGE('',*,*,#14839,.F.);
#21238=ORIENTED_EDGE('',*,*,#14840,.F.);
#21239=ORIENTED_EDGE('',*,*,#14837,.F.);
#21240=ORIENTED_EDGE('',*,*,#14834,.F.);
#21241=ORIENTED_EDGE('',*,*,#14841,.F.);
#21242=ORIENTED_EDGE('',*,*,#14842,.T.);
#21243=ORIENTED_EDGE('',*,*,#14843,.T.);
#21244=ORIENTED_EDGE('',*,*,#14844,.F.);
#21245=ORIENTED_EDGE('',*,*,#14843,.F.);
#21246=ORIENTED_EDGE('',*,*,#14845,.T.);
#21247=ORIENTED_EDGE('',*,*,#14846,.F.);
#21248=ORIENTED_EDGE('',*,*,#14847,.F.);
#21249=ORIENTED_EDGE('',*,*,#14848,.F.);
#21250=ORIENTED_EDGE('',*,*,#14845,.F.);
#21251=ORIENTED_EDGE('',*,*,#14842,.F.);
#21252=ORIENTED_EDGE('',*,*,#14849,.F.);
#21253=ORIENTED_EDGE('',*,*,#14850,.T.);
#21254=ORIENTED_EDGE('',*,*,#14851,.T.);
#21255=ORIENTED_EDGE('',*,*,#14852,.F.);
#21256=ORIENTED_EDGE('',*,*,#14853,.F.);
#21257=ORIENTED_EDGE('',*,*,#14851,.F.);
#21258=ORIENTED_EDGE('',*,*,#14854,.T.);
#21259=ORIENTED_EDGE('',*,*,#14855,.F.);
#21260=ORIENTED_EDGE('',*,*,#14856,.F.);
#21261=ORIENTED_EDGE('',*,*,#14857,.F.);
#21262=ORIENTED_EDGE('',*,*,#14854,.F.);
#21263=ORIENTED_EDGE('',*,*,#14850,.F.);
#21264=ORIENTED_EDGE('',*,*,#14858,.F.);
#21265=ORIENTED_EDGE('',*,*,#14859,.T.);
#21266=ORIENTED_EDGE('',*,*,#14860,.T.);
#21267=ORIENTED_EDGE('',*,*,#14861,.F.);
#21268=ORIENTED_EDGE('',*,*,#14860,.F.);
#21269=ORIENTED_EDGE('',*,*,#14862,.T.);
#21270=ORIENTED_EDGE('',*,*,#14863,.F.);
#21271=ORIENTED_EDGE('',*,*,#14864,.F.);
#21272=ORIENTED_EDGE('',*,*,#14865,.F.);
#21273=ORIENTED_EDGE('',*,*,#14862,.F.);
#21274=ORIENTED_EDGE('',*,*,#14859,.F.);
#21275=ORIENTED_EDGE('',*,*,#14866,.F.);
#21276=ORIENTED_EDGE('',*,*,#14867,.T.);
#21277=ORIENTED_EDGE('',*,*,#14868,.T.);
#21278=ORIENTED_EDGE('',*,*,#14869,.F.);
#21279=ORIENTED_EDGE('',*,*,#14868,.F.);
#21280=ORIENTED_EDGE('',*,*,#14870,.T.);
#21281=ORIENTED_EDGE('',*,*,#14871,.F.);
#21282=ORIENTED_EDGE('',*,*,#14872,.F.);
#21283=ORIENTED_EDGE('',*,*,#14873,.F.);
#21284=ORIENTED_EDGE('',*,*,#14870,.F.);
#21285=ORIENTED_EDGE('',*,*,#14867,.F.);
#21286=ORIENTED_EDGE('',*,*,#14874,.F.);
#21287=ORIENTED_EDGE('',*,*,#14875,.T.);
#21288=ORIENTED_EDGE('',*,*,#14876,.T.);
#21289=ORIENTED_EDGE('',*,*,#14877,.F.);
#21290=ORIENTED_EDGE('',*,*,#14876,.F.);
#21291=ORIENTED_EDGE('',*,*,#14878,.T.);
#21292=ORIENTED_EDGE('',*,*,#14879,.F.);
#21293=ORIENTED_EDGE('',*,*,#14880,.F.);
#21294=ORIENTED_EDGE('',*,*,#14881,.F.);
#21295=ORIENTED_EDGE('',*,*,#14878,.F.);
#21296=ORIENTED_EDGE('',*,*,#14875,.F.);
#21297=ORIENTED_EDGE('',*,*,#14882,.F.);
#21298=ORIENTED_EDGE('',*,*,#14883,.T.);
#21299=ORIENTED_EDGE('',*,*,#14884,.T.);
#21300=ORIENTED_EDGE('',*,*,#14885,.F.);
#21301=ORIENTED_EDGE('',*,*,#14884,.F.);
#21302=ORIENTED_EDGE('',*,*,#14886,.T.);
#21303=ORIENTED_EDGE('',*,*,#14887,.F.);
#21304=ORIENTED_EDGE('',*,*,#14888,.F.);
#21305=ORIENTED_EDGE('',*,*,#14889,.F.);
#21306=ORIENTED_EDGE('',*,*,#14886,.F.);
#21307=ORIENTED_EDGE('',*,*,#14883,.F.);
#21308=ORIENTED_EDGE('',*,*,#14890,.F.);
#21309=ORIENTED_EDGE('',*,*,#14891,.T.);
#21310=ORIENTED_EDGE('',*,*,#14892,.T.);
#21311=ORIENTED_EDGE('',*,*,#14893,.F.);
#21312=ORIENTED_EDGE('',*,*,#14892,.F.);
#21313=ORIENTED_EDGE('',*,*,#14894,.T.);
#21314=ORIENTED_EDGE('',*,*,#14895,.F.);
#21315=ORIENTED_EDGE('',*,*,#14896,.F.);
#21316=ORIENTED_EDGE('',*,*,#14897,.F.);
#21317=ORIENTED_EDGE('',*,*,#14894,.F.);
#21318=ORIENTED_EDGE('',*,*,#14891,.F.);
#21319=ORIENTED_EDGE('',*,*,#14898,.F.);
#21320=ORIENTED_EDGE('',*,*,#14899,.T.);
#21321=ORIENTED_EDGE('',*,*,#14900,.T.);
#21322=ORIENTED_EDGE('',*,*,#14901,.F.);
#21323=ORIENTED_EDGE('',*,*,#14900,.F.);
#21324=ORIENTED_EDGE('',*,*,#14902,.T.);
#21325=ORIENTED_EDGE('',*,*,#14903,.F.);
#21326=ORIENTED_EDGE('',*,*,#14904,.F.);
#21327=ORIENTED_EDGE('',*,*,#14905,.F.);
#21328=ORIENTED_EDGE('',*,*,#14902,.F.);
#21329=ORIENTED_EDGE('',*,*,#14899,.F.);
#21330=ORIENTED_EDGE('',*,*,#14906,.F.);
#21331=ORIENTED_EDGE('',*,*,#14907,.T.);
#21332=ORIENTED_EDGE('',*,*,#14908,.T.);
#21333=ORIENTED_EDGE('',*,*,#14909,.F.);
#21334=ORIENTED_EDGE('',*,*,#14908,.F.);
#21335=ORIENTED_EDGE('',*,*,#14910,.T.);
#21336=ORIENTED_EDGE('',*,*,#14911,.F.);
#21337=ORIENTED_EDGE('',*,*,#14912,.F.);
#21338=ORIENTED_EDGE('',*,*,#14913,.F.);
#21339=ORIENTED_EDGE('',*,*,#14910,.F.);
#21340=ORIENTED_EDGE('',*,*,#14907,.F.);
#21341=ORIENTED_EDGE('',*,*,#14914,.F.);
#21342=ORIENTED_EDGE('',*,*,#14915,.T.);
#21343=ORIENTED_EDGE('',*,*,#14916,.T.);
#21344=ORIENTED_EDGE('',*,*,#14917,.F.);
#21345=ORIENTED_EDGE('',*,*,#14916,.F.);
#21346=ORIENTED_EDGE('',*,*,#14918,.T.);
#21347=ORIENTED_EDGE('',*,*,#14919,.F.);
#21348=ORIENTED_EDGE('',*,*,#14920,.F.);
#21349=ORIENTED_EDGE('',*,*,#14921,.F.);
#21350=ORIENTED_EDGE('',*,*,#14918,.F.);
#21351=ORIENTED_EDGE('',*,*,#14915,.F.);
#21352=ORIENTED_EDGE('',*,*,#14922,.F.);
#21353=ORIENTED_EDGE('',*,*,#14923,.T.);
#21354=ORIENTED_EDGE('',*,*,#14924,.T.);
#21355=ORIENTED_EDGE('',*,*,#14925,.F.);
#21356=ORIENTED_EDGE('',*,*,#14924,.F.);
#21357=ORIENTED_EDGE('',*,*,#14926,.T.);
#21358=ORIENTED_EDGE('',*,*,#14927,.F.);
#21359=ORIENTED_EDGE('',*,*,#14928,.F.);
#21360=ORIENTED_EDGE('',*,*,#14929,.F.);
#21361=ORIENTED_EDGE('',*,*,#14926,.F.);
#21362=ORIENTED_EDGE('',*,*,#14923,.F.);
#21363=ORIENTED_EDGE('',*,*,#14930,.F.);
#21364=ORIENTED_EDGE('',*,*,#14931,.T.);
#21365=ORIENTED_EDGE('',*,*,#14932,.T.);
#21366=ORIENTED_EDGE('',*,*,#14933,.F.);
#21367=ORIENTED_EDGE('',*,*,#14932,.F.);
#21368=ORIENTED_EDGE('',*,*,#14934,.T.);
#21369=ORIENTED_EDGE('',*,*,#14935,.F.);
#21370=ORIENTED_EDGE('',*,*,#14936,.F.);
#21371=ORIENTED_EDGE('',*,*,#14937,.F.);
#21372=ORIENTED_EDGE('',*,*,#14934,.F.);
#21373=ORIENTED_EDGE('',*,*,#14931,.F.);
#21374=ORIENTED_EDGE('',*,*,#14938,.F.);
#21375=ORIENTED_EDGE('',*,*,#14939,.T.);
#21376=ORIENTED_EDGE('',*,*,#14940,.T.);
#21377=ORIENTED_EDGE('',*,*,#14941,.F.);
#21378=ORIENTED_EDGE('',*,*,#14940,.F.);
#21379=ORIENTED_EDGE('',*,*,#14942,.T.);
#21380=ORIENTED_EDGE('',*,*,#14943,.F.);
#21381=ORIENTED_EDGE('',*,*,#14944,.F.);
#21382=ORIENTED_EDGE('',*,*,#14945,.F.);
#21383=ORIENTED_EDGE('',*,*,#14942,.F.);
#21384=ORIENTED_EDGE('',*,*,#14939,.F.);
#21385=ORIENTED_EDGE('',*,*,#14946,.F.);
#21386=ORIENTED_EDGE('',*,*,#14947,.T.);
#21387=ORIENTED_EDGE('',*,*,#14948,.T.);
#21388=ORIENTED_EDGE('',*,*,#14949,.F.);
#21389=ORIENTED_EDGE('',*,*,#14948,.F.);
#21390=ORIENTED_EDGE('',*,*,#14950,.T.);
#21391=ORIENTED_EDGE('',*,*,#14951,.F.);
#21392=ORIENTED_EDGE('',*,*,#14952,.F.);
#21393=ORIENTED_EDGE('',*,*,#14953,.F.);
#21394=ORIENTED_EDGE('',*,*,#14950,.F.);
#21395=ORIENTED_EDGE('',*,*,#14947,.F.);
#21396=ORIENTED_EDGE('',*,*,#14954,.F.);
#21397=ORIENTED_EDGE('',*,*,#14955,.T.);
#21398=ORIENTED_EDGE('',*,*,#14956,.T.);
#21399=ORIENTED_EDGE('',*,*,#14957,.F.);
#21400=ORIENTED_EDGE('',*,*,#14956,.F.);
#21401=ORIENTED_EDGE('',*,*,#14958,.T.);
#21402=ORIENTED_EDGE('',*,*,#14959,.F.);
#21403=ORIENTED_EDGE('',*,*,#14960,.F.);
#21404=ORIENTED_EDGE('',*,*,#14961,.F.);
#21405=ORIENTED_EDGE('',*,*,#14958,.F.);
#21406=ORIENTED_EDGE('',*,*,#14955,.F.);
#21407=ORIENTED_EDGE('',*,*,#14962,.F.);
#21408=ORIENTED_EDGE('',*,*,#14963,.T.);
#21409=ORIENTED_EDGE('',*,*,#14964,.T.);
#21410=ORIENTED_EDGE('',*,*,#14965,.F.);
#21411=ORIENTED_EDGE('',*,*,#14964,.F.);
#21412=ORIENTED_EDGE('',*,*,#14966,.T.);
#21413=ORIENTED_EDGE('',*,*,#14967,.F.);
#21414=ORIENTED_EDGE('',*,*,#14968,.F.);
#21415=ORIENTED_EDGE('',*,*,#14969,.F.);
#21416=ORIENTED_EDGE('',*,*,#14966,.F.);
#21417=ORIENTED_EDGE('',*,*,#14963,.F.);
#21418=ORIENTED_EDGE('',*,*,#14970,.F.);
#21419=ORIENTED_EDGE('',*,*,#14971,.T.);
#21420=ORIENTED_EDGE('',*,*,#14972,.T.);
#21421=ORIENTED_EDGE('',*,*,#14973,.F.);
#21422=ORIENTED_EDGE('',*,*,#14972,.F.);
#21423=ORIENTED_EDGE('',*,*,#14974,.T.);
#21424=ORIENTED_EDGE('',*,*,#14975,.F.);
#21425=ORIENTED_EDGE('',*,*,#14976,.F.);
#21426=ORIENTED_EDGE('',*,*,#14977,.F.);
#21427=ORIENTED_EDGE('',*,*,#14974,.F.);
#21428=ORIENTED_EDGE('',*,*,#14971,.F.);
#21429=ORIENTED_EDGE('',*,*,#14978,.F.);
#21430=ORIENTED_EDGE('',*,*,#14979,.T.);
#21431=ORIENTED_EDGE('',*,*,#14980,.T.);
#21432=ORIENTED_EDGE('',*,*,#14981,.F.);
#21433=ORIENTED_EDGE('',*,*,#14980,.F.);
#21434=ORIENTED_EDGE('',*,*,#14982,.T.);
#21435=ORIENTED_EDGE('',*,*,#14983,.F.);
#21436=ORIENTED_EDGE('',*,*,#14984,.F.);
#21437=ORIENTED_EDGE('',*,*,#14985,.F.);
#21438=ORIENTED_EDGE('',*,*,#14982,.F.);
#21439=ORIENTED_EDGE('',*,*,#14979,.F.);
#21440=ORIENTED_EDGE('',*,*,#14986,.F.);
#21441=ORIENTED_EDGE('',*,*,#14987,.T.);
#21442=ORIENTED_EDGE('',*,*,#14988,.T.);
#21443=ORIENTED_EDGE('',*,*,#14989,.F.);
#21444=ORIENTED_EDGE('',*,*,#14988,.F.);
#21445=ORIENTED_EDGE('',*,*,#14990,.T.);
#21446=ORIENTED_EDGE('',*,*,#14991,.F.);
#21447=ORIENTED_EDGE('',*,*,#14992,.F.);
#21448=ORIENTED_EDGE('',*,*,#14993,.F.);
#21449=ORIENTED_EDGE('',*,*,#14990,.F.);
#21450=ORIENTED_EDGE('',*,*,#14987,.F.);
#21451=ORIENTED_EDGE('',*,*,#14719,.T.);
#21452=ORIENTED_EDGE('',*,*,#14713,.T.);
#21453=ORIENTED_EDGE('',*,*,#14716,.T.);
#21454=ORIENTED_EDGE('',*,*,#14994,.F.);
#21455=ORIENTED_EDGE('',*,*,#14727,.T.);
#21456=ORIENTED_EDGE('',*,*,#14721,.T.);
#21457=ORIENTED_EDGE('',*,*,#14724,.T.);
#21458=ORIENTED_EDGE('',*,*,#14995,.F.);
#21459=ORIENTED_EDGE('',*,*,#14735,.T.);
#21460=ORIENTED_EDGE('',*,*,#14729,.T.);
#21461=ORIENTED_EDGE('',*,*,#14732,.T.);
#21462=ORIENTED_EDGE('',*,*,#14996,.F.);
#21463=ORIENTED_EDGE('',*,*,#14743,.T.);
#21464=ORIENTED_EDGE('',*,*,#14737,.T.);
#21465=ORIENTED_EDGE('',*,*,#14740,.T.);
#21466=ORIENTED_EDGE('',*,*,#14997,.F.);
#21467=ORIENTED_EDGE('',*,*,#14751,.T.);
#21468=ORIENTED_EDGE('',*,*,#14745,.T.);
#21469=ORIENTED_EDGE('',*,*,#14748,.T.);
#21470=ORIENTED_EDGE('',*,*,#14998,.F.);
#21471=ORIENTED_EDGE('',*,*,#14759,.T.);
#21472=ORIENTED_EDGE('',*,*,#14753,.T.);
#21473=ORIENTED_EDGE('',*,*,#14756,.T.);
#21474=ORIENTED_EDGE('',*,*,#14999,.F.);
#21475=ORIENTED_EDGE('',*,*,#14767,.T.);
#21476=ORIENTED_EDGE('',*,*,#14761,.T.);
#21477=ORIENTED_EDGE('',*,*,#14764,.T.);
#21478=ORIENTED_EDGE('',*,*,#15000,.F.);
#21479=ORIENTED_EDGE('',*,*,#14775,.T.);
#21480=ORIENTED_EDGE('',*,*,#14769,.T.);
#21481=ORIENTED_EDGE('',*,*,#14772,.T.);
#21482=ORIENTED_EDGE('',*,*,#15001,.F.);
#21483=ORIENTED_EDGE('',*,*,#14783,.T.);
#21484=ORIENTED_EDGE('',*,*,#14777,.T.);
#21485=ORIENTED_EDGE('',*,*,#14780,.T.);
#21486=ORIENTED_EDGE('',*,*,#15002,.F.);
#21487=ORIENTED_EDGE('',*,*,#14791,.T.);
#21488=ORIENTED_EDGE('',*,*,#14785,.T.);
#21489=ORIENTED_EDGE('',*,*,#14788,.T.);
#21490=ORIENTED_EDGE('',*,*,#15003,.F.);
#21491=ORIENTED_EDGE('',*,*,#14799,.T.);
#21492=ORIENTED_EDGE('',*,*,#14793,.T.);
#21493=ORIENTED_EDGE('',*,*,#14796,.T.);
#21494=ORIENTED_EDGE('',*,*,#15004,.F.);
#21495=ORIENTED_EDGE('',*,*,#14807,.T.);
#21496=ORIENTED_EDGE('',*,*,#14801,.T.);
#21497=ORIENTED_EDGE('',*,*,#14804,.T.);
#21498=ORIENTED_EDGE('',*,*,#15005,.F.);
#21499=ORIENTED_EDGE('',*,*,#14815,.T.);
#21500=ORIENTED_EDGE('',*,*,#14809,.T.);
#21501=ORIENTED_EDGE('',*,*,#14812,.T.);
#21502=ORIENTED_EDGE('',*,*,#15006,.F.);
#21503=ORIENTED_EDGE('',*,*,#14823,.T.);
#21504=ORIENTED_EDGE('',*,*,#14817,.T.);
#21505=ORIENTED_EDGE('',*,*,#14820,.T.);
#21506=ORIENTED_EDGE('',*,*,#15007,.F.);
#21507=ORIENTED_EDGE('',*,*,#14831,.T.);
#21508=ORIENTED_EDGE('',*,*,#14825,.T.);
#21509=ORIENTED_EDGE('',*,*,#14828,.T.);
#21510=ORIENTED_EDGE('',*,*,#15008,.F.);
#21511=ORIENTED_EDGE('',*,*,#14839,.T.);
#21512=ORIENTED_EDGE('',*,*,#14833,.T.);
#21513=ORIENTED_EDGE('',*,*,#14836,.T.);
#21514=ORIENTED_EDGE('',*,*,#15009,.F.);
#21515=ORIENTED_EDGE('',*,*,#14847,.T.);
#21516=ORIENTED_EDGE('',*,*,#14841,.T.);
#21517=ORIENTED_EDGE('',*,*,#14844,.T.);
#21518=ORIENTED_EDGE('',*,*,#15010,.F.);
#21519=ORIENTED_EDGE('',*,*,#14856,.T.);
#21520=ORIENTED_EDGE('',*,*,#14849,.T.);
#21521=ORIENTED_EDGE('',*,*,#15011,.T.);
#21522=ORIENTED_EDGE('',*,*,#15012,.T.);
#21523=ORIENTED_EDGE('',*,*,#15011,.F.);
#21524=ORIENTED_EDGE('',*,*,#14852,.T.);
#21525=ORIENTED_EDGE('',*,*,#14853,.T.);
#21526=ORIENTED_EDGE('',*,*,#15013,.F.);
#21527=ORIENTED_EDGE('',*,*,#14864,.T.);
#21528=ORIENTED_EDGE('',*,*,#14858,.T.);
#21529=ORIENTED_EDGE('',*,*,#14861,.T.);
#21530=ORIENTED_EDGE('',*,*,#15014,.F.);
#21531=ORIENTED_EDGE('',*,*,#14872,.T.);
#21532=ORIENTED_EDGE('',*,*,#14866,.T.);
#21533=ORIENTED_EDGE('',*,*,#14869,.T.);
#21534=ORIENTED_EDGE('',*,*,#15015,.F.);
#21535=ORIENTED_EDGE('',*,*,#14880,.T.);
#21536=ORIENTED_EDGE('',*,*,#14874,.T.);
#21537=ORIENTED_EDGE('',*,*,#14877,.T.);
#21538=ORIENTED_EDGE('',*,*,#15016,.F.);
#21539=ORIENTED_EDGE('',*,*,#14888,.T.);
#21540=ORIENTED_EDGE('',*,*,#14882,.T.);
#21541=ORIENTED_EDGE('',*,*,#14885,.T.);
#21542=ORIENTED_EDGE('',*,*,#15017,.F.);
#21543=ORIENTED_EDGE('',*,*,#14896,.T.);
#21544=ORIENTED_EDGE('',*,*,#14890,.T.);
#21545=ORIENTED_EDGE('',*,*,#14893,.T.);
#21546=ORIENTED_EDGE('',*,*,#15018,.F.);
#21547=ORIENTED_EDGE('',*,*,#14904,.T.);
#21548=ORIENTED_EDGE('',*,*,#14898,.T.);
#21549=ORIENTED_EDGE('',*,*,#14901,.T.);
#21550=ORIENTED_EDGE('',*,*,#15019,.F.);
#21551=ORIENTED_EDGE('',*,*,#14912,.T.);
#21552=ORIENTED_EDGE('',*,*,#14906,.T.);
#21553=ORIENTED_EDGE('',*,*,#14909,.T.);
#21554=ORIENTED_EDGE('',*,*,#15020,.F.);
#21555=ORIENTED_EDGE('',*,*,#14920,.T.);
#21556=ORIENTED_EDGE('',*,*,#14914,.T.);
#21557=ORIENTED_EDGE('',*,*,#14917,.T.);
#21558=ORIENTED_EDGE('',*,*,#15021,.F.);
#21559=ORIENTED_EDGE('',*,*,#14928,.T.);
#21560=ORIENTED_EDGE('',*,*,#14922,.T.);
#21561=ORIENTED_EDGE('',*,*,#14925,.T.);
#21562=ORIENTED_EDGE('',*,*,#15022,.F.);
#21563=ORIENTED_EDGE('',*,*,#14936,.T.);
#21564=ORIENTED_EDGE('',*,*,#14930,.T.);
#21565=ORIENTED_EDGE('',*,*,#14933,.T.);
#21566=ORIENTED_EDGE('',*,*,#15023,.F.);
#21567=ORIENTED_EDGE('',*,*,#14944,.T.);
#21568=ORIENTED_EDGE('',*,*,#14938,.T.);
#21569=ORIENTED_EDGE('',*,*,#14941,.T.);
#21570=ORIENTED_EDGE('',*,*,#15024,.F.);
#21571=ORIENTED_EDGE('',*,*,#14952,.T.);
#21572=ORIENTED_EDGE('',*,*,#14946,.T.);
#21573=ORIENTED_EDGE('',*,*,#14949,.T.);
#21574=ORIENTED_EDGE('',*,*,#15025,.F.);
#21575=ORIENTED_EDGE('',*,*,#14960,.T.);
#21576=ORIENTED_EDGE('',*,*,#14954,.T.);
#21577=ORIENTED_EDGE('',*,*,#14957,.T.);
#21578=ORIENTED_EDGE('',*,*,#15026,.F.);
#21579=ORIENTED_EDGE('',*,*,#14968,.T.);
#21580=ORIENTED_EDGE('',*,*,#14962,.T.);
#21581=ORIENTED_EDGE('',*,*,#14965,.T.);
#21582=ORIENTED_EDGE('',*,*,#15027,.F.);
#21583=ORIENTED_EDGE('',*,*,#14976,.T.);
#21584=ORIENTED_EDGE('',*,*,#14970,.T.);
#21585=ORIENTED_EDGE('',*,*,#14973,.T.);
#21586=ORIENTED_EDGE('',*,*,#15028,.F.);
#21587=ORIENTED_EDGE('',*,*,#14984,.T.);
#21588=ORIENTED_EDGE('',*,*,#14978,.T.);
#21589=ORIENTED_EDGE('',*,*,#14981,.T.);
#21590=ORIENTED_EDGE('',*,*,#15029,.F.);
#21591=ORIENTED_EDGE('',*,*,#14992,.T.);
#21592=ORIENTED_EDGE('',*,*,#14986,.T.);
#21593=ORIENTED_EDGE('',*,*,#14989,.T.);
#21594=ORIENTED_EDGE('',*,*,#15030,.F.);
#21595=ORIENTED_EDGE('',*,*,#15031,.T.);
#21596=ORIENTED_EDGE('',*,*,#15032,.T.);
#21597=ORIENTED_EDGE('',*,*,#15033,.T.);
#21598=ORIENTED_EDGE('',*,*,#15034,.F.);
#21599=ORIENTED_EDGE('',*,*,#15033,.F.);
#21600=ORIENTED_EDGE('',*,*,#15035,.F.);
#21601=ORIENTED_EDGE('',*,*,#15036,.T.);
#21602=ORIENTED_EDGE('',*,*,#15037,.F.);
#21603=ORIENTED_EDGE('',*,*,#15038,.F.);
#21604=ORIENTED_EDGE('',*,*,#15036,.F.);
#21605=ORIENTED_EDGE('',*,*,#15039,.F.);
#21606=ORIENTED_EDGE('',*,*,#15031,.F.);
#21607=ORIENTED_EDGE('',*,*,#15032,.F.);
#21608=ORIENTED_EDGE('',*,*,#15039,.T.);
#21609=ORIENTED_EDGE('',*,*,#15035,.T.);
#21610=ORIENTED_EDGE('',*,*,#15040,.F.);
#21611=ORIENTED_EDGE('',*,*,#15041,.T.);
#21612=ORIENTED_EDGE('',*,*,#14857,.T.);
#21613=ORIENTED_EDGE('',*,*,#15010,.T.);
#21614=ORIENTED_EDGE('',*,*,#14846,.T.);
#21615=ORIENTED_EDGE('',*,*,#14848,.T.);
#21616=ORIENTED_EDGE('',*,*,#15009,.T.);
#21617=ORIENTED_EDGE('',*,*,#14838,.T.);
#21618=ORIENTED_EDGE('',*,*,#14840,.T.);
#21619=ORIENTED_EDGE('',*,*,#15008,.T.);
#21620=ORIENTED_EDGE('',*,*,#14830,.T.);
#21621=ORIENTED_EDGE('',*,*,#14832,.T.);
#21622=ORIENTED_EDGE('',*,*,#15007,.T.);
#21623=ORIENTED_EDGE('',*,*,#14822,.T.);
#21624=ORIENTED_EDGE('',*,*,#14824,.T.);
#21625=ORIENTED_EDGE('',*,*,#15006,.T.);
#21626=ORIENTED_EDGE('',*,*,#14814,.T.);
#21627=ORIENTED_EDGE('',*,*,#14816,.T.);
#21628=ORIENTED_EDGE('',*,*,#15005,.T.);
#21629=ORIENTED_EDGE('',*,*,#14806,.T.);
#21630=ORIENTED_EDGE('',*,*,#14808,.T.);
#21631=ORIENTED_EDGE('',*,*,#15004,.T.);
#21632=ORIENTED_EDGE('',*,*,#14798,.T.);
#21633=ORIENTED_EDGE('',*,*,#14800,.T.);
#21634=ORIENTED_EDGE('',*,*,#15003,.T.);
#21635=ORIENTED_EDGE('',*,*,#14790,.T.);
#21636=ORIENTED_EDGE('',*,*,#14792,.T.);
#21637=ORIENTED_EDGE('',*,*,#15002,.T.);
#21638=ORIENTED_EDGE('',*,*,#14782,.T.);
#21639=ORIENTED_EDGE('',*,*,#14784,.T.);
#21640=ORIENTED_EDGE('',*,*,#15001,.T.);
#21641=ORIENTED_EDGE('',*,*,#14774,.T.);
#21642=ORIENTED_EDGE('',*,*,#14776,.T.);
#21643=ORIENTED_EDGE('',*,*,#15000,.T.);
#21644=ORIENTED_EDGE('',*,*,#14766,.T.);
#21645=ORIENTED_EDGE('',*,*,#14768,.T.);
#21646=ORIENTED_EDGE('',*,*,#14999,.T.);
#21647=ORIENTED_EDGE('',*,*,#14758,.T.);
#21648=ORIENTED_EDGE('',*,*,#14760,.T.);
#21649=ORIENTED_EDGE('',*,*,#14998,.T.);
#21650=ORIENTED_EDGE('',*,*,#14750,.T.);
#21651=ORIENTED_EDGE('',*,*,#14752,.T.);
#21652=ORIENTED_EDGE('',*,*,#14997,.T.);
#21653=ORIENTED_EDGE('',*,*,#14742,.T.);
#21654=ORIENTED_EDGE('',*,*,#14744,.T.);
#21655=ORIENTED_EDGE('',*,*,#14996,.T.);
#21656=ORIENTED_EDGE('',*,*,#14734,.T.);
#21657=ORIENTED_EDGE('',*,*,#14736,.T.);
#21658=ORIENTED_EDGE('',*,*,#14995,.T.);
#21659=ORIENTED_EDGE('',*,*,#14726,.T.);
#21660=ORIENTED_EDGE('',*,*,#14728,.T.);
#21661=ORIENTED_EDGE('',*,*,#14994,.T.);
#21662=ORIENTED_EDGE('',*,*,#14718,.T.);
#21663=ORIENTED_EDGE('',*,*,#14720,.T.);
#21664=ORIENTED_EDGE('',*,*,#15034,.T.);
#21665=ORIENTED_EDGE('',*,*,#15037,.T.);
#21666=ORIENTED_EDGE('',*,*,#15038,.T.);
#21667=ORIENTED_EDGE('',*,*,#15030,.T.);
#21668=ORIENTED_EDGE('',*,*,#14991,.T.);
#21669=ORIENTED_EDGE('',*,*,#14993,.T.);
#21670=ORIENTED_EDGE('',*,*,#15029,.T.);
#21671=ORIENTED_EDGE('',*,*,#14983,.T.);
#21672=ORIENTED_EDGE('',*,*,#14985,.T.);
#21673=ORIENTED_EDGE('',*,*,#15028,.T.);
#21674=ORIENTED_EDGE('',*,*,#14975,.T.);
#21675=ORIENTED_EDGE('',*,*,#14977,.T.);
#21676=ORIENTED_EDGE('',*,*,#15027,.T.);
#21677=ORIENTED_EDGE('',*,*,#14967,.T.);
#21678=ORIENTED_EDGE('',*,*,#14969,.T.);
#21679=ORIENTED_EDGE('',*,*,#15026,.T.);
#21680=ORIENTED_EDGE('',*,*,#14959,.T.);
#21681=ORIENTED_EDGE('',*,*,#14961,.T.);
#21682=ORIENTED_EDGE('',*,*,#15025,.T.);
#21683=ORIENTED_EDGE('',*,*,#14951,.T.);
#21684=ORIENTED_EDGE('',*,*,#14953,.T.);
#21685=ORIENTED_EDGE('',*,*,#15024,.T.);
#21686=ORIENTED_EDGE('',*,*,#14943,.T.);
#21687=ORIENTED_EDGE('',*,*,#14945,.T.);
#21688=ORIENTED_EDGE('',*,*,#15023,.T.);
#21689=ORIENTED_EDGE('',*,*,#14935,.T.);
#21690=ORIENTED_EDGE('',*,*,#14937,.T.);
#21691=ORIENTED_EDGE('',*,*,#15022,.T.);
#21692=ORIENTED_EDGE('',*,*,#14927,.T.);
#21693=ORIENTED_EDGE('',*,*,#14929,.T.);
#21694=ORIENTED_EDGE('',*,*,#15021,.T.);
#21695=ORIENTED_EDGE('',*,*,#14919,.T.);
#21696=ORIENTED_EDGE('',*,*,#14921,.T.);
#21697=ORIENTED_EDGE('',*,*,#15020,.T.);
#21698=ORIENTED_EDGE('',*,*,#14911,.T.);
#21699=ORIENTED_EDGE('',*,*,#14913,.T.);
#21700=ORIENTED_EDGE('',*,*,#15019,.T.);
#21701=ORIENTED_EDGE('',*,*,#14903,.T.);
#21702=ORIENTED_EDGE('',*,*,#14905,.T.);
#21703=ORIENTED_EDGE('',*,*,#15018,.T.);
#21704=ORIENTED_EDGE('',*,*,#14895,.T.);
#21705=ORIENTED_EDGE('',*,*,#14897,.T.);
#21706=ORIENTED_EDGE('',*,*,#15017,.T.);
#21707=ORIENTED_EDGE('',*,*,#14887,.T.);
#21708=ORIENTED_EDGE('',*,*,#14889,.T.);
#21709=ORIENTED_EDGE('',*,*,#15016,.T.);
#21710=ORIENTED_EDGE('',*,*,#14879,.T.);
#21711=ORIENTED_EDGE('',*,*,#14881,.T.);
#21712=ORIENTED_EDGE('',*,*,#15015,.T.);
#21713=ORIENTED_EDGE('',*,*,#14871,.T.);
#21714=ORIENTED_EDGE('',*,*,#14873,.T.);
#21715=ORIENTED_EDGE('',*,*,#15014,.T.);
#21716=ORIENTED_EDGE('',*,*,#14863,.T.);
#21717=ORIENTED_EDGE('',*,*,#14865,.T.);
#21718=ORIENTED_EDGE('',*,*,#15013,.T.);
#21719=ORIENTED_EDGE('',*,*,#14855,.T.);
#21720=ORIENTED_EDGE('',*,*,#15041,.F.);
#21721=ORIENTED_EDGE('',*,*,#15042,.T.);
#21722=ORIENTED_EDGE('',*,*,#15043,.F.);
#21723=ORIENTED_EDGE('',*,*,#15042,.F.);
#21724=ORIENTED_EDGE('',*,*,#15044,.F.);
#21725=ORIENTED_EDGE('',*,*,#15045,.T.);
#21726=ORIENTED_EDGE('',*,*,#15046,.T.);
#21727=ORIENTED_EDGE('',*,*,#15047,.F.);
#21728=ORIENTED_EDGE('',*,*,#15048,.F.);
#21729=ORIENTED_EDGE('',*,*,#15049,.T.);
#21730=ORIENTED_EDGE('',*,*,#15050,.T.);
#21731=ORIENTED_EDGE('',*,*,#15045,.F.);
#21732=ORIENTED_EDGE('',*,*,#15051,.F.);
#21733=ORIENTED_EDGE('',*,*,#15052,.T.);
#21734=ORIENTED_EDGE('',*,*,#15053,.T.);
#21735=ORIENTED_EDGE('',*,*,#15049,.F.);
#21736=ORIENTED_EDGE('',*,*,#15054,.F.);
#21737=ORIENTED_EDGE('',*,*,#15055,.T.);
#21738=ORIENTED_EDGE('',*,*,#15056,.T.);
#21739=ORIENTED_EDGE('',*,*,#15052,.F.);
#21740=ORIENTED_EDGE('',*,*,#15057,.F.);
#21741=ORIENTED_EDGE('',*,*,#15058,.T.);
#21742=ORIENTED_EDGE('',*,*,#15059,.T.);
#21743=ORIENTED_EDGE('',*,*,#15055,.F.);
#21744=ORIENTED_EDGE('',*,*,#15060,.F.);
#21745=ORIENTED_EDGE('',*,*,#15047,.T.);
#21746=ORIENTED_EDGE('',*,*,#15061,.T.);
#21747=ORIENTED_EDGE('',*,*,#15058,.F.);
#21748=ORIENTED_EDGE('',*,*,#15061,.F.);
#21749=ORIENTED_EDGE('',*,*,#15046,.F.);
#21750=ORIENTED_EDGE('',*,*,#15050,.F.);
#21751=ORIENTED_EDGE('',*,*,#15053,.F.);
#21752=ORIENTED_EDGE('',*,*,#15056,.F.);
#21753=ORIENTED_EDGE('',*,*,#15059,.F.);
#21754=ORIENTED_EDGE('',*,*,#15043,.T.);
#21755=ORIENTED_EDGE('',*,*,#15062,.F.);
#21756=ORIENTED_EDGE('',*,*,#14590,.F.);
#21757=ORIENTED_EDGE('',*,*,#15063,.T.);
#21758=ORIENTED_EDGE('',*,*,#15062,.T.);
#21759=ORIENTED_EDGE('',*,*,#15063,.F.);
#21760=ORIENTED_EDGE('',*,*,#14641,.T.);
#21761=ORIENTED_EDGE('',*,*,#14706,.T.);
#21762=ORIENTED_EDGE('',*,*,#15064,.F.);
#21763=ORIENTED_EDGE('',*,*,#14712,.T.);
#21764=ORIENTED_EDGE('',*,*,#15065,.F.);
#21765=ORIENTED_EDGE('',*,*,#15066,.T.);
#21766=ORIENTED_EDGE('',*,*,#14703,.T.);
#21767=ORIENTED_EDGE('',*,*,#15064,.T.);
#21768=ORIENTED_EDGE('',*,*,#14704,.T.);
#21769=ORIENTED_EDGE('',*,*,#15066,.F.);
#21770=ORIENTED_EDGE('',*,*,#15012,.F.);
#21771=ORIENTED_EDGE('',*,*,#15065,.T.);
#21772=ORIENTED_EDGE('',*,*,#15040,.T.);
#21773=ORIENTED_EDGE('',*,*,#15044,.T.);
#21774=ORIENTED_EDGE('',*,*,#15060,.T.);
#21775=ORIENTED_EDGE('',*,*,#15057,.T.);
#21776=ORIENTED_EDGE('',*,*,#15054,.T.);
#21777=ORIENTED_EDGE('',*,*,#15051,.T.);
#21778=ORIENTED_EDGE('',*,*,#15048,.T.);
#21779=CONICAL_SURFACE('',#23498,0.495606601717798,1.17809724509618);
#21780=CONICAL_SURFACE('',#23502,0.495606601717798,1.17809724509618);
#21781=CONICAL_SURFACE('',#23506,0.495606601717798,1.17809724509618);
#21782=CONICAL_SURFACE('',#23510,0.495606601717798,1.17809724509618);
#21783=CONICAL_SURFACE('',#23515,0.55,0.785398163397448);
#21784=CONICAL_SURFACE('',#23518,0.55,0.785398163397448);
#21785=CONICAL_SURFACE('',#23528,0.589393398282202,0.392699081698717);
#21786=CONICAL_SURFACE('',#23531,0.589393398282202,0.392699081698717);
#21787=CONICAL_SURFACE('',#23534,0.589393398282202,0.392699081698717);
#21788=CONICAL_SURFACE('',#23538,0.589393398282202,0.392699081698717);
#21789=CONICAL_SURFACE('',#23549,0.55,0.785398163397448);
#21790=CONICAL_SURFACE('',#23552,0.545606601717798,1.17809724509617);
#21791=CONICAL_SURFACE('',#23556,0.545606601717798,1.17809724509617);
#21792=CONICAL_SURFACE('',#23560,0.545606601717798,1.17809724509617);
#21793=CONICAL_SURFACE('',#23564,0.545606601717798,1.17809724509617);
#21794=CONICAL_SURFACE('',#23567,0.575,0.785398163397449);
#21795=CONICAL_SURFACE('',#23570,0.575,0.785398163397449);
#21796=CONICAL_SURFACE('',#23582,0.589393398282202,0.392699081698719);
#21797=CONICAL_SURFACE('',#23584,0.589393398282202,0.392699081698719);
#21798=CONICAL_SURFACE('',#23586,0.589393398282202,0.392699081698719);
#21799=CONICAL_SURFACE('',#23590,0.589393398282202,0.392699081698719);
#21800=CONICAL_SURFACE('',#23593,0.575,0.785398163397449);
#21801=CONICAL_SURFACE('',#23595,0.575,0.785398163397449);
#21802=CONICAL_SURFACE('',#23596,0.565,0.785398163397452);
#21803=CONICAL_SURFACE('',#23601,0.565,0.785398163397452);
#21804=CONICAL_SURFACE('',#23606,0.565,0.785398163397452);
#21805=CONICAL_SURFACE('',#23611,0.565,0.785398163397452);
#21806=CONICAL_SURFACE('',#23616,0.515,0.785398163397445);
#21807=CONICAL_SURFACE('',#23621,0.515,0.785398163397449);
#21808=CONICAL_SURFACE('',#23626,0.515,0.785398163397452);
#21809=CONICAL_SURFACE('',#23631,0.2875,0.321750554396636);
#21810=CONICAL_SURFACE('',#23635,0.2875,0.785398163397439);
#21811=CONICAL_SURFACE('',#23638,0.2875,0.321750554396642);
#21812=CONICAL_SURFACE('',#23642,0.2875,0.78539816339745);
#21813=CONICAL_SURFACE('',#23645,0.2875,0.321750554396636);
#21814=CONICAL_SURFACE('',#23649,0.2875,0.785398163397439);
#21815=CONICAL_SURFACE('',#23652,0.342499999999999,0.321750554396636);
#21816=CONICAL_SURFACE('',#23656,0.342499999999999,0.785398163397437);
#21817=CONICAL_SURFACE('',#23659,0.342499999999999,0.321750554396636);
#21818=CONICAL_SURFACE('',#23663,0.342499999999999,0.785398163397437);
#21819=CONICAL_SURFACE('',#23666,0.342499999999999,0.321750554396636);
#21820=CONICAL_SURFACE('',#23670,0.342499999999999,0.785398163397437);
#21821=CONICAL_SURFACE('',#23673,0.342499999999999,0.321750554396636);
#21822=CONICAL_SURFACE('',#23677,0.342499999999999,0.785398163397437);
#21823=CONICAL_SURFACE('',#23681,0.55,0.785398163397448);
#21824=CONICAL_SURFACE('',#23689,0.515606601717798,1.17809724509616);
#21825=CONICAL_SURFACE('',#23693,0.515606601717797,1.17809724509619);
#21826=CONICAL_SURFACE('',#23697,0.56,0.785398163397454);
#21827=CONICAL_SURFACE('',#23717,0.589393398282201,0.392699081698744);
#21828=CONICAL_SURFACE('',#23720,0.589393398282202,0.39269908169875);
#21829=CONICAL_SURFACE('',#23724,0.56,0.785398163397454);
#21830=CONICAL_SURFACE('',#23731,0.589393398282202,0.392699081698749);
#21831=CONICAL_SURFACE('',#23735,0.589393398282201,0.392699081698732);
#21832=CONICAL_SURFACE('',#23738,0.56,0.785398163397454);
#21833=CONICAL_SURFACE('',#23746,0.515606601717797,1.17809724509618);
#21834=CONICAL_SURFACE('',#23749,0.515606601717798,1.17809724509616);
#21835=CONICAL_SURFACE('',#23753,0.56,0.785398163397454);
#21836=CONICAL_SURFACE('',#23766,3.315,0.785398163397444);
#21837=CONICAL_SURFACE('',#23770,3.79,0.785398163397448);
#21838=CONICAL_SURFACE('',#23775,3.315,0.785398163397444);
#21839=CONICAL_SURFACE('',#23778,0.185,0.785398163397448);
#21840=CONICAL_SURFACE('',#23783,0.185,0.785398163397444);
#21841=CONICAL_SURFACE('',#23784,0.185,0.785398163397456);
#21842=CONICAL_SURFACE('',#23789,0.185,0.785398163397452);
#21843=CONICAL_SURFACE('',#23790,0.185,0.785398163397448);
#21844=CONICAL_SURFACE('',#23795,0.185,0.785398163397444);
#21845=CONICAL_SURFACE('',#23796,0.42,0.785398163397452);
#21846=CONICAL_SURFACE('',#23800,0.419999999999999,0.785398163397452);
#21847=CONICAL_SURFACE('',#23804,0.42,0.785398163397447);
#21848=CONICAL_SURFACE('',#23808,0.459393398282203,1.17809724509617);
#21849=CONICAL_SURFACE('',#23811,0.455,0.785398163397442);
#21850=CONICAL_SURFACE('',#23815,0.415606601717798,0.392699081698719);
#21851=CONICAL_SURFACE('',#23820,0.2025,1.02974425867666);
#21852=CONICAL_SURFACE('',#23821,0.1275,1.02974425867665);
#21853=CONICAL_SURFACE('',#23825,0.305,0.785398163397446);
#21854=CONICAL_SURFACE('',#23826,0.1275,1.02974425867665);
#21855=CONICAL_SURFACE('',#23830,0.305,0.785398163397448);
#21856=CONICAL_SURFACE('',#23831,0.1275,1.02974425867665);
#21857=CONICAL_SURFACE('',#23835,0.305,0.785398163397446);
#21858=CONICAL_SURFACE('',#23836,0.43,0.558599315343562);
#21859=CONICAL_SURFACE('',#23837,0.429999999999999,0.558599315343561);
#21860=CONICAL_SURFACE('',#23838,0.430000000000001,0.558599315343561);
#21861=CONICAL_SURFACE('',#23839,0.0775000000000001,1.02974425867665);
#21862=CONICAL_SURFACE('',#23843,0.205,0.785398163397448);
#21863=CONICAL_SURFACE('',#23844,0.0775000000000001,1.02974425867665);
#21864=CONICAL_SURFACE('',#23848,0.205000000000001,0.785398163397448);
#21865=CONICAL_SURFACE('',#23849,0.0775000000000006,1.02974425867665);
#21866=CONICAL_SURFACE('',#23853,0.205,0.785398163397446);
#21867=CONICAL_SURFACE('',#23857,0.515606601717798,1.17809724509616);
#21868=CONICAL_SURFACE('',#23861,0.515606601717798,1.17809724509617);
#21869=CONICAL_SURFACE('',#23865,0.515606601717798,1.17809724509617);
#21870=CONICAL_SURFACE('',#23869,0.515606601717797,1.17809724509618);
#21871=CONICAL_SURFACE('',#23874,0.56,0.78539816339745);
#21872=CONICAL_SURFACE('',#23877,0.56,0.78539816339745);
#21873=CONICAL_SURFACE('',#23885,0.589393398282202,0.392699081698734);
#21874=CONICAL_SURFACE('',#23889,0.589393398282202,0.392699081698736);
#21875=CONICAL_SURFACE('',#23892,0.589393398282202,0.392699081698712);
#21876=CONICAL_SURFACE('',#23895,0.589393398282202,0.392699081698734);
#21877=CONICAL_SURFACE('',#23904,0.56,0.785398163397448);
#21878=CONICAL_SURFACE('',#23906,0.589393398282202,0.392699081698733);
#21879=CONICAL_SURFACE('',#23909,0.589393398282202,0.392699081698719);
#21880=CONICAL_SURFACE('',#23912,0.589393398282202,0.392699081698719);
#21881=CONICAL_SURFACE('',#23916,0.589393398282202,0.392699081698712);
#21882=CONICAL_SURFACE('',#23921,0.56,0.78539816339745);
#21883=CONICAL_SURFACE('',#23924,0.56,0.78539816339745);
#21884=CONICAL_SURFACE('',#23926,3.79,0.785398163397448);
#21885=CONICAL_SURFACE('',#23931,0.515606601717798,1.17809724509616);
#21886=CONICAL_SURFACE('',#23934,0.515606601717797,1.17809724509619);
#21887=CONICAL_SURFACE('',#23937,0.515606601717798,1.17809724509617);
#21888=CONICAL_SURFACE('',#23941,0.515606601717798,1.17809724509617);
#21889=CONICAL_SURFACE('',#23946,0.56,0.785398163397448);
#21890=CONICAL_SURFACE('',#23950,3.315,0.785398163397448);
#21891=CONICAL_SURFACE('',#23956,3.3543933982822,1.17809724509617);
#21892=CONICAL_SURFACE('',#23958,3.325,0.785398163397446);
#21893=CONICAL_SURFACE('',#23960,3.3106066017178,0.392699081698723);
#21894=CONICAL_SURFACE('',#23961,0.1025,1.02974425867666);
#21895=CONICAL_SURFACE('',#23965,0.255,0.785398163397448);
#21896=CONICAL_SURFACE('',#23966,0.1025,1.02974425867666);
#21897=CONICAL_SURFACE('',#23970,0.255,0.785398163397446);
#21898=CONICAL_SURFACE('',#23971,0.1025,1.02974425867666);
#21899=CONICAL_SURFACE('',#23975,0.255,0.785398163397446);
#21900=CONICAL_SURFACE('',#23976,0.56,0.785398163397448);
#21901=CONICAL_SURFACE('',#23978,0.56,0.785398163397448);
#21902=CONICAL_SURFACE('',#23984,4.0106066017178,0.392699081698746);
#21903=CONICAL_SURFACE('',#23991,4.025,0.785398163397446);
#21904=CONICAL_SURFACE('',#23993,4.0106066017178,0.392699081698729);
#21905=CONICAL_SURFACE('',#23995,4.025,0.785398163397446);
#21906=CONICAL_SURFACE('',#23997,4.0543933982822,1.17809724509616);
#21907=CONICAL_SURFACE('',#24004,4.7456066017178,1.17809724509618);
#21908=CONICAL_SURFACE('',#24006,4.775,0.785398163397446);
#21909=CONICAL_SURFACE('',#24008,4.0543933982822,1.17809724509617);
#21910=CONICAL_SURFACE('',#24012,4.7893933982822,0.392699081698714);
#21911=CONICAL_SURFACE('',#24018,4.7456066017178,1.17809724509618);
#21912=CONICAL_SURFACE('',#24020,4.775,0.785398163397446);
#21913=CONICAL_SURFACE('',#24022,4.7893933982822,0.392699081698714);
#21914=CONICAL_SURFACE('',#24023,0.0774999999999997,1.02974425867665);
#21915=CONICAL_SURFACE('',#24027,0.205,0.785398163397449);
#21916=CONICAL_SURFACE('',#24028,0.0774999999999997,1.02974425867665);
#21917=CONICAL_SURFACE('',#24032,0.204999999999999,0.785398163397447);
#21918=CONICAL_SURFACE('',#24033,0.0774999999999997,1.02974425867665);
#21919=CONICAL_SURFACE('',#24037,0.205,0.785398163397449);
#21920=CONICAL_SURFACE('',#24039,0.185,0.785398163397452);
#21921=CONICAL_SURFACE('',#24053,0.185,0.785398163397452);
#21922=CONICAL_SURFACE('',#24063,0.185,0.785398163397444);
#21923=CONICAL_SURFACE('',#24068,0.185,0.785398163397445);
#21924=CONICAL_SURFACE('',#24069,0.185,0.785398163397444);
#21925=CONICAL_SURFACE('',#24074,0.185,0.785398163397449);
#21926=CONICAL_SURFACE('',#24075,0.185000000000001,0.785398163397452);
#21927=CONICAL_SURFACE('',#24080,0.185000000000001,0.785398163397452);
#21928=CONICAL_SURFACE('',#24081,0.185,0.785398163397444);
#21929=CONICAL_SURFACE('',#24086,0.185,0.785398163397445);
#21930=CONICAL_SURFACE('',#24087,0.185,0.785398163397444);
#21931=CONICAL_SURFACE('',#24092,0.185,0.785398163397445);
#21932=CONICAL_SURFACE('',#24093,4.68,0.785398163397448);
#21933=CONICAL_SURFACE('',#24099,4.68,0.785398163397449);
#21934=CONICAL_SURFACE('',#24100,3.32,0.785398163397449);
#21935=CONICAL_SURFACE('',#24106,3.32,0.785398163397448);
#21936=CONICAL_SURFACE('',#24296,0.045,0.643501108793287);
#21937=CONICAL_SURFACE('',#24310,0.5,0.785398163397451);
#21938=CONICAL_SURFACE('',#24329,0.38,0.785398163397448);
#21939=CONICAL_SURFACE('',#24332,3.725,0.785398163397446);
#21940=CONICAL_SURFACE('',#24340,3.725,0.785398163397446);
#21941=CONICAL_SURFACE('',#24362,0.39,0.785398163397448);
#21942=CONICAL_SURFACE('',#24369,0.39,0.785398163397448);
#21943=CONICAL_SURFACE('',#24375,0.589393398282202,0.392699081698718);
#21944=CONICAL_SURFACE('',#24383,0.58,0.785398163397448);
#21945=CONICAL_SURFACE('',#24385,0.585,0.785398163397445);
#21946=CONICAL_SURFACE('',#24509,0.39,0.785398163397449);
#21947=CONICAL_SURFACE('',#24531,0.240000000000001,0.785398163397452);
#21948=CONICAL_SURFACE('',#24540,0.240000000000001,0.785398163397452);
#21949=CONICAL_SURFACE('',#24548,0.335,0.785398163397444);
#21950=CONICAL_SURFACE('',#24551,0.335,0.785398163397446);
#21951=CONICAL_SURFACE('',#24556,0.185,0.785398163397452);
#21952=CONICAL_SURFACE('',#24560,0.185,0.785398163397455);
#21953=CONICAL_SURFACE('',#24569,0.185,0.785398163397451);
#21954=CONICAL_SURFACE('',#24572,0.335,0.785398163397445);
#21955=CONICAL_SURFACE('',#24575,0.335,0.785398163397444);
#21956=CONICAL_SURFACE('',#24578,0.185,0.785398163397455);
#21957=CONICAL_SURFACE('',#24590,0.305,1.46591938806466);
#21958=CONICAL_SURFACE('',#24594,0.305,1.46591938806466);
#21959=CONICAL_SURFACE('',#24635,0.1,1.27933953231703);
#21960=CONICAL_SURFACE('',#24785,0.18,0.785398163397448);
#21961=CONICAL_SURFACE('',#24788,0.575,0.785398163397448);
#21962=CONICAL_SURFACE('',#24792,0.55,0.785398163397448);
#21963=CONICAL_SURFACE('',#25018,0.2675,0.78539816339745);
#21964=CONICAL_SURFACE('',#25020,0.0577350269189626,1.00599363799961);
#21965=CONICAL_SURFACE('',#25031,0.132,0.785398163397448);
#21966=CONICAL_SURFACE('',#25034,0.155,0.785398163397449);
#21967=CONICAL_SURFACE('',#25349,0.2675,0.78539816339745);
#21968=CONICAL_SURFACE('',#25351,0.0577350269189626,1.00599363799961);
#21969=CONICAL_SURFACE('',#25362,0.132,0.785398163397448);
#21970=CONICAL_SURFACE('',#25365,0.155,0.785398163397449);
#21971=CONICAL_SURFACE('',#25600,0.4175,0.785398163397448);
#21972=CONICAL_SURFACE('',#25602,0.0923760430703401,1.00831422748172);
#21973=CONICAL_SURFACE('',#25613,0.22,0.785398163397448);
#21974=CONICAL_SURFACE('',#25616,0.255,0.785398163397449);
#21975=ADVANCED_FACE('',(#2236),#21779,.T.);
#21976=ADVANCED_FACE('',(#2237),#1448,.T.);
#21977=ADVANCED_FACE('',(#2238),#21780,.T.);
#21978=ADVANCED_FACE('',(#2239),#1449,.T.);
#21979=ADVANCED_FACE('',(#2240),#21781,.T.);
#21980=ADVANCED_FACE('',(#2241),#1450,.T.);
#21981=ADVANCED_FACE('',(#2242),#21782,.T.);
#21982=ADVANCED_FACE('',(#2243),#1451,.T.);
#21983=ADVANCED_FACE('',(#2244),#1452,.T.);
#21984=ADVANCED_FACE('',(#2245),#21783,.T.);
#21985=ADVANCED_FACE('',(#2246),#1453,.T.);
#21986=ADVANCED_FACE('',(#2247),#21784,.T.);
#21987=ADVANCED_FACE('',(#2248,#1277,#1278,#1279,#1280,#1281,#1282,#1283),
#1454,.T.);
#21988=ADVANCED_FACE('',(#2249),#21785,.T.);
#21989=ADVANCED_FACE('',(#2250),#1455,.T.);
#21990=ADVANCED_FACE('',(#2251),#21786,.T.);
#21991=ADVANCED_FACE('',(#2252),#1456,.T.);
#21992=ADVANCED_FACE('',(#2253),#21787,.T.);
#21993=ADVANCED_FACE('',(#2254),#1457,.T.);
#21994=ADVANCED_FACE('',(#2255),#21788,.T.);
#21995=ADVANCED_FACE('',(#2256),#1458,.T.);
#21996=ADVANCED_FACE('',(#2257),#1459,.T.);
#21997=ADVANCED_FACE('',(#2258),#943,.T.);
#21998=ADVANCED_FACE('',(#2259),#1460,.T.);
#21999=ADVANCED_FACE('',(#2260),#944,.T.);
#22000=ADVANCED_FACE('',(#2261),#1461,.T.);
#22001=ADVANCED_FACE('',(#2262),#21789,.T.);
#22002=ADVANCED_FACE('',(#2263),#1462,.T.);
#22003=ADVANCED_FACE('',(#2264),#1463,.T.);
#22004=ADVANCED_FACE('',(#2265),#21790,.T.);
#22005=ADVANCED_FACE('',(#2266),#1464,.T.);
#22006=ADVANCED_FACE('',(#2267),#21791,.T.);
#22007=ADVANCED_FACE('',(#2268),#1465,.T.);
#22008=ADVANCED_FACE('',(#2269),#21792,.T.);
#22009=ADVANCED_FACE('',(#2270),#1466,.T.);
#22010=ADVANCED_FACE('',(#2271),#21793,.T.);
#22011=ADVANCED_FACE('',(#2272),#21794,.T.);
#22012=ADVANCED_FACE('',(#2273),#1467,.T.);
#22013=ADVANCED_FACE('',(#2274),#21795,.T.);
#22014=ADVANCED_FACE('',(#2275),#1468,.T.);
#22015=ADVANCED_FACE('',(#2276,#1284,#1285,#1286,#1287,#1288,#1289,#1290),
#1469,.F.);
#22016=ADVANCED_FACE('',(#2277),#1470,.T.);
#22017=ADVANCED_FACE('',(#2278),#21796,.T.);
#22018=ADVANCED_FACE('',(#2279),#1471,.T.);
#22019=ADVANCED_FACE('',(#2280),#21797,.T.);
#22020=ADVANCED_FACE('',(#2281),#1472,.T.);
#22021=ADVANCED_FACE('',(#2282),#21798,.T.);
#22022=ADVANCED_FACE('',(#2283),#1473,.T.);
#22023=ADVANCED_FACE('',(#2284),#21799,.T.);
#22024=ADVANCED_FACE('',(#2285),#21800,.T.);
#22025=ADVANCED_FACE('',(#2286),#1474,.T.);
#22026=ADVANCED_FACE('',(#2287),#21801,.T.);
#22027=ADVANCED_FACE('',(#2288),#21802,.F.);
#22028=ADVANCED_FACE('',(#2289),#945,.F.);
#22029=ADVANCED_FACE('',(#2290),#21803,.F.);
#22030=ADVANCED_FACE('',(#2291),#946,.F.);
#22031=ADVANCED_FACE('',(#2292),#21804,.F.);
#22032=ADVANCED_FACE('',(#2293),#947,.F.);
#22033=ADVANCED_FACE('',(#2294),#21805,.F.);
#22034=ADVANCED_FACE('',(#2295),#948,.F.);
#22035=ADVANCED_FACE('',(#2296),#21806,.F.);
#22036=ADVANCED_FACE('',(#2297),#949,.F.);
#22037=ADVANCED_FACE('',(#2298),#21807,.F.);
#22038=ADVANCED_FACE('',(#2299),#950,.F.);
#22039=ADVANCED_FACE('',(#2300),#21808,.F.);
#22040=ADVANCED_FACE('',(#2301),#951,.F.);
#22041=ADVANCED_FACE('',(#2302),#21809,.F.);
#22042=ADVANCED_FACE('',(#2303),#952,.F.);
#22043=ADVANCED_FACE('',(#2304),#21810,.F.);
#22044=ADVANCED_FACE('',(#2305,#1291),#1475,.F.);
#22045=ADVANCED_FACE('',(#2306),#21811,.F.);
#22046=ADVANCED_FACE('',(#2307),#953,.F.);
#22047=ADVANCED_FACE('',(#2308),#21812,.F.);
#22048=ADVANCED_FACE('',(#2309,#1292),#1476,.F.);
#22049=ADVANCED_FACE('',(#2310),#21813,.F.);
#22050=ADVANCED_FACE('',(#2311),#954,.F.);
#22051=ADVANCED_FACE('',(#2312),#21814,.F.);
#22052=ADVANCED_FACE('',(#2313,#1293),#1477,.F.);
#22053=ADVANCED_FACE('',(#2314),#21815,.F.);
#22054=ADVANCED_FACE('',(#2315),#955,.F.);
#22055=ADVANCED_FACE('',(#2316),#21816,.F.);
#22056=ADVANCED_FACE('',(#2317,#1294),#1478,.F.);
#22057=ADVANCED_FACE('',(#2318),#21817,.F.);
#22058=ADVANCED_FACE('',(#2319),#956,.F.);
#22059=ADVANCED_FACE('',(#2320),#21818,.F.);
#22060=ADVANCED_FACE('',(#2321,#1295),#1479,.F.);
#22061=ADVANCED_FACE('',(#2322),#21819,.F.);
#22062=ADVANCED_FACE('',(#2323),#957,.F.);
#22063=ADVANCED_FACE('',(#2324),#21820,.F.);
#22064=ADVANCED_FACE('',(#2325,#1296),#1480,.F.);
#22065=ADVANCED_FACE('',(#2326),#21821,.F.);
#22066=ADVANCED_FACE('',(#2327),#958,.F.);
#22067=ADVANCED_FACE('',(#2328),#21822,.F.);
#22068=ADVANCED_FACE('',(#2329,#1297),#1481,.F.);
#22069=ADVANCED_FACE('',(#2330),#1482,.T.);
#22070=ADVANCED_FACE('',(#2331),#21823,.T.);
#22071=ADVANCED_FACE('',(#2332),#1483,.T.);
#22072=ADVANCED_FACE('',(#2333),#959,.T.);
#22073=ADVANCED_FACE('',(#2334),#960,.T.);
#22074=ADVANCED_FACE('',(#2335),#1484,.T.);
#22075=ADVANCED_FACE('',(#2336),#1485,.T.);
#22076=ADVANCED_FACE('',(#2337),#1486,.T.);
#22077=ADVANCED_FACE('',(#2338),#21824,.T.);
#22078=ADVANCED_FACE('',(#2339),#1487,.T.);
#22079=ADVANCED_FACE('',(#2340),#21825,.T.);
#22080=ADVANCED_FACE('',(#2341),#1488,.T.);
#22081=ADVANCED_FACE('',(#2342),#21826,.T.);
#22082=ADVANCED_FACE('',(#2343),#1489,.T.);
#22083=ADVANCED_FACE('',(#2344),#1490,.T.);
#22084=ADVANCED_FACE('',(#2345,#1298,#1299,#1300,#1301,#1302,#1303,#1304),
#1491,.F.);
#22085=ADVANCED_FACE('',(#2346),#1492,.T.);
#22086=ADVANCED_FACE('',(#2347,#1305,#1306,#1307),#1493,.T.);
#22087=ADVANCED_FACE('',(#2348),#1494,.T.);
#22088=ADVANCED_FACE('',(#2349),#1495,.T.);
#22089=ADVANCED_FACE('',(#2350),#1496,.T.);
#22090=ADVANCED_FACE('',(#2351),#21827,.T.);
#22091=ADVANCED_FACE('',(#2352),#1497,.T.);
#22092=ADVANCED_FACE('',(#2353),#21828,.T.);
#22093=ADVANCED_FACE('',(#2354),#1498,.T.);
#22094=ADVANCED_FACE('',(#2355),#21829,.T.);
#22095=ADVANCED_FACE('',(#2356),#1499,.T.);
#22096=ADVANCED_FACE('',(#2357),#1500,.T.);
#22097=ADVANCED_FACE('',(#2358),#1501,.T.);
#22098=ADVANCED_FACE('',(#2359),#1502,.T.);
#22099=ADVANCED_FACE('',(#2360),#1503,.T.);
#22100=ADVANCED_FACE('',(#2361),#1504,.T.);
#22101=ADVANCED_FACE('',(#2362),#21830,.T.);
#22102=ADVANCED_FACE('',(#2363),#1505,.T.);
#22103=ADVANCED_FACE('',(#2364),#21831,.T.);
#22104=ADVANCED_FACE('',(#2365),#21832,.T.);
#22105=ADVANCED_FACE('',(#2366),#1506,.T.);
#22106=ADVANCED_FACE('',(#2367),#1507,.T.);
#22107=ADVANCED_FACE('',(#2368),#961,.T.);
#22108=ADVANCED_FACE('',(#2369),#1508,.T.);
#22109=ADVANCED_FACE('',(#2370),#1509,.T.);
#22110=ADVANCED_FACE('',(#2371),#1510,.T.);
#22111=ADVANCED_FACE('',(#2372),#21833,.T.);
#22112=ADVANCED_FACE('',(#2373),#1511,.T.);
#22113=ADVANCED_FACE('',(#2374),#21834,.T.);
#22114=ADVANCED_FACE('',(#2375),#1512,.T.);
#22115=ADVANCED_FACE('',(#2376),#21835,.T.);
#22116=ADVANCED_FACE('',(#2377),#1513,.T.);
#22117=ADVANCED_FACE('',(#2378,#1308,#1309,#1310,#1311,#1312,#1313,#1314,
#1315,#1316,#1317),#1514,.T.);
#22118=ADVANCED_FACE('',(#2379),#21836,.F.);
#22119=ADVANCED_FACE('',(#2380),#962,.F.);
#22120=ADVANCED_FACE('',(#2381),#21837,.F.);
#22121=ADVANCED_FACE('',(#2382),#963,.F.);
#22122=ADVANCED_FACE('',(#2383),#21838,.F.);
#22123=ADVANCED_FACE('',(#2384,#1318),#1515,.F.);
#22124=ADVANCED_FACE('',(#2385),#21839,.F.);
#22125=ADVANCED_FACE('',(#2386),#964,.F.);
#22126=ADVANCED_FACE('',(#2387),#21840,.F.);
#22127=ADVANCED_FACE('',(#2388),#21841,.F.);
#22128=ADVANCED_FACE('',(#2389),#965,.F.);
#22129=ADVANCED_FACE('',(#2390),#21842,.F.);
#22130=ADVANCED_FACE('',(#2391),#21843,.F.);
#22131=ADVANCED_FACE('',(#2392),#966,.F.);
#22132=ADVANCED_FACE('',(#2393),#21844,.F.);
#22133=ADVANCED_FACE('',(#2394),#21845,.F.);
#22134=ADVANCED_FACE('',(#2395),#967,.F.);
#22135=ADVANCED_FACE('',(#2396),#21846,.F.);
#22136=ADVANCED_FACE('',(#2397),#968,.F.);
#22137=ADVANCED_FACE('',(#2398),#21847,.F.);
#22138=ADVANCED_FACE('',(#2399),#969,.F.);
#22139=ADVANCED_FACE('',(#2400),#21848,.F.);
#22140=ADVANCED_FACE('',(#2401),#21849,.F.);
#22141=ADVANCED_FACE('',(#2402,#1319),#1516,.T.);
#22142=ADVANCED_FACE('',(#2403),#21850,.F.);
#22143=ADVANCED_FACE('',(#2404),#970,.F.);
#22144=ADVANCED_FACE('',(#2405),#21851,.F.);
#22145=ADVANCED_FACE('',(#2406),#21852,.F.);
#22146=ADVANCED_FACE('',(#2407),#971,.F.);
#22147=ADVANCED_FACE('',(#2408),#21853,.F.);
#22148=ADVANCED_FACE('',(#2409),#21854,.F.);
#22149=ADVANCED_FACE('',(#2410),#972,.F.);
#22150=ADVANCED_FACE('',(#2411),#21855,.F.);
#22151=ADVANCED_FACE('',(#2412),#21856,.F.);
#22152=ADVANCED_FACE('',(#2413),#973,.F.);
#22153=ADVANCED_FACE('',(#2414),#21857,.F.);
#22154=ADVANCED_FACE('',(#2415),#21858,.F.);
#22155=ADVANCED_FACE('',(#2416),#21859,.F.);
#22156=ADVANCED_FACE('',(#2417),#21860,.F.);
#22157=ADVANCED_FACE('',(#2418),#21861,.F.);
#22158=ADVANCED_FACE('',(#2419),#974,.F.);
#22159=ADVANCED_FACE('',(#2420),#21862,.F.);
#22160=ADVANCED_FACE('',(#2421),#21863,.F.);
#22161=ADVANCED_FACE('',(#2422),#975,.F.);
#22162=ADVANCED_FACE('',(#2423),#21864,.F.);
#22163=ADVANCED_FACE('',(#2424),#21865,.F.);
#22164=ADVANCED_FACE('',(#2425),#976,.F.);
#22165=ADVANCED_FACE('',(#2426),#21866,.F.);
#22166=ADVANCED_FACE('',(#2427),#1517,.T.);
#22167=ADVANCED_FACE('',(#2428),#977,.T.);
#22168=ADVANCED_FACE('',(#2429),#21867,.T.);
#22169=ADVANCED_FACE('',(#2430),#1518,.T.);
#22170=ADVANCED_FACE('',(#2431),#21868,.T.);
#22171=ADVANCED_FACE('',(#2432),#1519,.T.);
#22172=ADVANCED_FACE('',(#2433),#21869,.T.);
#22173=ADVANCED_FACE('',(#2434),#1520,.T.);
#22174=ADVANCED_FACE('',(#2435),#21870,.T.);
#22175=ADVANCED_FACE('',(#2436),#1521,.T.);
#22176=ADVANCED_FACE('',(#2437),#1522,.T.);
#22177=ADVANCED_FACE('',(#2438),#21871,.T.);
#22178=ADVANCED_FACE('',(#2439),#1523,.T.);
#22179=ADVANCED_FACE('',(#2440),#21872,.T.);
#22180=ADVANCED_FACE('',(#2441,#1320,#1321,#1322,#1323),#1524,.F.);
#22181=ADVANCED_FACE('',(#2442),#1525,.T.);
#22182=ADVANCED_FACE('',(#2443),#21873,.T.);
#22183=ADVANCED_FACE('',(#2444),#1526,.T.);
#22184=ADVANCED_FACE('',(#2445),#21874,.T.);
#22185=ADVANCED_FACE('',(#2446),#1527,.T.);
#22186=ADVANCED_FACE('',(#2447),#21875,.T.);
#22187=ADVANCED_FACE('',(#2448),#1528,.T.);
#22188=ADVANCED_FACE('',(#2449),#21876,.T.);
#22189=ADVANCED_FACE('',(#2450),#978,.T.);
#22190=ADVANCED_FACE('',(#2451),#1529,.T.);
#22191=ADVANCED_FACE('',(#2452),#979,.T.);
#22192=ADVANCED_FACE('',(#2453),#1530,.T.);
#22193=ADVANCED_FACE('',(#2454),#21877,.T.);
#22194=ADVANCED_FACE('',(#2455),#1531,.T.);
#22195=ADVANCED_FACE('',(#2456),#21878,.T.);
#22196=ADVANCED_FACE('',(#2457),#1532,.T.);
#22197=ADVANCED_FACE('',(#2458),#21879,.T.);
#22198=ADVANCED_FACE('',(#2459),#1533,.T.);
#22199=ADVANCED_FACE('',(#2460),#21880,.T.);
#22200=ADVANCED_FACE('',(#2461),#1534,.T.);
#22201=ADVANCED_FACE('',(#2462),#21881,.T.);
#22202=ADVANCED_FACE('',(#2463),#1535,.T.);
#22203=ADVANCED_FACE('',(#2464),#1536,.T.);
#22204=ADVANCED_FACE('',(#2465),#21882,.T.);
#22205=ADVANCED_FACE('',(#2466),#1537,.T.);
#22206=ADVANCED_FACE('',(#2467),#21883,.T.);
#22207=ADVANCED_FACE('',(#2468),#21884,.F.);
#22208=ADVANCED_FACE('',(#2469),#980,.F.);
#22209=ADVANCED_FACE('',(#2470),#21885,.T.);
#22210=ADVANCED_FACE('',(#2471),#1538,.T.);
#22211=ADVANCED_FACE('',(#2472),#21886,.T.);
#22212=ADVANCED_FACE('',(#2473),#1539,.T.);
#22213=ADVANCED_FACE('',(#2474),#21887,.T.);
#22214=ADVANCED_FACE('',(#2475),#1540,.T.);
#22215=ADVANCED_FACE('',(#2476),#21888,.T.);
#22216=ADVANCED_FACE('',(#2477),#1541,.T.);
#22217=ADVANCED_FACE('',(#2478),#1542,.T.);
#22218=ADVANCED_FACE('',(#2479),#21889,.T.);
#22219=ADVANCED_FACE('',(#2480),#1543,.T.);
#22220=ADVANCED_FACE('',(#2481,#1324),#1544,.T.);
#22221=ADVANCED_FACE('',(#2482),#21890,.F.);
#22222=ADVANCED_FACE('',(#2483),#981,.F.);
#22223=ADVANCED_FACE('',(#2484,#1325),#1545,.F.);
#22224=ADVANCED_FACE('',(#2485),#21891,.F.);
#22225=ADVANCED_FACE('',(#2486),#21892,.F.);
#22226=ADVANCED_FACE('',(#2487),#21893,.F.);
#22227=ADVANCED_FACE('',(#2488),#21894,.F.);
#22228=ADVANCED_FACE('',(#2489),#982,.F.);
#22229=ADVANCED_FACE('',(#2490),#21895,.F.);
#22230=ADVANCED_FACE('',(#2491),#21896,.F.);
#22231=ADVANCED_FACE('',(#2492),#983,.F.);
#22232=ADVANCED_FACE('',(#2493),#21897,.F.);
#22233=ADVANCED_FACE('',(#2494),#21898,.F.);
#22234=ADVANCED_FACE('',(#2495),#984,.F.);
#22235=ADVANCED_FACE('',(#2496),#21899,.F.);
#22236=ADVANCED_FACE('',(#2497),#21900,.T.);
#22237=ADVANCED_FACE('',(#2498),#1546,.T.);
#22238=ADVANCED_FACE('',(#2499),#21901,.T.);
#22239=ADVANCED_FACE('',(#2500),#1547,.T.);
#22240=ADVANCED_FACE('',(#2501),#985,.T.);
#22241=ADVANCED_FACE('',(#2502),#1548,.T.);
#22242=ADVANCED_FACE('',(#2503),#986,.T.);
#22243=ADVANCED_FACE('',(#2504),#21902,.F.);
#22244=ADVANCED_FACE('',(#2505),#987,.F.);
#22245=ADVANCED_FACE('',(#2506),#21903,.F.);
#22246=ADVANCED_FACE('',(#2507),#21904,.F.);
#22247=ADVANCED_FACE('',(#2508),#21905,.F.);
#22248=ADVANCED_FACE('',(#2509),#21906,.F.);
#22249=ADVANCED_FACE('',(#2510,#1326,#1327,#1328,#1329),#1549,.T.);
#22250=ADVANCED_FACE('',(#2511),#21907,.T.);
#22251=ADVANCED_FACE('',(#2512),#21908,.T.);
#22252=ADVANCED_FACE('',(#2513),#21909,.F.);
#22253=ADVANCED_FACE('',(#2514,#1330),#1550,.T.);
#22254=ADVANCED_FACE('',(#2515),#21910,.T.);
#22255=ADVANCED_FACE('',(#2516),#988,.T.);
#22256=ADVANCED_FACE('',(#2517),#21911,.T.);
#22257=ADVANCED_FACE('',(#2518),#21912,.T.);
#22258=ADVANCED_FACE('',(#2519),#21913,.T.);
#22259=ADVANCED_FACE('',(#2520),#21914,.F.);
#22260=ADVANCED_FACE('',(#2521),#989,.F.);
#22261=ADVANCED_FACE('',(#2522),#21915,.F.);
#22262=ADVANCED_FACE('',(#2523),#21916,.F.);
#22263=ADVANCED_FACE('',(#2524),#990,.F.);
#22264=ADVANCED_FACE('',(#2525),#21917,.F.);
#22265=ADVANCED_FACE('',(#2526),#21918,.F.);
#22266=ADVANCED_FACE('',(#2527),#991,.F.);
#22267=ADVANCED_FACE('',(#2528),#21919,.F.);
#22268=ADVANCED_FACE('',(#2529),#21920,.F.);
#22269=ADVANCED_FACE('',(#2530),#992,.F.);
#22270=ADVANCED_FACE('',(#2531,#1331,#1332,#1333,#1334,#1335,#1336,#1337),
#1551,.T.);
#22271=ADVANCED_FACE('',(#2532),#21921,.F.);
#22272=ADVANCED_FACE('',(#2533,#1338,#1339,#1340,#1341,#1342,#1343,#1344),
#1552,.T.);
#22273=ADVANCED_FACE('',(#2534),#21922,.F.);
#22274=ADVANCED_FACE('',(#2535),#993,.F.);
#22275=ADVANCED_FACE('',(#2536),#21923,.F.);
#22276=ADVANCED_FACE('',(#2537),#21924,.F.);
#22277=ADVANCED_FACE('',(#2538),#994,.F.);
#22278=ADVANCED_FACE('',(#2539),#21925,.F.);
#22279=ADVANCED_FACE('',(#2540),#21926,.F.);
#22280=ADVANCED_FACE('',(#2541),#995,.F.);
#22281=ADVANCED_FACE('',(#2542),#21927,.F.);
#22282=ADVANCED_FACE('',(#2543),#21928,.F.);
#22283=ADVANCED_FACE('',(#2544),#996,.F.);
#22284=ADVANCED_FACE('',(#2545),#21929,.F.);
#22285=ADVANCED_FACE('',(#2546),#21930,.F.);
#22286=ADVANCED_FACE('',(#2547),#997,.F.);
#22287=ADVANCED_FACE('',(#2548),#21931,.F.);
#22288=ADVANCED_FACE('',(#2549),#21932,.T.);
#22289=ADVANCED_FACE('',(#2550),#998,.T.);
#22290=ADVANCED_FACE('',(#2551),#21933,.T.);
#22291=ADVANCED_FACE('',(#2552),#21934,.F.);
#22292=ADVANCED_FACE('',(#2553),#999,.F.);
#22293=ADVANCED_FACE('',(#2554),#21935,.F.);
#22294=ADVANCED_FACE('',(#2555),#1000,.T.);
#22295=ADVANCED_FACE('',(#2556),#1001,.T.);
#22296=ADVANCED_FACE('',(#2557),#1002,.T.);
#22297=ADVANCED_FACE('',(#2558),#1003,.T.);
#22298=ADVANCED_FACE('',(#2559),#1004,.T.);
#22299=ADVANCED_FACE('',(#2560),#1005,.T.);
#22300=ADVANCED_FACE('',(#2561),#1006,.T.);
#22301=ADVANCED_FACE('',(#2562),#1007,.T.);
#22302=ADVANCED_FACE('',(#2563),#1008,.T.);
#22303=ADVANCED_FACE('',(#2564),#1009,.T.);
#22304=ADVANCED_FACE('',(#2565),#1010,.T.);
#22305=ADVANCED_FACE('',(#2566),#1011,.T.);
#22306=ADVANCED_FACE('',(#2567),#1012,.T.);
#22307=ADVANCED_FACE('',(#2568),#1013,.T.);
#22308=ADVANCED_FACE('',(#2569),#1014,.T.);
#22309=ADVANCED_FACE('',(#2570),#1015,.T.);
#22310=ADVANCED_FACE('',(#2571),#1016,.T.);
#22311=ADVANCED_FACE('',(#2572),#1017,.T.);
#22312=ADVANCED_FACE('',(#2573),#1018,.T.);
#22313=ADVANCED_FACE('',(#2574),#1019,.T.);
#22314=ADVANCED_FACE('',(#2575),#1020,.T.);
#22315=ADVANCED_FACE('',(#2576),#363,.F.);
#22316=ADVANCED_FACE('',(#2577),#1553,.T.);
#22317=ADVANCED_FACE('',(#2578),#1021,.T.);
#22318=ADVANCED_FACE('',(#2579),#364,.F.);
#22319=ADVANCED_FACE('',(#2580),#1022,.F.);
#22320=ADVANCED_FACE('',(#2581),#1023,.F.);
#22321=ADVANCED_FACE('',(#2582),#1024,.F.);
#22322=ADVANCED_FACE('',(#2583),#1025,.F.);
#22323=ADVANCED_FACE('',(#2584),#1554,.F.);
#22324=ADVANCED_FACE('',(#2585),#1555,.F.);
#22325=ADVANCED_FACE('',(#2586),#1556,.F.);
#22326=ADVANCED_FACE('',(#2587),#1557,.T.);
#22327=ADVANCED_FACE('',(#2588),#1558,.F.);
#22328=ADVANCED_FACE('',(#2589),#1559,.F.);
#22329=ADVANCED_FACE('',(#2590),#1560,.F.);
#22330=ADVANCED_FACE('',(#2591),#1561,.T.);
#22331=ADVANCED_FACE('',(#2592),#1562,.F.);
#22332=ADVANCED_FACE('',(#2593),#1563,.F.);
#22333=ADVANCED_FACE('',(#2594),#1564,.F.);
#22334=ADVANCED_FACE('',(#2595),#1565,.T.);
#22335=ADVANCED_FACE('',(#2596),#1566,.F.);
#22336=ADVANCED_FACE('',(#2597),#1567,.F.);
#22337=ADVANCED_FACE('',(#2598),#1568,.F.);
#22338=ADVANCED_FACE('',(#2599),#1569,.T.);
#22339=ADVANCED_FACE('',(#2600),#1570,.F.);
#22340=ADVANCED_FACE('',(#2601),#1571,.F.);
#22341=ADVANCED_FACE('',(#2602),#1572,.F.);
#22342=ADVANCED_FACE('',(#2603),#1573,.T.);
#22343=ADVANCED_FACE('',(#2604),#1574,.F.);
#22344=ADVANCED_FACE('',(#2605),#1575,.F.);
#22345=ADVANCED_FACE('',(#2606),#1576,.F.);
#22346=ADVANCED_FACE('',(#2607),#1577,.T.);
#22347=ADVANCED_FACE('',(#2608),#1578,.F.);
#22348=ADVANCED_FACE('',(#2609),#1579,.F.);
#22349=ADVANCED_FACE('',(#2610),#1580,.F.);
#22350=ADVANCED_FACE('',(#2611),#1581,.T.);
#22351=ADVANCED_FACE('',(#2612),#1582,.F.);
#22352=ADVANCED_FACE('',(#2613),#1583,.F.);
#22353=ADVANCED_FACE('',(#2614),#1584,.F.);
#22354=ADVANCED_FACE('',(#2615),#1585,.T.);
#22355=ADVANCED_FACE('',(#2616),#1586,.F.);
#22356=ADVANCED_FACE('',(#2617),#1587,.F.);
#22357=ADVANCED_FACE('',(#2618),#1588,.F.);
#22358=ADVANCED_FACE('',(#2619),#1589,.T.);
#22359=ADVANCED_FACE('',(#2620),#1590,.F.);
#22360=ADVANCED_FACE('',(#2621),#1591,.F.);
#22361=ADVANCED_FACE('',(#2622),#1592,.F.);
#22362=ADVANCED_FACE('',(#2623),#1593,.T.);
#22363=ADVANCED_FACE('',(#2624),#1594,.F.);
#22364=ADVANCED_FACE('',(#2625),#1595,.F.);
#22365=ADVANCED_FACE('',(#2626),#1596,.F.);
#22366=ADVANCED_FACE('',(#2627),#1597,.T.);
#22367=ADVANCED_FACE('',(#2628),#1598,.F.);
#22368=ADVANCED_FACE('',(#2629),#1599,.F.);
#22369=ADVANCED_FACE('',(#2630),#1600,.F.);
#22370=ADVANCED_FACE('',(#2631),#1601,.T.);
#22371=ADVANCED_FACE('',(#2632),#1602,.F.);
#22372=ADVANCED_FACE('',(#2633),#1603,.F.);
#22373=ADVANCED_FACE('',(#2634),#1604,.F.);
#22374=ADVANCED_FACE('',(#2635),#1605,.T.);
#22375=ADVANCED_FACE('',(#2636),#1606,.F.);
#22376=ADVANCED_FACE('',(#2637),#1607,.F.);
#22377=ADVANCED_FACE('',(#2638),#1608,.F.);
#22378=ADVANCED_FACE('',(#2639),#1609,.T.);
#22379=ADVANCED_FACE('',(#2640),#1610,.F.);
#22380=ADVANCED_FACE('',(#2641),#1611,.F.);
#22381=ADVANCED_FACE('',(#2642),#1612,.F.);
#22382=ADVANCED_FACE('',(#2643),#1613,.T.);
#22383=ADVANCED_FACE('',(#2644),#1614,.F.);
#22384=ADVANCED_FACE('',(#2645),#1615,.F.);
#22385=ADVANCED_FACE('',(#2646),#1616,.F.);
#22386=ADVANCED_FACE('',(#2647),#1617,.T.);
#22387=ADVANCED_FACE('',(#2648),#1618,.F.);
#22388=ADVANCED_FACE('',(#2649),#1619,.F.);
#22389=ADVANCED_FACE('',(#2650),#1620,.F.);
#22390=ADVANCED_FACE('',(#2651),#1621,.T.);
#22391=ADVANCED_FACE('',(#2652),#1622,.F.);
#22392=ADVANCED_FACE('',(#2653),#1623,.F.);
#22393=ADVANCED_FACE('',(#2654),#1624,.F.);
#22394=ADVANCED_FACE('',(#2655),#1625,.T.);
#22395=ADVANCED_FACE('',(#2656),#1626,.F.);
#22396=ADVANCED_FACE('',(#2657),#1627,.F.);
#22397=ADVANCED_FACE('',(#2658),#1628,.F.);
#22398=ADVANCED_FACE('',(#2659),#1629,.T.);
#22399=ADVANCED_FACE('',(#2660),#1630,.F.);
#22400=ADVANCED_FACE('',(#2661),#1631,.F.);
#22401=ADVANCED_FACE('',(#2662),#1632,.F.);
#22402=ADVANCED_FACE('',(#2663),#1633,.T.);
#22403=ADVANCED_FACE('',(#2664),#1634,.F.);
#22404=ADVANCED_FACE('',(#2665),#1635,.F.);
#22405=ADVANCED_FACE('',(#2666),#1636,.F.);
#22406=ADVANCED_FACE('',(#2667),#1637,.T.);
#22407=ADVANCED_FACE('',(#2668),#1638,.F.);
#22408=ADVANCED_FACE('',(#2669),#1639,.F.);
#22409=ADVANCED_FACE('',(#2670),#1640,.F.);
#22410=ADVANCED_FACE('',(#2671),#1641,.T.);
#22411=ADVANCED_FACE('',(#2672),#1642,.F.);
#22412=ADVANCED_FACE('',(#2673),#1643,.F.);
#22413=ADVANCED_FACE('',(#2674),#1644,.F.);
#22414=ADVANCED_FACE('',(#2675),#1645,.T.);
#22415=ADVANCED_FACE('',(#2676),#1646,.F.);
#22416=ADVANCED_FACE('',(#2677),#1647,.F.);
#22417=ADVANCED_FACE('',(#2678),#1648,.F.);
#22418=ADVANCED_FACE('',(#2679),#1649,.T.);
#22419=ADVANCED_FACE('',(#2680),#1026,.T.);
#22420=ADVANCED_FACE('',(#2681),#21936,.T.);
#22421=ADVANCED_FACE('',(#2682),#1650,.T.);
#22422=ADVANCED_FACE('',(#2683,#1345),#1651,.F.);
#22423=ADVANCED_FACE('',(#2684),#1027,.F.);
#22424=ADVANCED_FACE('',(#2685,#1346,#1347,#1348,#1349,#1350,#1351,#1352,
#1353,#1354,#1355,#1356,#1357,#1358,#1359,#1360,#1361,#1362,#1363,#1364,
#1365,#1366,#1367,#1368),#1028,.T.);
#22425=ADVANCED_FACE('',(#2686,#1369),#1652,.T.);
#22426=ADVANCED_FACE('',(#2687),#1029,.T.);
#22427=ADVANCED_FACE('',(#2688),#21937,.T.);
#22428=ADVANCED_FACE('',(#2689,#1370),#1653,.T.);
#22429=ADVANCED_FACE('',(#2690),#1654,.T.);
#22430=ADVANCED_FACE('',(#2691),#1655,.T.);
#22431=ADVANCED_FACE('',(#2692),#1656,.T.);
#22432=ADVANCED_FACE('',(#2693),#1657,.T.);
#22433=ADVANCED_FACE('',(#2694),#1658,.T.);
#22434=ADVANCED_FACE('',(#2695),#1659,.T.);
#22435=ADVANCED_FACE('',(#2696,#1371),#1660,.T.);
#22436=ADVANCED_FACE('',(#2697,#1372,#1373,#1374,#1375,#1376),#1661,.F.);
#22437=ADVANCED_FACE('',(#2698),#1662,.T.);
#22438=ADVANCED_FACE('',(#2699),#1663,.T.);
#22439=ADVANCED_FACE('',(#2700),#1664,.T.);
#22440=ADVANCED_FACE('',(#2701),#1665,.T.);
#22441=ADVANCED_FACE('',(#2702,#1377,#1378,#1379,#1380,#1381),#1666,.T.);
#22442=ADVANCED_FACE('',(#2703),#1667,.T.);
#22443=ADVANCED_FACE('',(#2704),#21938,.T.);
#22444=ADVANCED_FACE('',(#2705),#1030,.T.);
#22445=ADVANCED_FACE('',(#2706),#21939,.T.);
#22446=ADVANCED_FACE('',(#2707),#1031,.T.);
#22447=ADVANCED_FACE('',(#2708),#1668,.T.);
#22448=ADVANCED_FACE('',(#2709),#21940,.T.);
#22449=ADVANCED_FACE('',(#2710),#1669,.T.);
#22450=ADVANCED_FACE('',(#2711),#1032,.T.);
#22451=ADVANCED_FACE('',(#2712,#1382),#1670,.F.);
#22452=ADVANCED_FACE('',(#2713,#1383),#1671,.F.);
#22453=ADVANCED_FACE('',(#2714),#1033,.T.);
#22454=ADVANCED_FACE('',(#2715),#1034,.T.);
#22455=ADVANCED_FACE('',(#2716,#1384),#1672,.F.);
#22456=ADVANCED_FACE('',(#2717,#1385),#1673,.F.);
#22457=ADVANCED_FACE('',(#2718),#1035,.T.);
#22458=ADVANCED_FACE('',(#2719),#21941,.T.);
#22459=ADVANCED_FACE('',(#2720),#1036,.T.);
#22460=ADVANCED_FACE('',(#2721,#1386),#1674,.T.);
#22461=ADVANCED_FACE('',(#2722),#21942,.T.);
#22462=ADVANCED_FACE('',(#2723,#1387),#1675,.T.);
#22463=ADVANCED_FACE('',(#2724),#1037,.F.);
#22464=ADVANCED_FACE('',(#2725),#21943,.T.);
#22465=ADVANCED_FACE('',(#2726),#1038,.T.);
#22466=ADVANCED_FACE('',(#2727),#21944,.T.);
#22467=ADVANCED_FACE('',(#2728),#21945,.T.);
#22468=ADVANCED_FACE('',(#2729,#1388),#1676,.T.);
#22469=ADVANCED_FACE('',(#2730),#1677,.F.);
#22470=ADVANCED_FACE('',(#2731),#1678,.F.);
#22471=ADVANCED_FACE('',(#2732),#1679,.F.);
#22472=ADVANCED_FACE('',(#2733),#1680,.T.);
#22473=ADVANCED_FACE('',(#2734),#1681,.F.);
#22474=ADVANCED_FACE('',(#2735),#1682,.F.);
#22475=ADVANCED_FACE('',(#2736),#1683,.F.);
#22476=ADVANCED_FACE('',(#2737),#1684,.T.);
#22477=ADVANCED_FACE('',(#2738),#1685,.F.);
#22478=ADVANCED_FACE('',(#2739),#1686,.F.);
#22479=ADVANCED_FACE('',(#2740),#1687,.F.);
#22480=ADVANCED_FACE('',(#2741),#1688,.T.);
#22481=ADVANCED_FACE('',(#2742),#1689,.F.);
#22482=ADVANCED_FACE('',(#2743),#1690,.F.);
#22483=ADVANCED_FACE('',(#2744),#1691,.F.);
#22484=ADVANCED_FACE('',(#2745),#1692,.T.);
#22485=ADVANCED_FACE('',(#2746),#1693,.F.);
#22486=ADVANCED_FACE('',(#2747),#1694,.F.);
#22487=ADVANCED_FACE('',(#2748),#1695,.F.);
#22488=ADVANCED_FACE('',(#2749),#1696,.T.);
#22489=ADVANCED_FACE('',(#2750),#1697,.F.);
#22490=ADVANCED_FACE('',(#2751),#1698,.F.);
#22491=ADVANCED_FACE('',(#2752),#1699,.F.);
#22492=ADVANCED_FACE('',(#2753),#1700,.T.);
#22493=ADVANCED_FACE('',(#2754),#1701,.F.);
#22494=ADVANCED_FACE('',(#2755),#1702,.F.);
#22495=ADVANCED_FACE('',(#2756),#1703,.F.);
#22496=ADVANCED_FACE('',(#2757),#1704,.T.);
#22497=ADVANCED_FACE('',(#2758),#1705,.F.);
#22498=ADVANCED_FACE('',(#2759),#1706,.F.);
#22499=ADVANCED_FACE('',(#2760),#1707,.F.);
#22500=ADVANCED_FACE('',(#2761),#1708,.T.);
#22501=ADVANCED_FACE('',(#2762),#1709,.F.);
#22502=ADVANCED_FACE('',(#2763),#1710,.F.);
#22503=ADVANCED_FACE('',(#2764),#1711,.F.);
#22504=ADVANCED_FACE('',(#2765),#1712,.T.);
#22505=ADVANCED_FACE('',(#2766),#1713,.F.);
#22506=ADVANCED_FACE('',(#2767),#1714,.F.);
#22507=ADVANCED_FACE('',(#2768),#1715,.F.);
#22508=ADVANCED_FACE('',(#2769),#1716,.T.);
#22509=ADVANCED_FACE('',(#2770),#1717,.F.);
#22510=ADVANCED_FACE('',(#2771),#1718,.F.);
#22511=ADVANCED_FACE('',(#2772),#1719,.F.);
#22512=ADVANCED_FACE('',(#2773),#1720,.T.);
#22513=ADVANCED_FACE('',(#2774),#1721,.F.);
#22514=ADVANCED_FACE('',(#2775),#1722,.F.);
#22515=ADVANCED_FACE('',(#2776),#1723,.F.);
#22516=ADVANCED_FACE('',(#2777),#1724,.T.);
#22517=ADVANCED_FACE('',(#2778),#1725,.F.);
#22518=ADVANCED_FACE('',(#2779),#1726,.F.);
#22519=ADVANCED_FACE('',(#2780),#1727,.F.);
#22520=ADVANCED_FACE('',(#2781),#1728,.T.);
#22521=ADVANCED_FACE('',(#2782),#1729,.F.);
#22522=ADVANCED_FACE('',(#2783),#1730,.F.);
#22523=ADVANCED_FACE('',(#2784),#1731,.F.);
#22524=ADVANCED_FACE('',(#2785),#1732,.T.);
#22525=ADVANCED_FACE('',(#2786),#1733,.F.);
#22526=ADVANCED_FACE('',(#2787),#1734,.F.);
#22527=ADVANCED_FACE('',(#2788),#1735,.F.);
#22528=ADVANCED_FACE('',(#2789),#1736,.T.);
#22529=ADVANCED_FACE('',(#2790),#1737,.F.);
#22530=ADVANCED_FACE('',(#2791),#1738,.F.);
#22531=ADVANCED_FACE('',(#2792),#1739,.F.);
#22532=ADVANCED_FACE('',(#2793),#1740,.T.);
#22533=ADVANCED_FACE('',(#2794),#1741,.F.);
#22534=ADVANCED_FACE('',(#2795),#1742,.F.);
#22535=ADVANCED_FACE('',(#2796),#1743,.F.);
#22536=ADVANCED_FACE('',(#2797),#1744,.T.);
#22537=ADVANCED_FACE('',(#2798),#1745,.F.);
#22538=ADVANCED_FACE('',(#2799),#1746,.F.);
#22539=ADVANCED_FACE('',(#2800),#1747,.F.);
#22540=ADVANCED_FACE('',(#2801),#1748,.T.);
#22541=ADVANCED_FACE('',(#2802),#1039,.T.);
#22542=ADVANCED_FACE('',(#2803),#1040,.F.);
#22543=ADVANCED_FACE('',(#2804,#1389),#1749,.F.);
#22544=ADVANCED_FACE('',(#2805,#1390),#1750,.T.);
#22545=ADVANCED_FACE('',(#2806),#1751,.T.);
#22546=ADVANCED_FACE('',(#2807),#21946,.T.);
#22547=ADVANCED_FACE('',(#2808),#1041,.T.);
#22548=ADVANCED_FACE('',(#2809,#1391),#1752,.T.);
#22549=ADVANCED_FACE('',(#2810,#1392,#1393,#1394,#1395,#1396,#1397,#1398,
#1399,#1400,#1401,#1402,#1403,#1404,#1405,#1406,#1407,#1408),#1042,.T.);
#22550=ADVANCED_FACE('',(#2811,#1409),#1753,.T.);
#22551=ADVANCED_FACE('',(#2812),#1043,.T.);
#22552=ADVANCED_FACE('',(#2813),#1754,.T.);
#22553=ADVANCED_FACE('',(#2814),#1044,.F.);
#22554=ADVANCED_FACE('',(#2815,#1410),#1755,.T.);
#22555=ADVANCED_FACE('',(#2816),#1045,.T.);
#22556=ADVANCED_FACE('',(#2817,#1411),#1756,.T.);
#22557=ADVANCED_FACE('',(#2818),#21947,.F.);
#22558=ADVANCED_FACE('',(#2819),#1046,.F.);
#22559=ADVANCED_FACE('',(#2820,#1412),#1757,.F.);
#22560=ADVANCED_FACE('',(#2821),#21948,.F.);
#22561=ADVANCED_FACE('',(#2822,#1413),#1758,.T.);
#22562=ADVANCED_FACE('',(#2823),#1759,.T.);
#22563=ADVANCED_FACE('',(#2824),#21949,.T.);
#22564=ADVANCED_FACE('',(#2825),#1760,.T.);
#22565=ADVANCED_FACE('',(#2826),#21950,.T.);
#22566=ADVANCED_FACE('',(#2827),#1761,.T.);
#22567=ADVANCED_FACE('',(#2828),#1762,.T.);
#22568=ADVANCED_FACE('',(#2829),#1763,.T.);
#22569=ADVANCED_FACE('',(#2830),#21951,.T.);
#22570=ADVANCED_FACE('',(#2831),#1764,.T.);
#22571=ADVANCED_FACE('',(#2832),#21952,.T.);
#22572=ADVANCED_FACE('',(#2833),#1765,.T.);
#22573=ADVANCED_FACE('',(#2834),#1047,.T.);
#22574=ADVANCED_FACE('',(#2835),#1766,.T.);
#22575=ADVANCED_FACE('',(#2836),#1767,.T.);
#22576=ADVANCED_FACE('',(#2837),#1768,.F.);
#22577=ADVANCED_FACE('',(#2838),#21953,.T.);
#22578=ADVANCED_FACE('',(#2839),#1769,.T.);
#22579=ADVANCED_FACE('',(#2840),#21954,.T.);
#22580=ADVANCED_FACE('',(#2841),#1770,.T.);
#22581=ADVANCED_FACE('',(#2842),#21955,.T.);
#22582=ADVANCED_FACE('',(#2843),#1771,.T.);
#22583=ADVANCED_FACE('',(#2844),#21956,.T.);
#22584=ADVANCED_FACE('',(#2845),#1772,.T.);
#22585=ADVANCED_FACE('',(#2846),#1773,.T.);
#22586=ADVANCED_FACE('',(#2847),#1048,.T.);
#22587=ADVANCED_FACE('',(#2848),#1774,.T.);
#22588=ADVANCED_FACE('',(#2849),#1049,.T.);
#22589=ADVANCED_FACE('',(#2850),#1775,.T.);
#22590=ADVANCED_FACE('',(#2851),#1050,.T.);
#22591=ADVANCED_FACE('',(#2852),#1051,.F.);
#22592=ADVANCED_FACE('',(#2853),#21957,.F.);
#22593=ADVANCED_FACE('',(#2854),#1052,.T.);
#22594=ADVANCED_FACE('',(#2855),#21958,.T.);
#22595=ADVANCED_FACE('',(#2856),#1053,.T.);
#22596=ADVANCED_FACE('',(#2857),#1054,.T.);
#22597=ADVANCED_FACE('',(#2858),#1055,.T.);
#22598=ADVANCED_FACE('',(#2859),#1056,.T.);
#22599=ADVANCED_FACE('',(#2860),#1057,.T.);
#22600=ADVANCED_FACE('',(#2861),#1058,.T.);
#22601=ADVANCED_FACE('',(#2862),#1059,.T.);
#22602=ADVANCED_FACE('',(#2863),#1060,.T.);
#22603=ADVANCED_FACE('',(#2864),#1061,.T.);
#22604=ADVANCED_FACE('',(#2865),#1062,.T.);
#22605=ADVANCED_FACE('',(#2866),#1063,.T.);
#22606=ADVANCED_FACE('',(#2867),#1064,.T.);
#22607=ADVANCED_FACE('',(#2868),#1065,.T.);
#22608=ADVANCED_FACE('',(#2869),#1066,.T.);
#22609=ADVANCED_FACE('',(#2870),#1067,.T.);
#22610=ADVANCED_FACE('',(#2871),#1068,.T.);
#22611=ADVANCED_FACE('',(#2872),#1069,.T.);
#22612=ADVANCED_FACE('',(#2873),#1070,.T.);
#22613=ADVANCED_FACE('',(#2874),#1071,.T.);
#22614=ADVANCED_FACE('',(#2875),#1072,.T.);
#22615=ADVANCED_FACE('',(#2876),#1073,.T.);
#22616=ADVANCED_FACE('',(#2877),#1074,.T.);
#22617=ADVANCED_FACE('',(#2878),#1075,.T.);
#22618=ADVANCED_FACE('',(#2879),#1076,.T.);
#22619=ADVANCED_FACE('',(#2880),#1077,.T.);
#22620=ADVANCED_FACE('',(#2881),#1078,.T.);
#22621=ADVANCED_FACE('',(#2882),#1079,.T.);
#22622=ADVANCED_FACE('',(#2883),#1080,.T.);
#22623=ADVANCED_FACE('',(#2884),#1081,.T.);
#22624=ADVANCED_FACE('',(#2885),#365,.F.);
#22625=ADVANCED_FACE('',(#2886),#1776,.T.);
#22626=ADVANCED_FACE('',(#2887),#1082,.T.);
#22627=ADVANCED_FACE('',(#2888),#366,.F.);
#22628=ADVANCED_FACE('',(#2889),#1083,.T.);
#22629=ADVANCED_FACE('',(#2890),#21959,.F.);
#22630=ADVANCED_FACE('',(#2891),#1777,.F.);
#22631=ADVANCED_FACE('',(#2892),#1778,.F.);
#22632=ADVANCED_FACE('',(#2893),#1779,.F.);
#22633=ADVANCED_FACE('',(#2894),#1780,.T.);
#22634=ADVANCED_FACE('',(#2895),#1781,.F.);
#22635=ADVANCED_FACE('',(#2896),#1782,.F.);
#22636=ADVANCED_FACE('',(#2897),#1783,.F.);
#22637=ADVANCED_FACE('',(#2898),#1784,.T.);
#22638=ADVANCED_FACE('',(#2899),#1785,.F.);
#22639=ADVANCED_FACE('',(#2900),#1786,.F.);
#22640=ADVANCED_FACE('',(#2901),#1787,.F.);
#22641=ADVANCED_FACE('',(#2902),#1788,.T.);
#22642=ADVANCED_FACE('',(#2903),#1789,.F.);
#22643=ADVANCED_FACE('',(#2904),#1790,.F.);
#22644=ADVANCED_FACE('',(#2905),#1791,.F.);
#22645=ADVANCED_FACE('',(#2906),#1792,.T.);
#22646=ADVANCED_FACE('',(#2907),#1793,.F.);
#22647=ADVANCED_FACE('',(#2908),#1794,.F.);
#22648=ADVANCED_FACE('',(#2909),#1795,.F.);
#22649=ADVANCED_FACE('',(#2910),#1796,.T.);
#22650=ADVANCED_FACE('',(#2911),#1797,.F.);
#22651=ADVANCED_FACE('',(#2912),#1798,.F.);
#22652=ADVANCED_FACE('',(#2913),#1799,.F.);
#22653=ADVANCED_FACE('',(#2914),#1800,.T.);
#22654=ADVANCED_FACE('',(#2915),#1801,.F.);
#22655=ADVANCED_FACE('',(#2916),#1802,.F.);
#22656=ADVANCED_FACE('',(#2917),#1803,.F.);
#22657=ADVANCED_FACE('',(#2918),#1804,.T.);
#22658=ADVANCED_FACE('',(#2919),#1805,.F.);
#22659=ADVANCED_FACE('',(#2920),#1806,.F.);
#22660=ADVANCED_FACE('',(#2921),#1807,.F.);
#22661=ADVANCED_FACE('',(#2922),#1808,.T.);
#22662=ADVANCED_FACE('',(#2923),#1809,.F.);
#22663=ADVANCED_FACE('',(#2924),#1810,.F.);
#22664=ADVANCED_FACE('',(#2925),#1811,.F.);
#22665=ADVANCED_FACE('',(#2926),#1812,.T.);
#22666=ADVANCED_FACE('',(#2927),#1813,.F.);
#22667=ADVANCED_FACE('',(#2928),#1814,.F.);
#22668=ADVANCED_FACE('',(#2929),#1815,.F.);
#22669=ADVANCED_FACE('',(#2930),#1816,.T.);
#22670=ADVANCED_FACE('',(#2931),#1817,.F.);
#22671=ADVANCED_FACE('',(#2932),#1818,.F.);
#22672=ADVANCED_FACE('',(#2933),#1819,.F.);
#22673=ADVANCED_FACE('',(#2934),#1820,.T.);
#22674=ADVANCED_FACE('',(#2935),#1821,.F.);
#22675=ADVANCED_FACE('',(#2936),#1822,.F.);
#22676=ADVANCED_FACE('',(#2937),#1823,.F.);
#22677=ADVANCED_FACE('',(#2938),#1824,.T.);
#22678=ADVANCED_FACE('',(#2939),#1825,.F.);
#22679=ADVANCED_FACE('',(#2940),#1826,.F.);
#22680=ADVANCED_FACE('',(#2941),#1827,.F.);
#22681=ADVANCED_FACE('',(#2942),#1828,.T.);
#22682=ADVANCED_FACE('',(#2943),#1829,.F.);
#22683=ADVANCED_FACE('',(#2944),#1830,.F.);
#22684=ADVANCED_FACE('',(#2945),#1831,.F.);
#22685=ADVANCED_FACE('',(#2946),#1832,.T.);
#22686=ADVANCED_FACE('',(#2947),#1833,.F.);
#22687=ADVANCED_FACE('',(#2948),#1834,.F.);
#22688=ADVANCED_FACE('',(#2949),#1835,.F.);
#22689=ADVANCED_FACE('',(#2950),#1836,.T.);
#22690=ADVANCED_FACE('',(#2951),#1837,.F.);
#22691=ADVANCED_FACE('',(#2952),#1838,.F.);
#22692=ADVANCED_FACE('',(#2953),#1839,.F.);
#22693=ADVANCED_FACE('',(#2954),#1840,.T.);
#22694=ADVANCED_FACE('',(#2955),#1841,.F.);
#22695=ADVANCED_FACE('',(#2956),#1842,.F.);
#22696=ADVANCED_FACE('',(#2957),#1843,.F.);
#22697=ADVANCED_FACE('',(#2958),#1844,.T.);
#22698=ADVANCED_FACE('',(#2959),#1845,.F.);
#22699=ADVANCED_FACE('',(#2960),#1846,.F.);
#22700=ADVANCED_FACE('',(#2961),#1847,.F.);
#22701=ADVANCED_FACE('',(#2962),#1848,.T.);
#22702=ADVANCED_FACE('',(#2963),#1849,.F.);
#22703=ADVANCED_FACE('',(#2964),#1850,.F.);
#22704=ADVANCED_FACE('',(#2965),#1851,.F.);
#22705=ADVANCED_FACE('',(#2966),#1852,.T.);
#22706=ADVANCED_FACE('',(#2967),#1853,.F.);
#22707=ADVANCED_FACE('',(#2968),#1854,.F.);
#22708=ADVANCED_FACE('',(#2969),#1855,.F.);
#22709=ADVANCED_FACE('',(#2970),#1856,.T.);
#22710=ADVANCED_FACE('',(#2971),#1857,.F.);
#22711=ADVANCED_FACE('',(#2972),#1858,.F.);
#22712=ADVANCED_FACE('',(#2973),#1859,.F.);
#22713=ADVANCED_FACE('',(#2974),#1860,.T.);
#22714=ADVANCED_FACE('',(#2975),#1861,.F.);
#22715=ADVANCED_FACE('',(#2976),#1862,.F.);
#22716=ADVANCED_FACE('',(#2977),#1863,.F.);
#22717=ADVANCED_FACE('',(#2978),#1864,.T.);
#22718=ADVANCED_FACE('',(#2979),#1865,.F.);
#22719=ADVANCED_FACE('',(#2980),#1866,.F.);
#22720=ADVANCED_FACE('',(#2981),#1867,.F.);
#22721=ADVANCED_FACE('',(#2982),#1868,.T.);
#22722=ADVANCED_FACE('',(#2983),#1869,.F.);
#22723=ADVANCED_FACE('',(#2984),#1870,.F.);
#22724=ADVANCED_FACE('',(#2985),#1871,.F.);
#22725=ADVANCED_FACE('',(#2986),#1872,.T.);
#22726=ADVANCED_FACE('',(#2987),#1873,.T.);
#22727=ADVANCED_FACE('',(#2988),#21960,.T.);
#22728=ADVANCED_FACE('',(#2989,#1414),#1874,.T.);
#22729=ADVANCED_FACE('',(#2990),#21961,.T.);
#22730=ADVANCED_FACE('',(#2991,#1415,#1416,#1417,#1418,#1419,#1420,#1421,
#1422,#1423,#1424,#1425,#1426,#1427,#1428,#1429,#1430,#1431,#1432,#1433,
#1434,#1435,#1436,#1437),#1084,.T.);
#22731=ADVANCED_FACE('',(#2992),#21962,.T.);
#22732=ADVANCED_FACE('',(#2993,#1438),#1875,.T.);
#22733=ADVANCED_FACE('',(#2994),#1085,.T.);
#22734=ADVANCED_FACE('',(#2995),#1086,.T.);
#22735=ADVANCED_FACE('',(#2996),#1087,.T.);
#22736=ADVANCED_FACE('',(#2997),#1088,.T.);
#22737=ADVANCED_FACE('',(#2998),#1089,.T.);
#22738=ADVANCED_FACE('',(#2999),#1090,.T.);
#22739=ADVANCED_FACE('',(#3000),#1091,.T.);
#22740=ADVANCED_FACE('',(#3001),#1092,.T.);
#22741=ADVANCED_FACE('',(#3002),#1093,.T.);
#22742=ADVANCED_FACE('',(#3003),#1094,.T.);
#22743=ADVANCED_FACE('',(#3004),#1095,.T.);
#22744=ADVANCED_FACE('',(#3005),#1096,.T.);
#22745=ADVANCED_FACE('',(#3006),#1097,.T.);
#22746=ADVANCED_FACE('',(#3007),#1098,.T.);
#22747=ADVANCED_FACE('',(#3008),#1099,.T.);
#22748=ADVANCED_FACE('',(#3009),#1100,.T.);
#22749=ADVANCED_FACE('',(#3010),#1101,.T.);
#22750=ADVANCED_FACE('',(#3011),#1102,.T.);
#22751=ADVANCED_FACE('',(#3012),#1103,.T.);
#22752=ADVANCED_FACE('',(#3013),#1104,.T.);
#22753=ADVANCED_FACE('',(#3014),#1105,.T.);
#22754=ADVANCED_FACE('',(#3015),#1106,.T.);
#22755=ADVANCED_FACE('',(#3016),#1107,.T.);
#22756=ADVANCED_FACE('',(#3017),#1108,.T.);
#22757=ADVANCED_FACE('',(#3018),#1109,.T.);
#22758=ADVANCED_FACE('',(#3019),#1110,.T.);
#22759=ADVANCED_FACE('',(#3020),#1111,.T.);
#22760=ADVANCED_FACE('',(#3021),#1112,.T.);
#22761=ADVANCED_FACE('',(#3022),#1113,.T.);
#22762=ADVANCED_FACE('',(#3023),#1876,.F.);
#22763=ADVANCED_FACE('',(#3024),#367,.F.);
#22764=ADVANCED_FACE('',(#3025),#1877,.T.);
#22765=ADVANCED_FACE('',(#3026),#1114,.T.);
#22766=ADVANCED_FACE('',(#3027),#368,.F.);
#22767=ADVANCED_FACE('',(#3028),#1878,.T.);
#22768=ADVANCED_FACE('',(#3029),#1879,.F.);
#22769=ADVANCED_FACE('',(#3030),#1880,.F.);
#22770=ADVANCED_FACE('',(#3031),#1881,.T.);
#22771=ADVANCED_FACE('',(#3032),#1882,.F.);
#22772=ADVANCED_FACE('',(#3033),#1883,.F.);
#22773=ADVANCED_FACE('',(#3034),#1884,.T.);
#22774=ADVANCED_FACE('',(#3035),#1885,.F.);
#22775=ADVANCED_FACE('',(#3036),#1886,.F.);
#22776=ADVANCED_FACE('',(#3037),#1887,.T.);
#22777=ADVANCED_FACE('',(#3038),#1888,.F.);
#22778=ADVANCED_FACE('',(#3039),#1889,.F.);
#22779=ADVANCED_FACE('',(#3040),#1890,.T.);
#22780=ADVANCED_FACE('',(#3041),#1891,.F.);
#22781=ADVANCED_FACE('',(#3042),#1892,.F.);
#22782=ADVANCED_FACE('',(#3043),#1893,.T.);
#22783=ADVANCED_FACE('',(#3044),#1894,.F.);
#22784=ADVANCED_FACE('',(#3045),#1895,.F.);
#22785=ADVANCED_FACE('',(#3046),#1896,.T.);
#22786=ADVANCED_FACE('',(#3047),#1897,.F.);
#22787=ADVANCED_FACE('',(#3048),#1898,.F.);
#22788=ADVANCED_FACE('',(#3049),#1899,.T.);
#22789=ADVANCED_FACE('',(#3050),#1900,.F.);
#22790=ADVANCED_FACE('',(#3051),#1901,.F.);
#22791=ADVANCED_FACE('',(#3052),#1902,.T.);
#22792=ADVANCED_FACE('',(#3053),#1903,.F.);
#22793=ADVANCED_FACE('',(#3054),#1904,.F.);
#22794=ADVANCED_FACE('',(#3055),#1905,.T.);
#22795=ADVANCED_FACE('',(#3056),#1906,.F.);
#22796=ADVANCED_FACE('',(#3057),#1907,.F.);
#22797=ADVANCED_FACE('',(#3058),#1908,.T.);
#22798=ADVANCED_FACE('',(#3059),#1909,.F.);
#22799=ADVANCED_FACE('',(#3060),#1910,.F.);
#22800=ADVANCED_FACE('',(#3061),#1911,.T.);
#22801=ADVANCED_FACE('',(#3062),#1912,.F.);
#22802=ADVANCED_FACE('',(#3063),#1913,.F.);
#22803=ADVANCED_FACE('',(#3064),#1914,.T.);
#22804=ADVANCED_FACE('',(#3065),#1915,.F.);
#22805=ADVANCED_FACE('',(#3066),#1916,.F.);
#22806=ADVANCED_FACE('',(#3067),#1917,.T.);
#22807=ADVANCED_FACE('',(#3068),#1918,.F.);
#22808=ADVANCED_FACE('',(#3069),#1919,.F.);
#22809=ADVANCED_FACE('',(#3070),#1920,.T.);
#22810=ADVANCED_FACE('',(#3071),#1921,.F.);
#22811=ADVANCED_FACE('',(#3072),#1922,.F.);
#22812=ADVANCED_FACE('',(#3073),#1923,.T.);
#22813=ADVANCED_FACE('',(#3074),#1924,.F.);
#22814=ADVANCED_FACE('',(#3075),#1925,.F.);
#22815=ADVANCED_FACE('',(#3076),#1926,.T.);
#22816=ADVANCED_FACE('',(#3077),#1927,.F.);
#22817=ADVANCED_FACE('',(#3078),#1928,.F.);
#22818=ADVANCED_FACE('',(#3079),#1929,.T.);
#22819=ADVANCED_FACE('',(#3080),#1930,.F.);
#22820=ADVANCED_FACE('',(#3081),#1931,.F.);
#22821=ADVANCED_FACE('',(#3082),#1932,.T.);
#22822=ADVANCED_FACE('',(#3083),#1933,.F.);
#22823=ADVANCED_FACE('',(#3084),#1934,.F.);
#22824=ADVANCED_FACE('',(#3085),#1935,.T.);
#22825=ADVANCED_FACE('',(#3086),#1936,.F.);
#22826=ADVANCED_FACE('',(#3087),#1937,.F.);
#22827=ADVANCED_FACE('',(#3088),#1938,.T.);
#22828=ADVANCED_FACE('',(#3089),#1939,.F.);
#22829=ADVANCED_FACE('',(#3090),#1940,.F.);
#22830=ADVANCED_FACE('',(#3091),#1941,.T.);
#22831=ADVANCED_FACE('',(#3092),#1942,.F.);
#22832=ADVANCED_FACE('',(#3093),#1943,.F.);
#22833=ADVANCED_FACE('',(#3094),#1944,.T.);
#22834=ADVANCED_FACE('',(#3095),#1945,.F.);
#22835=ADVANCED_FACE('',(#3096),#1946,.F.);
#22836=ADVANCED_FACE('',(#3097),#1947,.T.);
#22837=ADVANCED_FACE('',(#3098),#1948,.F.);
#22838=ADVANCED_FACE('',(#3099),#1949,.F.);
#22839=ADVANCED_FACE('',(#3100),#1950,.T.);
#22840=ADVANCED_FACE('',(#3101),#1951,.F.);
#22841=ADVANCED_FACE('',(#3102),#1952,.F.);
#22842=ADVANCED_FACE('',(#3103),#1953,.T.);
#22843=ADVANCED_FACE('',(#3104),#1954,.F.);
#22844=ADVANCED_FACE('',(#3105),#1955,.F.);
#22845=ADVANCED_FACE('',(#3106),#1956,.T.);
#22846=ADVANCED_FACE('',(#3107),#1957,.F.);
#22847=ADVANCED_FACE('',(#3108),#1958,.F.);
#22848=ADVANCED_FACE('',(#3109),#1959,.T.);
#22849=ADVANCED_FACE('',(#3110),#1960,.F.);
#22850=ADVANCED_FACE('',(#3111),#1961,.F.);
#22851=ADVANCED_FACE('',(#3112),#1962,.T.);
#22852=ADVANCED_FACE('',(#3113),#1963,.F.);
#22853=ADVANCED_FACE('',(#3114),#1964,.F.);
#22854=ADVANCED_FACE('',(#3115),#1965,.T.);
#22855=ADVANCED_FACE('',(#3116),#1966,.F.);
#22856=ADVANCED_FACE('',(#3117),#1967,.F.);
#22857=ADVANCED_FACE('',(#3118),#1968,.T.);
#22858=ADVANCED_FACE('',(#3119),#1969,.F.);
#22859=ADVANCED_FACE('',(#3120),#1970,.F.);
#22860=ADVANCED_FACE('',(#3121),#1971,.T.);
#22861=ADVANCED_FACE('',(#3122),#1972,.F.);
#22862=ADVANCED_FACE('',(#3123),#1973,.F.);
#22863=ADVANCED_FACE('',(#3124),#1974,.T.);
#22864=ADVANCED_FACE('',(#3125),#1975,.F.);
#22865=ADVANCED_FACE('',(#3126),#1976,.F.);
#22866=ADVANCED_FACE('',(#3127),#1977,.T.);
#22867=ADVANCED_FACE('',(#3128),#1978,.F.);
#22868=ADVANCED_FACE('',(#3129),#1979,.F.);
#22869=ADVANCED_FACE('',(#3130),#1980,.T.);
#22870=ADVANCED_FACE('',(#3131),#1981,.F.);
#22871=ADVANCED_FACE('',(#3132),#1982,.F.);
#22872=ADVANCED_FACE('',(#3133),#1115,.T.);
#22873=ADVANCED_FACE('',(#3134),#1983,.F.);
#22874=ADVANCED_FACE('',(#3135),#1984,.F.);
#22875=ADVANCED_FACE('',(#3136),#1985,.T.);
#22876=ADVANCED_FACE('',(#3137),#21963,.T.);
#22877=ADVANCED_FACE('',(#3138),#21964,.F.);
#22878=ADVANCED_FACE('',(#3139),#1986,.F.);
#22879=ADVANCED_FACE('',(#3140),#1987,.F.);
#22880=ADVANCED_FACE('',(#3141),#1988,.F.);
#22881=ADVANCED_FACE('',(#3142),#1989,.F.);
#22882=ADVANCED_FACE('',(#3143),#1990,.F.);
#22883=ADVANCED_FACE('',(#3144),#1991,.F.);
#22884=ADVANCED_FACE('',(#3145,#1439),#1992,.F.);
#22885=ADVANCED_FACE('',(#3146),#1993,.T.);
#22886=ADVANCED_FACE('',(#3147),#21965,.T.);
#22887=ADVANCED_FACE('',(#3148),#1116,.T.);
#22888=ADVANCED_FACE('',(#3149),#21966,.T.);
#22889=ADVANCED_FACE('',(#3150,#1440),#1994,.T.);
#22890=ADVANCED_FACE('',(#3151,#1441),#1995,.T.);
#22891=ADVANCED_FACE('',(#3152),#1117,.T.);
#22892=ADVANCED_FACE('',(#3153),#1118,.T.);
#22893=ADVANCED_FACE('',(#3154),#1119,.T.);
#22894=ADVANCED_FACE('',(#3155),#1120,.T.);
#22895=ADVANCED_FACE('',(#3156),#1121,.T.);
#22896=ADVANCED_FACE('',(#3157),#1122,.T.);
#22897=ADVANCED_FACE('',(#3158),#1123,.T.);
#22898=ADVANCED_FACE('',(#3159),#1124,.T.);
#22899=ADVANCED_FACE('',(#3160),#1125,.T.);
#22900=ADVANCED_FACE('',(#3161),#1126,.T.);
#22901=ADVANCED_FACE('',(#3162),#1127,.T.);
#22902=ADVANCED_FACE('',(#3163),#1128,.T.);
#22903=ADVANCED_FACE('',(#3164),#1129,.T.);
#22904=ADVANCED_FACE('',(#3165),#1130,.T.);
#22905=ADVANCED_FACE('',(#3166),#1131,.T.);
#22906=ADVANCED_FACE('',(#3167),#1132,.T.);
#22907=ADVANCED_FACE('',(#3168),#1133,.T.);
#22908=ADVANCED_FACE('',(#3169),#1134,.T.);
#22909=ADVANCED_FACE('',(#3170),#1135,.T.);
#22910=ADVANCED_FACE('',(#3171),#1136,.T.);
#22911=ADVANCED_FACE('',(#3172),#1137,.T.);
#22912=ADVANCED_FACE('',(#3173),#1138,.T.);
#22913=ADVANCED_FACE('',(#3174),#1139,.T.);
#22914=ADVANCED_FACE('',(#3175),#1140,.T.);
#22915=ADVANCED_FACE('',(#3176),#1141,.T.);
#22916=ADVANCED_FACE('',(#3177),#1142,.T.);
#22917=ADVANCED_FACE('',(#3178),#1143,.T.);
#22918=ADVANCED_FACE('',(#3179),#1144,.T.);
#22919=ADVANCED_FACE('',(#3180),#1145,.T.);
#22920=ADVANCED_FACE('',(#3181),#1146,.T.);
#22921=ADVANCED_FACE('',(#3182),#1147,.T.);
#22922=ADVANCED_FACE('',(#3183),#1148,.T.);
#22923=ADVANCED_FACE('',(#3184),#1149,.T.);
#22924=ADVANCED_FACE('',(#3185),#1150,.T.);
#22925=ADVANCED_FACE('',(#3186),#1151,.T.);
#22926=ADVANCED_FACE('',(#3187),#1152,.T.);
#22927=ADVANCED_FACE('',(#3188),#1153,.T.);
#22928=ADVANCED_FACE('',(#3189),#1154,.T.);
#22929=ADVANCED_FACE('',(#3190),#1155,.T.);
#22930=ADVANCED_FACE('',(#3191),#1156,.T.);
#22931=ADVANCED_FACE('',(#3192),#1157,.T.);
#22932=ADVANCED_FACE('',(#3193),#1158,.T.);
#22933=ADVANCED_FACE('',(#3194),#1159,.T.);
#22934=ADVANCED_FACE('',(#3195),#1160,.T.);
#22935=ADVANCED_FACE('',(#3196),#1161,.T.);
#22936=ADVANCED_FACE('',(#3197),#1162,.T.);
#22937=ADVANCED_FACE('',(#3198),#1163,.T.);
#22938=ADVANCED_FACE('',(#3199),#1164,.T.);
#22939=ADVANCED_FACE('',(#3200),#1165,.T.);
#22940=ADVANCED_FACE('',(#3201),#1166,.T.);
#22941=ADVANCED_FACE('',(#3202),#1167,.T.);
#22942=ADVANCED_FACE('',(#3203),#1168,.T.);
#22943=ADVANCED_FACE('',(#3204),#1169,.T.);
#22944=ADVANCED_FACE('',(#3205),#1170,.T.);
#22945=ADVANCED_FACE('',(#3206),#1171,.T.);
#22946=ADVANCED_FACE('',(#3207),#1172,.T.);
#22947=ADVANCED_FACE('',(#3208),#1173,.T.);
#22948=ADVANCED_FACE('',(#3209),#1174,.T.);
#22949=ADVANCED_FACE('',(#3210),#1175,.T.);
#22950=ADVANCED_FACE('',(#3211),#1176,.T.);
#22951=ADVANCED_FACE('',(#3212),#1177,.T.);
#22952=ADVANCED_FACE('',(#3213),#1178,.T.);
#22953=ADVANCED_FACE('',(#3214),#1179,.T.);
#22954=ADVANCED_FACE('',(#3215),#1180,.T.);
#22955=ADVANCED_FACE('',(#3216),#1181,.T.);
#22956=ADVANCED_FACE('',(#3217),#1182,.T.);
#22957=ADVANCED_FACE('',(#3218),#1183,.T.);
#22958=ADVANCED_FACE('',(#3219),#1184,.T.);
#22959=ADVANCED_FACE('',(#3220),#1185,.T.);
#22960=ADVANCED_FACE('',(#3221),#1186,.T.);
#22961=ADVANCED_FACE('',(#3222),#1187,.T.);
#22962=ADVANCED_FACE('',(#3223),#1188,.T.);
#22963=ADVANCED_FACE('',(#3224),#1189,.T.);
#22964=ADVANCED_FACE('',(#3225),#1190,.T.);
#22965=ADVANCED_FACE('',(#3226),#1191,.T.);
#22966=ADVANCED_FACE('',(#3227),#1192,.T.);
#22967=ADVANCED_FACE('',(#3228),#1193,.T.);
#22968=ADVANCED_FACE('',(#3229),#1194,.T.);
#22969=ADVANCED_FACE('',(#3230),#1195,.T.);
#22970=ADVANCED_FACE('',(#3231),#1196,.T.);
#22971=ADVANCED_FACE('',(#3232),#1197,.T.);
#22972=ADVANCED_FACE('',(#3233),#1198,.T.);
#22973=ADVANCED_FACE('',(#3234),#1199,.T.);
#22974=ADVANCED_FACE('',(#3235),#1200,.T.);
#22975=ADVANCED_FACE('',(#3236),#1201,.T.);
#22976=ADVANCED_FACE('',(#3237),#1202,.T.);
#22977=ADVANCED_FACE('',(#3238),#1203,.T.);
#22978=ADVANCED_FACE('',(#3239),#1204,.T.);
#22979=ADVANCED_FACE('',(#3240),#1205,.T.);
#22980=ADVANCED_FACE('',(#3241),#1206,.T.);
#22981=ADVANCED_FACE('',(#3242),#1207,.T.);
#22982=ADVANCED_FACE('',(#3243),#1208,.T.);
#22983=ADVANCED_FACE('',(#3244),#1209,.T.);
#22984=ADVANCED_FACE('',(#3245),#1210,.T.);
#22985=ADVANCED_FACE('',(#3246),#1211,.T.);
#22986=ADVANCED_FACE('',(#3247),#1212,.T.);
#22987=ADVANCED_FACE('',(#3248),#1213,.T.);
#22988=ADVANCED_FACE('',(#3249),#1214,.T.);
#22989=ADVANCED_FACE('',(#3250),#1215,.T.);
#22990=ADVANCED_FACE('',(#3251),#1216,.T.);
#22991=ADVANCED_FACE('',(#3252),#1217,.T.);
#22992=ADVANCED_FACE('',(#3253),#1218,.T.);
#22993=ADVANCED_FACE('',(#3254),#1219,.T.);
#22994=ADVANCED_FACE('',(#3255),#1220,.T.);
#22995=ADVANCED_FACE('',(#3256),#1221,.T.);
#22996=ADVANCED_FACE('',(#3257),#1222,.T.);
#22997=ADVANCED_FACE('',(#3258),#1223,.T.);
#22998=ADVANCED_FACE('',(#3259),#1224,.T.);
#22999=ADVANCED_FACE('',(#3260),#1225,.T.);
#23000=ADVANCED_FACE('',(#3261),#1226,.T.);
#23001=ADVANCED_FACE('',(#3262),#1227,.T.);
#23002=ADVANCED_FACE('',(#3263),#1228,.T.);
#23003=ADVANCED_FACE('',(#3264),#1229,.T.);
#23004=ADVANCED_FACE('',(#3265),#1230,.T.);
#23005=ADVANCED_FACE('',(#3266),#1231,.T.);
#23006=ADVANCED_FACE('',(#3267),#1232,.T.);
#23007=ADVANCED_FACE('',(#3268),#1233,.T.);
#23008=ADVANCED_FACE('',(#3269),#1996,.F.);
#23009=ADVANCED_FACE('',(#3270),#369,.F.);
#23010=ADVANCED_FACE('',(#3271),#1997,.T.);
#23011=ADVANCED_FACE('',(#3272),#1234,.T.);
#23012=ADVANCED_FACE('',(#3273),#370,.F.);
#23013=ADVANCED_FACE('',(#3274),#1998,.T.);
#23014=ADVANCED_FACE('',(#3275),#1999,.F.);
#23015=ADVANCED_FACE('',(#3276),#2000,.F.);
#23016=ADVANCED_FACE('',(#3277),#2001,.T.);
#23017=ADVANCED_FACE('',(#3278),#2002,.F.);
#23018=ADVANCED_FACE('',(#3279),#2003,.F.);
#23019=ADVANCED_FACE('',(#3280),#2004,.T.);
#23020=ADVANCED_FACE('',(#3281),#2005,.F.);
#23021=ADVANCED_FACE('',(#3282),#2006,.F.);
#23022=ADVANCED_FACE('',(#3283),#2007,.T.);
#23023=ADVANCED_FACE('',(#3284),#2008,.F.);
#23024=ADVANCED_FACE('',(#3285),#2009,.F.);
#23025=ADVANCED_FACE('',(#3286),#2010,.T.);
#23026=ADVANCED_FACE('',(#3287),#2011,.F.);
#23027=ADVANCED_FACE('',(#3288),#2012,.F.);
#23028=ADVANCED_FACE('',(#3289),#2013,.T.);
#23029=ADVANCED_FACE('',(#3290),#2014,.F.);
#23030=ADVANCED_FACE('',(#3291),#2015,.F.);
#23031=ADVANCED_FACE('',(#3292),#2016,.T.);
#23032=ADVANCED_FACE('',(#3293),#2017,.F.);
#23033=ADVANCED_FACE('',(#3294),#2018,.F.);
#23034=ADVANCED_FACE('',(#3295),#2019,.T.);
#23035=ADVANCED_FACE('',(#3296),#2020,.F.);
#23036=ADVANCED_FACE('',(#3297),#2021,.F.);
#23037=ADVANCED_FACE('',(#3298),#2022,.T.);
#23038=ADVANCED_FACE('',(#3299),#2023,.F.);
#23039=ADVANCED_FACE('',(#3300),#2024,.F.);
#23040=ADVANCED_FACE('',(#3301),#2025,.T.);
#23041=ADVANCED_FACE('',(#3302),#2026,.F.);
#23042=ADVANCED_FACE('',(#3303),#2027,.F.);
#23043=ADVANCED_FACE('',(#3304),#2028,.T.);
#23044=ADVANCED_FACE('',(#3305),#2029,.F.);
#23045=ADVANCED_FACE('',(#3306),#2030,.F.);
#23046=ADVANCED_FACE('',(#3307),#2031,.T.);
#23047=ADVANCED_FACE('',(#3308),#2032,.F.);
#23048=ADVANCED_FACE('',(#3309),#2033,.F.);
#23049=ADVANCED_FACE('',(#3310),#2034,.T.);
#23050=ADVANCED_FACE('',(#3311),#2035,.F.);
#23051=ADVANCED_FACE('',(#3312),#2036,.F.);
#23052=ADVANCED_FACE('',(#3313),#2037,.T.);
#23053=ADVANCED_FACE('',(#3314),#2038,.F.);
#23054=ADVANCED_FACE('',(#3315),#2039,.F.);
#23055=ADVANCED_FACE('',(#3316),#2040,.T.);
#23056=ADVANCED_FACE('',(#3317),#2041,.F.);
#23057=ADVANCED_FACE('',(#3318),#2042,.F.);
#23058=ADVANCED_FACE('',(#3319),#2043,.T.);
#23059=ADVANCED_FACE('',(#3320),#2044,.F.);
#23060=ADVANCED_FACE('',(#3321),#2045,.F.);
#23061=ADVANCED_FACE('',(#3322),#2046,.T.);
#23062=ADVANCED_FACE('',(#3323),#2047,.F.);
#23063=ADVANCED_FACE('',(#3324),#2048,.F.);
#23064=ADVANCED_FACE('',(#3325),#2049,.T.);
#23065=ADVANCED_FACE('',(#3326),#2050,.F.);
#23066=ADVANCED_FACE('',(#3327),#2051,.F.);
#23067=ADVANCED_FACE('',(#3328),#2052,.T.);
#23068=ADVANCED_FACE('',(#3329),#2053,.F.);
#23069=ADVANCED_FACE('',(#3330),#2054,.F.);
#23070=ADVANCED_FACE('',(#3331),#2055,.T.);
#23071=ADVANCED_FACE('',(#3332),#2056,.F.);
#23072=ADVANCED_FACE('',(#3333),#2057,.F.);
#23073=ADVANCED_FACE('',(#3334),#2058,.T.);
#23074=ADVANCED_FACE('',(#3335),#2059,.F.);
#23075=ADVANCED_FACE('',(#3336),#2060,.F.);
#23076=ADVANCED_FACE('',(#3337),#2061,.T.);
#23077=ADVANCED_FACE('',(#3338),#2062,.F.);
#23078=ADVANCED_FACE('',(#3339),#2063,.F.);
#23079=ADVANCED_FACE('',(#3340),#2064,.T.);
#23080=ADVANCED_FACE('',(#3341),#2065,.F.);
#23081=ADVANCED_FACE('',(#3342),#2066,.F.);
#23082=ADVANCED_FACE('',(#3343),#2067,.T.);
#23083=ADVANCED_FACE('',(#3344),#2068,.F.);
#23084=ADVANCED_FACE('',(#3345),#2069,.F.);
#23085=ADVANCED_FACE('',(#3346),#2070,.T.);
#23086=ADVANCED_FACE('',(#3347),#2071,.F.);
#23087=ADVANCED_FACE('',(#3348),#2072,.F.);
#23088=ADVANCED_FACE('',(#3349),#2073,.T.);
#23089=ADVANCED_FACE('',(#3350),#2074,.F.);
#23090=ADVANCED_FACE('',(#3351),#2075,.F.);
#23091=ADVANCED_FACE('',(#3352),#2076,.T.);
#23092=ADVANCED_FACE('',(#3353),#2077,.F.);
#23093=ADVANCED_FACE('',(#3354),#2078,.F.);
#23094=ADVANCED_FACE('',(#3355),#2079,.T.);
#23095=ADVANCED_FACE('',(#3356),#2080,.F.);
#23096=ADVANCED_FACE('',(#3357),#2081,.F.);
#23097=ADVANCED_FACE('',(#3358),#2082,.T.);
#23098=ADVANCED_FACE('',(#3359),#2083,.F.);
#23099=ADVANCED_FACE('',(#3360),#2084,.F.);
#23100=ADVANCED_FACE('',(#3361),#2085,.T.);
#23101=ADVANCED_FACE('',(#3362),#2086,.F.);
#23102=ADVANCED_FACE('',(#3363),#2087,.F.);
#23103=ADVANCED_FACE('',(#3364),#2088,.T.);
#23104=ADVANCED_FACE('',(#3365),#2089,.F.);
#23105=ADVANCED_FACE('',(#3366),#2090,.F.);
#23106=ADVANCED_FACE('',(#3367),#2091,.T.);
#23107=ADVANCED_FACE('',(#3368),#2092,.F.);
#23108=ADVANCED_FACE('',(#3369),#2093,.F.);
#23109=ADVANCED_FACE('',(#3370),#2094,.T.);
#23110=ADVANCED_FACE('',(#3371),#2095,.F.);
#23111=ADVANCED_FACE('',(#3372),#2096,.F.);
#23112=ADVANCED_FACE('',(#3373),#2097,.T.);
#23113=ADVANCED_FACE('',(#3374),#2098,.F.);
#23114=ADVANCED_FACE('',(#3375),#2099,.F.);
#23115=ADVANCED_FACE('',(#3376),#2100,.T.);
#23116=ADVANCED_FACE('',(#3377),#2101,.F.);
#23117=ADVANCED_FACE('',(#3378),#2102,.F.);
#23118=ADVANCED_FACE('',(#3379),#1235,.T.);
#23119=ADVANCED_FACE('',(#3380),#2103,.F.);
#23120=ADVANCED_FACE('',(#3381),#2104,.F.);
#23121=ADVANCED_FACE('',(#3382),#2105,.T.);
#23122=ADVANCED_FACE('',(#3383),#21967,.T.);
#23123=ADVANCED_FACE('',(#3384),#21968,.F.);
#23124=ADVANCED_FACE('',(#3385),#2106,.F.);
#23125=ADVANCED_FACE('',(#3386),#2107,.F.);
#23126=ADVANCED_FACE('',(#3387),#2108,.F.);
#23127=ADVANCED_FACE('',(#3388),#2109,.F.);
#23128=ADVANCED_FACE('',(#3389),#2110,.F.);
#23129=ADVANCED_FACE('',(#3390),#2111,.F.);
#23130=ADVANCED_FACE('',(#3391,#1442),#2112,.F.);
#23131=ADVANCED_FACE('',(#3392),#2113,.T.);
#23132=ADVANCED_FACE('',(#3393),#21969,.T.);
#23133=ADVANCED_FACE('',(#3394),#1236,.T.);
#23134=ADVANCED_FACE('',(#3395),#21970,.T.);
#23135=ADVANCED_FACE('',(#3396,#1443),#2114,.T.);
#23136=ADVANCED_FACE('',(#3397,#1444),#2115,.T.);
#23137=ADVANCED_FACE('',(#3398),#1237,.T.);
#23138=ADVANCED_FACE('',(#3399),#1238,.T.);
#23139=ADVANCED_FACE('',(#3400),#1239,.T.);
#23140=ADVANCED_FACE('',(#3401),#1240,.T.);
#23141=ADVANCED_FACE('',(#3402),#1241,.T.);
#23142=ADVANCED_FACE('',(#3403),#1242,.T.);
#23143=ADVANCED_FACE('',(#3404),#1243,.T.);
#23144=ADVANCED_FACE('',(#3405),#1244,.T.);
#23145=ADVANCED_FACE('',(#3406),#1245,.T.);
#23146=ADVANCED_FACE('',(#3407),#1246,.T.);
#23147=ADVANCED_FACE('',(#3408),#1247,.T.);
#23148=ADVANCED_FACE('',(#3409),#1248,.T.);
#23149=ADVANCED_FACE('',(#3410),#1249,.T.);
#23150=ADVANCED_FACE('',(#3411),#1250,.T.);
#23151=ADVANCED_FACE('',(#3412),#1251,.T.);
#23152=ADVANCED_FACE('',(#3413),#1252,.T.);
#23153=ADVANCED_FACE('',(#3414),#1253,.T.);
#23154=ADVANCED_FACE('',(#3415),#1254,.T.);
#23155=ADVANCED_FACE('',(#3416),#1255,.T.);
#23156=ADVANCED_FACE('',(#3417),#1256,.T.);
#23157=ADVANCED_FACE('',(#3418),#1257,.T.);
#23158=ADVANCED_FACE('',(#3419),#1258,.T.);
#23159=ADVANCED_FACE('',(#3420),#1259,.T.);
#23160=ADVANCED_FACE('',(#3421),#1260,.T.);
#23161=ADVANCED_FACE('',(#3422),#1261,.T.);
#23162=ADVANCED_FACE('',(#3423),#1262,.T.);
#23163=ADVANCED_FACE('',(#3424),#1263,.T.);
#23164=ADVANCED_FACE('',(#3425),#1264,.T.);
#23165=ADVANCED_FACE('',(#3426),#1265,.T.);
#23166=ADVANCED_FACE('',(#3427),#1266,.T.);
#23167=ADVANCED_FACE('',(#3428),#1267,.T.);
#23168=ADVANCED_FACE('',(#3429),#1268,.T.);
#23169=ADVANCED_FACE('',(#3430),#1269,.T.);
#23170=ADVANCED_FACE('',(#3431),#1270,.T.);
#23171=ADVANCED_FACE('',(#3432),#1271,.T.);
#23172=ADVANCED_FACE('',(#3433),#1272,.T.);
#23173=ADVANCED_FACE('',(#3434),#1273,.T.);
#23174=ADVANCED_FACE('',(#3435),#2116,.F.);
#23175=ADVANCED_FACE('',(#3436),#371,.F.);
#23176=ADVANCED_FACE('',(#3437),#2117,.T.);
#23177=ADVANCED_FACE('',(#3438),#1274,.T.);
#23178=ADVANCED_FACE('',(#3439),#372,.F.);
#23179=ADVANCED_FACE('',(#3440),#2118,.T.);
#23180=ADVANCED_FACE('',(#3441),#2119,.F.);
#23181=ADVANCED_FACE('',(#3442),#2120,.F.);
#23182=ADVANCED_FACE('',(#3443),#2121,.T.);
#23183=ADVANCED_FACE('',(#3444),#2122,.F.);
#23184=ADVANCED_FACE('',(#3445),#2123,.F.);
#23185=ADVANCED_FACE('',(#3446),#2124,.T.);
#23186=ADVANCED_FACE('',(#3447),#2125,.F.);
#23187=ADVANCED_FACE('',(#3448),#2126,.F.);
#23188=ADVANCED_FACE('',(#3449),#2127,.T.);
#23189=ADVANCED_FACE('',(#3450),#2128,.F.);
#23190=ADVANCED_FACE('',(#3451),#2129,.F.);
#23191=ADVANCED_FACE('',(#3452),#2130,.T.);
#23192=ADVANCED_FACE('',(#3453),#2131,.F.);
#23193=ADVANCED_FACE('',(#3454),#2132,.F.);
#23194=ADVANCED_FACE('',(#3455),#2133,.T.);
#23195=ADVANCED_FACE('',(#3456),#2134,.F.);
#23196=ADVANCED_FACE('',(#3457),#2135,.F.);
#23197=ADVANCED_FACE('',(#3458),#2136,.T.);
#23198=ADVANCED_FACE('',(#3459),#2137,.F.);
#23199=ADVANCED_FACE('',(#3460),#2138,.F.);
#23200=ADVANCED_FACE('',(#3461),#2139,.T.);
#23201=ADVANCED_FACE('',(#3462),#2140,.F.);
#23202=ADVANCED_FACE('',(#3463),#2141,.F.);
#23203=ADVANCED_FACE('',(#3464),#2142,.T.);
#23204=ADVANCED_FACE('',(#3465),#2143,.F.);
#23205=ADVANCED_FACE('',(#3466),#2144,.F.);
#23206=ADVANCED_FACE('',(#3467),#2145,.T.);
#23207=ADVANCED_FACE('',(#3468),#2146,.F.);
#23208=ADVANCED_FACE('',(#3469),#2147,.F.);
#23209=ADVANCED_FACE('',(#3470),#2148,.T.);
#23210=ADVANCED_FACE('',(#3471),#2149,.F.);
#23211=ADVANCED_FACE('',(#3472),#2150,.F.);
#23212=ADVANCED_FACE('',(#3473),#2151,.T.);
#23213=ADVANCED_FACE('',(#3474),#2152,.F.);
#23214=ADVANCED_FACE('',(#3475),#2153,.F.);
#23215=ADVANCED_FACE('',(#3476),#2154,.T.);
#23216=ADVANCED_FACE('',(#3477),#2155,.F.);
#23217=ADVANCED_FACE('',(#3478),#2156,.F.);
#23218=ADVANCED_FACE('',(#3479),#2157,.T.);
#23219=ADVANCED_FACE('',(#3480),#2158,.F.);
#23220=ADVANCED_FACE('',(#3481),#2159,.F.);
#23221=ADVANCED_FACE('',(#3482),#2160,.T.);
#23222=ADVANCED_FACE('',(#3483),#2161,.F.);
#23223=ADVANCED_FACE('',(#3484),#2162,.F.);
#23224=ADVANCED_FACE('',(#3485),#2163,.T.);
#23225=ADVANCED_FACE('',(#3486),#2164,.F.);
#23226=ADVANCED_FACE('',(#3487),#2165,.F.);
#23227=ADVANCED_FACE('',(#3488),#2166,.T.);
#23228=ADVANCED_FACE('',(#3489),#2167,.F.);
#23229=ADVANCED_FACE('',(#3490),#2168,.F.);
#23230=ADVANCED_FACE('',(#3491),#2169,.T.);
#23231=ADVANCED_FACE('',(#3492),#2170,.F.);
#23232=ADVANCED_FACE('',(#3493),#2171,.F.);
#23233=ADVANCED_FACE('',(#3494),#2172,.T.);
#23234=ADVANCED_FACE('',(#3495),#2173,.F.);
#23235=ADVANCED_FACE('',(#3496),#2174,.F.);
#23236=ADVANCED_FACE('',(#3497),#2175,.T.);
#23237=ADVANCED_FACE('',(#3498),#2176,.F.);
#23238=ADVANCED_FACE('',(#3499),#2177,.F.);
#23239=ADVANCED_FACE('',(#3500),#2178,.T.);
#23240=ADVANCED_FACE('',(#3501),#2179,.F.);
#23241=ADVANCED_FACE('',(#3502),#2180,.F.);
#23242=ADVANCED_FACE('',(#3503),#2181,.T.);
#23243=ADVANCED_FACE('',(#3504),#2182,.F.);
#23244=ADVANCED_FACE('',(#3505),#2183,.F.);
#23245=ADVANCED_FACE('',(#3506),#2184,.T.);
#23246=ADVANCED_FACE('',(#3507),#2185,.F.);
#23247=ADVANCED_FACE('',(#3508),#2186,.F.);
#23248=ADVANCED_FACE('',(#3509),#2187,.T.);
#23249=ADVANCED_FACE('',(#3510),#2188,.F.);
#23250=ADVANCED_FACE('',(#3511),#2189,.F.);
#23251=ADVANCED_FACE('',(#3512),#2190,.T.);
#23252=ADVANCED_FACE('',(#3513),#2191,.F.);
#23253=ADVANCED_FACE('',(#3514),#2192,.F.);
#23254=ADVANCED_FACE('',(#3515),#2193,.T.);
#23255=ADVANCED_FACE('',(#3516),#2194,.F.);
#23256=ADVANCED_FACE('',(#3517),#2195,.F.);
#23257=ADVANCED_FACE('',(#3518),#2196,.T.);
#23258=ADVANCED_FACE('',(#3519),#2197,.F.);
#23259=ADVANCED_FACE('',(#3520),#2198,.F.);
#23260=ADVANCED_FACE('',(#3521),#2199,.T.);
#23261=ADVANCED_FACE('',(#3522),#2200,.F.);
#23262=ADVANCED_FACE('',(#3523),#2201,.F.);
#23263=ADVANCED_FACE('',(#3524),#2202,.T.);
#23264=ADVANCED_FACE('',(#3525),#2203,.F.);
#23265=ADVANCED_FACE('',(#3526),#2204,.F.);
#23266=ADVANCED_FACE('',(#3527),#2205,.T.);
#23267=ADVANCED_FACE('',(#3528),#2206,.F.);
#23268=ADVANCED_FACE('',(#3529),#2207,.F.);
#23269=ADVANCED_FACE('',(#3530),#2208,.T.);
#23270=ADVANCED_FACE('',(#3531),#2209,.F.);
#23271=ADVANCED_FACE('',(#3532),#2210,.F.);
#23272=ADVANCED_FACE('',(#3533),#2211,.T.);
#23273=ADVANCED_FACE('',(#3534),#2212,.F.);
#23274=ADVANCED_FACE('',(#3535),#2213,.F.);
#23275=ADVANCED_FACE('',(#3536),#2214,.T.);
#23276=ADVANCED_FACE('',(#3537),#2215,.F.);
#23277=ADVANCED_FACE('',(#3538),#2216,.F.);
#23278=ADVANCED_FACE('',(#3539),#2217,.T.);
#23279=ADVANCED_FACE('',(#3540),#2218,.F.);
#23280=ADVANCED_FACE('',(#3541),#2219,.F.);
#23281=ADVANCED_FACE('',(#3542),#2220,.T.);
#23282=ADVANCED_FACE('',(#3543),#2221,.F.);
#23283=ADVANCED_FACE('',(#3544),#2222,.F.);
#23284=ADVANCED_FACE('',(#3545),#1275,.T.);
#23285=ADVANCED_FACE('',(#3546),#2223,.F.);
#23286=ADVANCED_FACE('',(#3547),#2224,.F.);
#23287=ADVANCED_FACE('',(#3548),#2225,.T.);
#23288=ADVANCED_FACE('',(#3549),#21971,.T.);
#23289=ADVANCED_FACE('',(#3550),#21972,.F.);
#23290=ADVANCED_FACE('',(#3551),#2226,.F.);
#23291=ADVANCED_FACE('',(#3552),#2227,.F.);
#23292=ADVANCED_FACE('',(#3553),#2228,.F.);
#23293=ADVANCED_FACE('',(#3554),#2229,.F.);
#23294=ADVANCED_FACE('',(#3555),#2230,.F.);
#23295=ADVANCED_FACE('',(#3556),#2231,.F.);
#23296=ADVANCED_FACE('',(#3557,#1445),#2232,.F.);
#23297=ADVANCED_FACE('',(#3558),#2233,.T.);
#23298=ADVANCED_FACE('',(#3559),#21973,.T.);
#23299=ADVANCED_FACE('',(#3560),#1276,.T.);
#23300=ADVANCED_FACE('',(#3561),#21974,.T.);
#23301=ADVANCED_FACE('',(#3562,#1446),#2234,.T.);
#23302=ADVANCED_FACE('',(#3563,#1447),#2235,.T.);
#23303=CLOSED_SHELL('',(#21975,#21976,#21977,#21978,#21979,#21980,#21981,
#21982,#21983,#21984,#21985,#21986,#21987,#21988,#21989,#21990,#21991,#21992,
#21993,#21994,#21995,#21996,#21997,#21998,#21999,#22000,#22001,#22002,#22003,
#22004,#22005,#22006,#22007,#22008,#22009,#22010,#22011,#22012,#22013,#22014,
#22015,#22016,#22017,#22018,#22019,#22020,#22021,#22022,#22023,#22024,#22025,
#22026,#22027,#22028,#22029,#22030,#22031,#22032,#22033,#22034,#22035,#22036,
#22037,#22038,#22039,#22040,#22041,#22042,#22043,#22044,#22045,#22046,#22047,
#22048,#22049,#22050,#22051,#22052,#22053,#22054,#22055,#22056,#22057,#22058,
#22059,#22060,#22061,#22062,#22063,#22064,#22065,#22066,#22067,#22068,#22069,
#22070,#22071,#22072,#22073,#22074));
#23304=CLOSED_SHELL('',(#22075,#22076,#22077,#22078,#22079,#22080,#22081,
#22082,#22083,#22084,#22085,#22086,#22087,#22088,#22089,#22090,#22091,#22092,
#22093,#22094,#22095,#22096,#22097,#22098,#22099,#22100,#22101,#22102,#22103,
#22104,#22105,#22106,#22107,#22108,#22109,#22110,#22111,#22112,#22113,#22114,
#22115,#22116,#22117,#22118,#22119,#22120,#22121,#22122,#22123,#22124,#22125,
#22126,#22127,#22128,#22129,#22130,#22131,#22132,#22133,#22134,#22135,#22136,
#22137,#22138,#22139,#22140,#22141,#22142,#22143,#22144,#22145,#22146,#22147,
#22148,#22149,#22150,#22151,#22152,#22153,#22154,#22155,#22156,#22157,#22158,
#22159,#22160,#22161,#22162,#22163,#22164,#22165,#22166,#22167));
#23305=CLOSED_SHELL('',(#22168,#22169,#22170,#22171,#22172,#22173,#22174,
#22175,#22176,#22177,#22178,#22179,#22180,#22181,#22182,#22183,#22184,#22185,
#22186,#22187,#22188,#22189,#22190,#22191,#22192,#22193,#22194,#22195,#22196,
#22197,#22198,#22199,#22200,#22201,#22202,#22203,#22204,#22205,#22206,#22207,
#22208,#22209,#22210,#22211,#22212,#22213,#22214,#22215,#22216,#22217,#22218,
#22219,#22220,#22221,#22222,#22223,#22224,#22225,#22226,#22227,#22228,#22229,
#22230,#22231,#22232,#22233,#22234,#22235,#22236,#22237,#22238,#22239,#22240,
#22241,#22242));
#23306=CLOSED_SHELL('',(#22243,#22244,#22245,#22246,#22247,#22248,#22249,
#22250,#22251,#22252,#22253,#22254,#22255,#22256,#22257,#22258,#22259,#22260,
#22261,#22262,#22263,#22264,#22265,#22266,#22267));
#23307=CLOSED_SHELL('',(#22268,#22269,#22270,#22271,#22272,#22273,#22274,
#22275,#22276,#22277,#22278,#22279,#22280,#22281,#22282,#22283,#22284,#22285,
#22286,#22287,#22288,#22289,#22290,#22291,#22292,#22293));
#23308=CLOSED_SHELL('',(#22294,#22295,#22296,#22297,#22298,#22299,#22300,
#22301,#22302,#22303,#22304,#22305,#22306,#22307,#22308,#22309,#22310,#22311,
#22312,#22313,#22314,#22315,#22316,#22317,#22318,#22319,#22320,#22321,#22322,
#22323,#22324,#22325,#22326,#22327,#22328,#22329,#22330,#22331,#22332,#22333,
#22334,#22335,#22336,#22337,#22338,#22339,#22340,#22341,#22342,#22343,#22344,
#22345,#22346,#22347,#22348,#22349,#22350,#22351,#22352,#22353,#22354,#22355,
#22356,#22357,#22358,#22359,#22360,#22361,#22362,#22363,#22364,#22365,#22366,
#22367,#22368,#22369,#22370,#22371,#22372,#22373,#22374,#22375,#22376,#22377,
#22378,#22379,#22380,#22381,#22382,#22383,#22384,#22385,#22386,#22387,#22388,
#22389,#22390,#22391,#22392,#22393,#22394,#22395,#22396,#22397,#22398,#22399,
#22400,#22401,#22402,#22403,#22404,#22405,#22406,#22407,#22408,#22409,#22410,
#22411,#22412,#22413,#22414,#22415,#22416,#22417,#22418,#22419,#22420,#22421,
#22422,#22423,#22424,#22425,#22426,#22427,#22428,#22429,#22430,#22431,#22432,
#22433,#22434,#22435,#22436,#22437,#22438,#22439,#22440,#22441,#22442,#22443,
#22444));
#23309=CLOSED_SHELL('',(#22445,#22446,#22447,#22448,#22449));
#23310=CLOSED_SHELL('',(#22450,#22451,#22452,#22453,#22454,#22455,#22456,
#22457,#22458,#22459,#22460,#22461,#22462,#22463));
#23311=CLOSED_SHELL('',(#22464,#22465,#22466,#22467,#22468,#22469,#22470,
#22471,#22472,#22473,#22474,#22475,#22476,#22477,#22478,#22479,#22480,#22481,
#22482,#22483,#22484,#22485,#22486,#22487,#22488,#22489,#22490,#22491,#22492,
#22493,#22494,#22495,#22496,#22497,#22498,#22499,#22500,#22501,#22502,#22503,
#22504,#22505,#22506,#22507,#22508,#22509,#22510,#22511,#22512,#22513,#22514,
#22515,#22516,#22517,#22518,#22519,#22520,#22521,#22522,#22523,#22524,#22525,
#22526,#22527,#22528,#22529,#22530,#22531,#22532,#22533,#22534,#22535,#22536,
#22537,#22538,#22539,#22540,#22541,#22542,#22543,#22544,#22545,#22546,#22547,
#22548,#22549,#22550,#22551,#22552));
#23312=CLOSED_SHELL('',(#22553,#22554,#22555,#22556));
#23313=CLOSED_SHELL('',(#22557,#22558,#22559,#22560,#22561,#22562,#22563,
#22564,#22565,#22566,#22567,#22568,#22569,#22570,#22571,#22572,#22573,#22574,
#22575,#22576,#22577,#22578,#22579,#22580,#22581,#22582,#22583,#22584,#22585,
#22586,#22587,#22588,#22589,#22590));
#23314=CLOSED_SHELL('',(#22591,#22592,#22593,#22594));
#23315=CLOSED_SHELL('',(#22595,#22596,#22597,#22598,#22599,#22600,#22601,
#22602,#22603,#22604,#22605,#22606,#22607,#22608,#22609,#22610,#22611,#22612,
#22613,#22614,#22615,#22616,#22617,#22618,#22619,#22620,#22621,#22622,#22623,
#22624,#22625,#22626,#22627,#22628,#22629,#22630,#22631,#22632,#22633,#22634,
#22635,#22636,#22637,#22638,#22639,#22640,#22641,#22642,#22643,#22644,#22645,
#22646,#22647,#22648,#22649,#22650,#22651,#22652,#22653,#22654,#22655,#22656,
#22657,#22658,#22659,#22660,#22661,#22662,#22663,#22664,#22665,#22666,#22667,
#22668,#22669,#22670,#22671,#22672,#22673,#22674,#22675,#22676,#22677,#22678,
#22679,#22680,#22681,#22682,#22683,#22684,#22685,#22686,#22687,#22688,#22689,
#22690,#22691,#22692,#22693,#22694,#22695,#22696,#22697,#22698,#22699,#22700,
#22701,#22702,#22703,#22704,#22705,#22706,#22707,#22708,#22709,#22710,#22711,
#22712,#22713,#22714,#22715,#22716,#22717,#22718,#22719,#22720,#22721,#22722,
#22723,#22724,#22725,#22726,#22727,#22728,#22729,#22730,#22731,#22732));
#23316=CLOSED_SHELL('',(#22733,#22734,#22735,#22736,#22737,#22738,#22739,
#22740,#22741,#22742,#22743,#22744,#22745,#22746,#22747,#22748,#22749,#22750,
#22751,#22752,#22753,#22754,#22755,#22756,#22757,#22758,#22759,#22760,#22761,
#22762,#22763,#22764,#22765,#22766,#22767,#22768,#22769,#22770,#22771,#22772,
#22773,#22774,#22775,#22776,#22777,#22778,#22779,#22780,#22781,#22782,#22783,
#22784,#22785,#22786,#22787,#22788,#22789,#22790,#22791,#22792,#22793,#22794,
#22795,#22796,#22797,#22798,#22799,#22800,#22801,#22802,#22803,#22804,#22805,
#22806,#22807,#22808,#22809,#22810,#22811,#22812,#22813,#22814,#22815,#22816,
#22817,#22818,#22819,#22820,#22821,#22822,#22823,#22824,#22825,#22826,#22827,
#22828,#22829,#22830,#22831,#22832,#22833,#22834,#22835,#22836,#22837,#22838,
#22839,#22840,#22841,#22842,#22843,#22844,#22845,#22846,#22847,#22848,#22849,
#22850,#22851,#22852,#22853,#22854,#22855,#22856,#22857,#22858,#22859,#22860,
#22861,#22862,#22863,#22864,#22865,#22866,#22867,#22868,#22869,#22870,#22871,
#22872,#22873,#22874,#22875,#22876,#22877,#22878,#22879,#22880,#22881,#22882,
#22883,#22884,#22885,#22886,#22887,#22888,#22889,#22890));
#23317=CLOSED_SHELL('',(#22891,#22892,#22893,#22894,#22895,#22896,#22897,
#22898,#22899,#22900,#22901,#22902,#22903,#22904,#22905,#22906,#22907,#22908,
#22909,#22910,#22911,#22912,#22913,#22914,#22915,#22916,#22917,#22918,#22919,
#22920,#22921,#22922,#22923,#22924,#22925,#22926,#22927,#22928,#22929,#22930,
#22931,#22932,#22933,#22934,#22935,#22936,#22937,#22938,#22939,#22940,#22941,
#22942,#22943,#22944,#22945,#22946,#22947,#22948,#22949,#22950,#22951,#22952,
#22953,#22954,#22955,#22956,#22957,#22958,#22959,#22960,#22961,#22962,#22963,
#22964,#22965,#22966,#22967,#22968,#22969,#22970,#22971,#22972,#22973,#22974,
#22975,#22976,#22977,#22978,#22979,#22980,#22981,#22982,#22983,#22984,#22985,
#22986,#22987,#22988,#22989,#22990,#22991,#22992,#22993,#22994,#22995,#22996,
#22997,#22998,#22999,#23000,#23001,#23002,#23003,#23004,#23005,#23006,#23007,
#23008,#23009,#23010,#23011,#23012,#23013,#23014,#23015,#23016,#23017,#23018,
#23019,#23020,#23021,#23022,#23023,#23024,#23025,#23026,#23027,#23028,#23029,
#23030,#23031,#23032,#23033,#23034,#23035,#23036,#23037,#23038,#23039,#23040,
#23041,#23042,#23043,#23044,#23045,#23046,#23047,#23048,#23049,#23050,#23051,
#23052,#23053,#23054,#23055,#23056,#23057,#23058,#23059,#23060,#23061,#23062,
#23063,#23064,#23065,#23066,#23067,#23068,#23069,#23070,#23071,#23072,#23073,
#23074,#23075,#23076,#23077,#23078,#23079,#23080,#23081,#23082,#23083,#23084,
#23085,#23086,#23087,#23088,#23089,#23090,#23091,#23092,#23093,#23094,#23095,
#23096,#23097,#23098,#23099,#23100,#23101,#23102,#23103,#23104,#23105,#23106,
#23107,#23108,#23109,#23110,#23111,#23112,#23113,#23114,#23115,#23116,#23117,
#23118,#23119,#23120,#23121,#23122,#23123,#23124,#23125,#23126,#23127,#23128,
#23129,#23130,#23131,#23132,#23133,#23134,#23135,#23136));
#23318=CLOSED_SHELL('',(#23137,#23138,#23139,#23140,#23141,#23142,#23143,
#23144,#23145,#23146,#23147,#23148,#23149,#23150,#23151,#23152,#23153,#23154,
#23155,#23156,#23157,#23158,#23159,#23160,#23161,#23162,#23163,#23164,#23165,
#23166,#23167,#23168,#23169,#23170,#23171,#23172,#23173,#23174,#23175,#23176,
#23177,#23178,#23179,#23180,#23181,#23182,#23183,#23184,#23185,#23186,#23187,
#23188,#23189,#23190,#23191,#23192,#23193,#23194,#23195,#23196,#23197,#23198,
#23199,#23200,#23201,#23202,#23203,#23204,#23205,#23206,#23207,#23208,#23209,
#23210,#23211,#23212,#23213,#23214,#23215,#23216,#23217,#23218,#23219,#23220,
#23221,#23222,#23223,#23224,#23225,#23226,#23227,#23228,#23229,#23230,#23231,
#23232,#23233,#23234,#23235,#23236,#23237,#23238,#23239,#23240,#23241,#23242,
#23243,#23244,#23245,#23246,#23247,#23248,#23249,#23250,#23251,#23252,#23253,
#23254,#23255,#23256,#23257,#23258,#23259,#23260,#23261,#23262,#23263,#23264,
#23265,#23266,#23267,#23268,#23269,#23270,#23271,#23272,#23273,#23274,#23275,
#23276,#23277,#23278,#23279,#23280,#23281,#23282,#23283,#23284,#23285,#23286,
#23287,#23288,#23289,#23290,#23291,#23292,#23293,#23294,#23295,#23296,#23297,
#23298,#23299,#23300,#23301,#23302));
#23319=DERIVED_UNIT_ELEMENT(#23351,1.);
#23320=DERIVED_UNIT_ELEMENT(#53652,-3.);
#23321=DERIVED_UNIT_ELEMENT(#23351,1.);
#23322=DERIVED_UNIT_ELEMENT(#53652,-3.);
#23323=DERIVED_UNIT_ELEMENT(#23351,1.);
#23324=DERIVED_UNIT_ELEMENT(#53652,-3.);
#23325=DERIVED_UNIT_ELEMENT(#23351,1.);
#23326=DERIVED_UNIT_ELEMENT(#53652,-3.);
#23327=DERIVED_UNIT_ELEMENT(#23351,1.);
#23328=DERIVED_UNIT_ELEMENT(#53652,-3.);
#23329=DERIVED_UNIT_ELEMENT(#23351,1.);
#23330=DERIVED_UNIT_ELEMENT(#53652,-3.);
#23331=DERIVED_UNIT_ELEMENT(#23351,1.);
#23332=DERIVED_UNIT_ELEMENT(#53652,-3.);
#23333=DERIVED_UNIT_ELEMENT(#23351,1.);
#23334=DERIVED_UNIT_ELEMENT(#53652,-3.);
#23335=DERIVED_UNIT_ELEMENT(#23351,1.);
#23336=DERIVED_UNIT_ELEMENT(#53652,-3.);
#23337=DERIVED_UNIT_ELEMENT(#23351,1.);
#23338=DERIVED_UNIT_ELEMENT(#53652,-3.);
#23339=DERIVED_UNIT_ELEMENT(#23351,1.);
#23340=DERIVED_UNIT_ELEMENT(#53652,-3.);
#23341=DERIVED_UNIT_ELEMENT(#23351,1.);
#23342=DERIVED_UNIT_ELEMENT(#53652,-3.);
#23343=DERIVED_UNIT_ELEMENT(#23351,1.);
#23344=DERIVED_UNIT_ELEMENT(#53652,-3.);
#23345=DERIVED_UNIT_ELEMENT(#23351,1.);
#23346=DERIVED_UNIT_ELEMENT(#53652,-3.);
#23347=DERIVED_UNIT_ELEMENT(#23351,1.);
#23348=DERIVED_UNIT_ELEMENT(#53652,-3.);
#23349=DERIVED_UNIT_ELEMENT(#23351,1.);
#23350=DERIVED_UNIT_ELEMENT(#53652,-3.);
#23351=(
MASS_UNIT()
NAMED_UNIT(*)
SI_UNIT(.KILO.,.GRAM.)
);
#23352=DERIVED_UNIT((#23319,#23320));
#23353=DERIVED_UNIT((#23321,#23322));
#23354=DERIVED_UNIT((#23323,#23324));
#23355=DERIVED_UNIT((#23325,#23326));
#23356=DERIVED_UNIT((#23327,#23328));
#23357=DERIVED_UNIT((#23329,#23330));
#23358=DERIVED_UNIT((#23331,#23332));
#23359=DERIVED_UNIT((#23333,#23334));
#23360=DERIVED_UNIT((#23335,#23336));
#23361=DERIVED_UNIT((#23337,#23338));
#23362=DERIVED_UNIT((#23339,#23340));
#23363=DERIVED_UNIT((#23341,#23342));
#23364=DERIVED_UNIT((#23343,#23344));
#23365=DERIVED_UNIT((#23345,#23346));
#23366=DERIVED_UNIT((#23347,#23348));
#23367=DERIVED_UNIT((#23349,#23350));
#23368=MEASURE_REPRESENTATION_ITEM('density measure',
POSITIVE_RATIO_MEASURE(2700.),#23352);
#23369=MEASURE_REPRESENTATION_ITEM('density measure',
POSITIVE_RATIO_MEASURE(2700.),#23353);
#23370=MEASURE_REPRESENTATION_ITEM('density measure',
POSITIVE_RATIO_MEASURE(2700.),#23354);
#23371=MEASURE_REPRESENTATION_ITEM('density measure',
POSITIVE_RATIO_MEASURE(7850.),#23355);
#23372=MEASURE_REPRESENTATION_ITEM('density measure',
POSITIVE_RATIO_MEASURE(2700.),#23356);
#23373=MEASURE_REPRESENTATION_ITEM('density measure',
POSITIVE_RATIO_MEASURE(8470.),#23357);
#23374=MEASURE_REPRESENTATION_ITEM('density measure',
POSITIVE_RATIO_MEASURE(2180.),#23358);
#23375=MEASURE_REPRESENTATION_ITEM('density measure',
POSITIVE_RATIO_MEASURE(3900.),#23359);
#23376=MEASURE_REPRESENTATION_ITEM('density measure',
POSITIVE_RATIO_MEASURE(8000.),#23360);
#23377=MEASURE_REPRESENTATION_ITEM('density measure',
POSITIVE_RATIO_MEASURE(1250.),#23361);
#23378=MEASURE_REPRESENTATION_ITEM('density measure',
POSITIVE_RATIO_MEASURE(8000.),#23362);
#23379=MEASURE_REPRESENTATION_ITEM('density measure',
POSITIVE_RATIO_MEASURE(7850.),#23363);
#23380=MEASURE_REPRESENTATION_ITEM('density measure',
POSITIVE_RATIO_MEASURE(2700.),#23364);
#23381=MEASURE_REPRESENTATION_ITEM('density measure',
POSITIVE_RATIO_MEASURE(8000.),#23365);
#23382=MEASURE_REPRESENTATION_ITEM('density measure',
POSITIVE_RATIO_MEASURE(8000.),#23366);
#23383=MEASURE_REPRESENTATION_ITEM('density measure',
POSITIVE_RATIO_MEASURE(8000.),#23367);
#23384=PROPERTY_DEFINITION_REPRESENTATION(#23464,#23416);
#23385=PROPERTY_DEFINITION_REPRESENTATION(#23465,#23417);
#23386=PROPERTY_DEFINITION_REPRESENTATION(#23466,#23418);
#23387=PROPERTY_DEFINITION_REPRESENTATION(#23467,#23419);
#23388=PROPERTY_DEFINITION_REPRESENTATION(#23468,#23420);
#23389=PROPERTY_DEFINITION_REPRESENTATION(#23469,#23421);
#23390=PROPERTY_DEFINITION_REPRESENTATION(#23470,#23422);
#23391=PROPERTY_DEFINITION_REPRESENTATION(#23471,#23423);
#23392=PROPERTY_DEFINITION_REPRESENTATION(#23472,#23424);
#23393=PROPERTY_DEFINITION_REPRESENTATION(#23473,#23425);
#23394=PROPERTY_DEFINITION_REPRESENTATION(#23474,#23426);
#23395=PROPERTY_DEFINITION_REPRESENTATION(#23475,#23427);
#23396=PROPERTY_DEFINITION_REPRESENTATION(#23476,#23428);
#23397=PROPERTY_DEFINITION_REPRESENTATION(#23477,#23429);
#23398=PROPERTY_DEFINITION_REPRESENTATION(#23478,#23430);
#23399=PROPERTY_DEFINITION_REPRESENTATION(#23479,#23431);
#23400=PROPERTY_DEFINITION_REPRESENTATION(#23480,#23432);
#23401=PROPERTY_DEFINITION_REPRESENTATION(#23481,#23433);
#23402=PROPERTY_DEFINITION_REPRESENTATION(#23482,#23434);
#23403=PROPERTY_DEFINITION_REPRESENTATION(#23483,#23435);
#23404=PROPERTY_DEFINITION_REPRESENTATION(#23484,#23436);
#23405=PROPERTY_DEFINITION_REPRESENTATION(#23485,#23437);
#23406=PROPERTY_DEFINITION_REPRESENTATION(#23486,#23438);
#23407=PROPERTY_DEFINITION_REPRESENTATION(#23487,#23439);
#23408=PROPERTY_DEFINITION_REPRESENTATION(#23488,#23440);
#23409=PROPERTY_DEFINITION_REPRESENTATION(#23489,#23441);
#23410=PROPERTY_DEFINITION_REPRESENTATION(#23490,#23442);
#23411=PROPERTY_DEFINITION_REPRESENTATION(#23491,#23443);
#23412=PROPERTY_DEFINITION_REPRESENTATION(#23492,#23444);
#23413=PROPERTY_DEFINITION_REPRESENTATION(#23493,#23445);
#23414=PROPERTY_DEFINITION_REPRESENTATION(#23494,#23446);
#23415=PROPERTY_DEFINITION_REPRESENTATION(#23495,#23447);
#23416=REPRESENTATION('material name',(#23448),#53634);
#23417=REPRESENTATION('density',(#23368),#53634);
#23418=REPRESENTATION('material name',(#23449),#53635);
#23419=REPRESENTATION('density',(#23369),#53635);
#23420=REPRESENTATION('material name',(#23450),#53636);
#23421=REPRESENTATION('density',(#23370),#53636);
#23422=REPRESENTATION('material name',(#23451),#53637);
#23423=REPRESENTATION('density',(#23371),#53637);
#23424=REPRESENTATION('material name',(#23452),#53638);
#23425=REPRESENTATION('density',(#23372),#53638);
#23426=REPRESENTATION('material name',(#23453),#53639);
#23427=REPRESENTATION('density',(#23373),#53639);
#23428=REPRESENTATION('material name',(#23454),#53640);
#23429=REPRESENTATION('density',(#23374),#53640);
#23430=REPRESENTATION('material name',(#23455),#53641);
#23431=REPRESENTATION('density',(#23375),#53641);
#23432=REPRESENTATION('material name',(#23456),#53642);
#23433=REPRESENTATION('density',(#23376),#53642);
#23434=REPRESENTATION('material name',(#23457),#53643);
#23435=REPRESENTATION('density',(#23377),#53643);
#23436=REPRESENTATION('material name',(#23458),#53644);
#23437=REPRESENTATION('density',(#23378),#53644);
#23438=REPRESENTATION('material name',(#23459),#53645);
#23439=REPRESENTATION('density',(#23379),#53645);
#23440=REPRESENTATION('material name',(#23460),#53646);
#23441=REPRESENTATION('density',(#23380),#53646);
#23442=REPRESENTATION('material name',(#23461),#53647);
#23443=REPRESENTATION('density',(#23381),#53647);
#23444=REPRESENTATION('material name',(#23462),#53648);
#23445=REPRESENTATION('density',(#23382),#53648);
#23446=REPRESENTATION('material name',(#23463),#53649);
#23447=REPRESENTATION('density',(#23383),#53649);
#23448=DESCRIPTIVE_REPRESENTATION_ITEM('Aluminum 6061','Aluminum 6061');
#23449=DESCRIPTIVE_REPRESENTATION_ITEM('Aluminum 6061','Aluminum 6061');
#23450=DESCRIPTIVE_REPRESENTATION_ITEM('Aluminum 6061','Aluminum 6061');
#23451=DESCRIPTIVE_REPRESENTATION_ITEM('Steel','Steel');
#23452=DESCRIPTIVE_REPRESENTATION_ITEM('Aluminum 6061','Aluminum 6061');
#23453=DESCRIPTIVE_REPRESENTATION_ITEM('Brass, Soft Yellow',
'Brass, Soft Yellow');
#23454=DESCRIPTIVE_REPRESENTATION_ITEM('Glass','Glass');
#23455=DESCRIPTIVE_REPRESENTATION_ITEM('Alumina (Al2O3)',
'Alumina (Al2O3)');
#23456=DESCRIPTIVE_REPRESENTATION_ITEM('Stainless Steel AISI 304',
'Stainless Steel AISI 304');
#23457=DESCRIPTIVE_REPRESENTATION_ITEM('Rubber, Silicone',
'Rubber, Silicone');
#23458=DESCRIPTIVE_REPRESENTATION_ITEM('Stainless Steel AISI 304',
'Stainless Steel AISI 304');
#23459=DESCRIPTIVE_REPRESENTATION_ITEM('Steel','Steel');
#23460=DESCRIPTIVE_REPRESENTATION_ITEM('Aluminum 6061','Aluminum 6061');
#23461=DESCRIPTIVE_REPRESENTATION_ITEM('Stainless Steel AISI 304',
'Stainless Steel AISI 304');
#23462=DESCRIPTIVE_REPRESENTATION_ITEM('Stainless Steel AISI 304',
'Stainless Steel AISI 304');
#23463=DESCRIPTIVE_REPRESENTATION_ITEM('Stainless Steel AISI 304',
'Stainless Steel AISI 304');
#23464=PROPERTY_DEFINITION('material property','material name',#53742);
#23465=PROPERTY_DEFINITION('material property','density of part',#53742);
#23466=PROPERTY_DEFINITION('material property','material name',#53743);
#23467=PROPERTY_DEFINITION('material property','density of part',#53743);
#23468=PROPERTY_DEFINITION('material property','material name',#53744);
#23469=PROPERTY_DEFINITION('material property','density of part',#53744);
#23470=PROPERTY_DEFINITION('material property','material name',#53745);
#23471=PROPERTY_DEFINITION('material property','density of part',#53745);
#23472=PROPERTY_DEFINITION('material property','material name',#53746);
#23473=PROPERTY_DEFINITION('material property','density of part',#53746);
#23474=PROPERTY_DEFINITION('material property','material name',#53747);
#23475=PROPERTY_DEFINITION('material property','density of part',#53747);
#23476=PROPERTY_DEFINITION('material property','material name',#53748);
#23477=PROPERTY_DEFINITION('material property','density of part',#53748);
#23478=PROPERTY_DEFINITION('material property','material name',#53749);
#23479=PROPERTY_DEFINITION('material property','density of part',#53749);
#23480=PROPERTY_DEFINITION('material property','material name',#53750);
#23481=PROPERTY_DEFINITION('material property','density of part',#53750);
#23482=PROPERTY_DEFINITION('material property','material name',#53751);
#23483=PROPERTY_DEFINITION('material property','density of part',#53751);
#23484=PROPERTY_DEFINITION('material property','material name',#53752);
#23485=PROPERTY_DEFINITION('material property','density of part',#53752);
#23486=PROPERTY_DEFINITION('material property','material name',#53753);
#23487=PROPERTY_DEFINITION('material property','density of part',#53753);
#23488=PROPERTY_DEFINITION('material property','material name',#53754);
#23489=PROPERTY_DEFINITION('material property','density of part',#53754);
#23490=PROPERTY_DEFINITION('material property','material name',#53755);
#23491=PROPERTY_DEFINITION('material property','density of part',#53755);
#23492=PROPERTY_DEFINITION('material property','material name',#53756);
#23493=PROPERTY_DEFINITION('material property','density of part',#53756);
#23494=PROPERTY_DEFINITION('material property','material name',#53757);
#23495=PROPERTY_DEFINITION('material property','density of part',#53757);
#23496=AXIS2_PLACEMENT_3D('',#31815,#25654,#25655);
#23497=AXIS2_PLACEMENT_3D('',#31816,#25656,#25657);
#23498=AXIS2_PLACEMENT_3D('',#31817,#25658,#25659);
#23499=AXIS2_PLACEMENT_3D('',#31822,#25661,#25662);
#23500=AXIS2_PLACEMENT_3D('',#31825,#25664,#25665);
#23501=AXIS2_PLACEMENT_3D('',#31826,#25666,#25667);
#23502=AXIS2_PLACEMENT_3D('',#31832,#25671,#25672);
#23503=AXIS2_PLACEMENT_3D('',#31836,#25674,#25675);
#23504=AXIS2_PLACEMENT_3D('',#31837,#25676,#25677);
#23505=AXIS2_PLACEMENT_3D('',#31838,#25678,#25679);
#23506=AXIS2_PLACEMENT_3D('',#31844,#25683,#25684);
#23507=AXIS2_PLACEMENT_3D('',#31848,#25686,#25687);
#23508=AXIS2_PLACEMENT_3D('',#31849,#25688,#25689);
#23509=AXIS2_PLACEMENT_3D('',#31850,#25690,#25691);
#23510=AXIS2_PLACEMENT_3D('',#31856,#25695,#25696);
#23511=AXIS2_PLACEMENT_3D('',#31860,#25698,#25699);
#23512=AXIS2_PLACEMENT_3D('',#31861,#25700,#25701);
#23513=AXIS2_PLACEMENT_3D('',#31862,#25702,#25703);
#23514=AXIS2_PLACEMENT_3D('',#31865,#25706,#25707);
#23515=AXIS2_PLACEMENT_3D('',#31871,#25711,#25712);
#23516=AXIS2_PLACEMENT_3D('',#31874,#25714,#25715);
#23517=AXIS2_PLACEMENT_3D('',#31875,#25716,#25717);
#23518=AXIS2_PLACEMENT_3D('',#31879,#25720,#25721);
#23519=AXIS2_PLACEMENT_3D('',#31882,#25723,#25724);
#23520=AXIS2_PLACEMENT_3D('',#31883,#25725,#25726);
#23521=AXIS2_PLACEMENT_3D('',#31885,#25727,#25728);
#23522=AXIS2_PLACEMENT_3D('',#31887,#25729,#25730);
#23523=AXIS2_PLACEMENT_3D('',#31889,#25731,#25732);
#23524=AXIS2_PLACEMENT_3D('',#31891,#25733,#25734);
#23525=AXIS2_PLACEMENT_3D('',#31893,#25735,#25736);
#23526=AXIS2_PLACEMENT_3D('',#31895,#25737,#25738);
#23527=AXIS2_PLACEMENT_3D('',#31897,#25739,#25740);
#23528=AXIS2_PLACEMENT_3D('',#31898,#25741,#25742);
#23529=AXIS2_PLACEMENT_3D('',#31903,#25745,#25746);
#23530=AXIS2_PLACEMENT_3D('',#31904,#25747,#25748);
#23531=AXIS2_PLACEMENT_3D('',#31908,#25751,#25752);
#23532=AXIS2_PLACEMENT_3D('',#31911,#25754,#25755);
#23533=AXIS2_PLACEMENT_3D('',#31912,#25756,#25757);
#23534=AXIS2_PLACEMENT_3D('',#31916,#25760,#25761);
#23535=AXIS2_PLACEMENT_3D('',#31920,#25763,#25764);
#23536=AXIS2_PLACEMENT_3D('',#31921,#25765,#25766);
#23537=AXIS2_PLACEMENT_3D('',#31922,#25767,#25768);
#23538=AXIS2_PLACEMENT_3D('',#31928,#25772,#25773);
#23539=AXIS2_PLACEMENT_3D('',#31932,#25775,#25776);
#23540=AXIS2_PLACEMENT_3D('',#31933,#25777,#25778);
#23541=AXIS2_PLACEMENT_3D('',#31934,#25779,#25780);
#23542=AXIS2_PLACEMENT_3D('',#31937,#25783,#25784);
#23543=AXIS2_PLACEMENT_3D('',#31943,#25788,#25789);
#23544=AXIS2_PLACEMENT_3D('',#31946,#25791,#25792);
#23545=AXIS2_PLACEMENT_3D('',#31947,#25793,#25794);
#23546=AXIS2_PLACEMENT_3D('',#31951,#25797,#25798);
#23547=AXIS2_PLACEMENT_3D('',#31954,#25800,#25801);
#23548=AXIS2_PLACEMENT_3D('',#31955,#25802,#25803);
#23549=AXIS2_PLACEMENT_3D('',#31958,#25806,#25807);
#23550=AXIS2_PLACEMENT_3D('',#31960,#25809,#25810);
#23551=AXIS2_PLACEMENT_3D('',#31961,#25811,#25812);
#23552=AXIS2_PLACEMENT_3D('',#31970,#25817,#25818);
#23553=AXIS2_PLACEMENT_3D('',#31974,#25820,#25821);
#23554=AXIS2_PLACEMENT_3D('',#31975,#25822,#25823);
#23555=AXIS2_PLACEMENT_3D('',#31976,#25824,#25825);
#23556=AXIS2_PLACEMENT_3D('',#31982,#25829,#25830);
#23557=AXIS2_PLACEMENT_3D('',#31986,#25832,#25833);
#23558=AXIS2_PLACEMENT_3D('',#31987,#25834,#25835);
#23559=AXIS2_PLACEMENT_3D('',#31988,#25836,#25837);
#23560=AXIS2_PLACEMENT_3D('',#31994,#25841,#25842);
#23561=AXIS2_PLACEMENT_3D('',#31998,#25844,#25845);
#23562=AXIS2_PLACEMENT_3D('',#31999,#25846,#25847);
#23563=AXIS2_PLACEMENT_3D('',#32000,#25848,#25849);
#23564=AXIS2_PLACEMENT_3D('',#32006,#25853,#25854);
#23565=AXIS2_PLACEMENT_3D('',#32007,#25855,#25856);
#23566=AXIS2_PLACEMENT_3D('',#32008,#25857,#25858);
#23567=AXIS2_PLACEMENT_3D('',#32009,#25859,#25860);
#23568=AXIS2_PLACEMENT_3D('',#32013,#25862,#25863);
#23569=AXIS2_PLACEMENT_3D('',#32015,#25865,#25866);
#23570=AXIS2_PLACEMENT_3D('',#32019,#25869,#25870);
#23571=AXIS2_PLACEMENT_3D('',#32022,#25872,#25873);
#23572=AXIS2_PLACEMENT_3D('',#32023,#25874,#25875);
#23573=AXIS2_PLACEMENT_3D('',#32027,#25878,#25879);
#23574=AXIS2_PLACEMENT_3D('',#32029,#25880,#25881);
#23575=AXIS2_PLACEMENT_3D('',#32031,#25882,#25883);
#23576=AXIS2_PLACEMENT_3D('',#32033,#25884,#25885);
#23577=AXIS2_PLACEMENT_3D('',#32035,#25886,#25887);
#23578=AXIS2_PLACEMENT_3D('',#32037,#25888,#25889);
#23579=AXIS2_PLACEMENT_3D('',#32039,#25890,#25891);
#23580=AXIS2_PLACEMENT_3D('',#32041,#25892,#25893);
#23581=AXIS2_PLACEMENT_3D('',#32042,#25894,#25895);
#23582=AXIS2_PLACEMENT_3D('',#32045,#25898,#25899);
#23583=AXIS2_PLACEMENT_3D('',#32047,#25901,#25902);
#23584=AXIS2_PLACEMENT_3D('',#32049,#25904,#25905);
#23585=AXIS2_PLACEMENT_3D('',#32051,#25907,#25908);
#23586=AXIS2_PLACEMENT_3D('',#32057,#25912,#25913);
#23587=AXIS2_PLACEMENT_3D('',#32061,#25915,#25916);
#23588=AXIS2_PLACEMENT_3D('',#32062,#25917,#25918);
#23589=AXIS2_PLACEMENT_3D('',#32063,#25919,#25920);
#23590=AXIS2_PLACEMENT_3D('',#32069,#25924,#25925);
#23591=AXIS2_PLACEMENT_3D('',#32070,#25926,#25927);
#23592=AXIS2_PLACEMENT_3D('',#32071,#25928,#25929);
#23593=AXIS2_PLACEMENT_3D('',#32072,#25930,#25931);
#23594=AXIS2_PLACEMENT_3D('',#32075,#25934,#25935);
#23595=AXIS2_PLACEMENT_3D('',#32077,#25937,#25938);
#23596=AXIS2_PLACEMENT_3D('',#32078,#25939,#25940);
#23597=AXIS2_PLACEMENT_3D('',#32082,#25942,#25943);
#23598=AXIS2_PLACEMENT_3D('',#32083,#25944,#25945);
#23599=AXIS2_PLACEMENT_3D('',#32084,#25946,#25947);
#23600=AXIS2_PLACEMENT_3D('',#32086,#25948,#25949);
#23601=AXIS2_PLACEMENT_3D('',#32088,#25951,#25952);
#23602=AXIS2_PLACEMENT_3D('',#32092,#25954,#25955);
#23603=AXIS2_PLACEMENT_3D('',#32093,#25956,#25957);
#23604=AXIS2_PLACEMENT_3D('',#32094,#25958,#25959);
#23605=AXIS2_PLACEMENT_3D('',#32096,#25960,#25961);
#23606=AXIS2_PLACEMENT_3D('',#32098,#25963,#25964);
#23607=AXIS2_PLACEMENT_3D('',#32102,#25966,#25967);
#23608=AXIS2_PLACEMENT_3D('',#32103,#25968,#25969);
#23609=AXIS2_PLACEMENT_3D('',#32104,#25970,#25971);
#23610=AXIS2_PLACEMENT_3D('',#32106,#25972,#25973);
#23611=AXIS2_PLACEMENT_3D('',#32108,#25975,#25976);
#23612=AXIS2_PLACEMENT_3D('',#32112,#25978,#25979);
#23613=AXIS2_PLACEMENT_3D('',#32113,#25980,#25981);
#23614=AXIS2_PLACEMENT_3D('',#32114,#25982,#25983);
#23615=AXIS2_PLACEMENT_3D('',#32116,#25984,#25985);
#23616=AXIS2_PLACEMENT_3D('',#32118,#25987,#25988);
#23617=AXIS2_PLACEMENT_3D('',#32122,#25990,#25991);
#23618=AXIS2_PLACEMENT_3D('',#32123,#25992,#25993);
#23619=AXIS2_PLACEMENT_3D('',#32124,#25994,#25995);
#23620=AXIS2_PLACEMENT_3D('',#32126,#25996,#25997);
#23621=AXIS2_PLACEMENT_3D('',#32128,#25999,#26000);
#23622=AXIS2_PLACEMENT_3D('',#32132,#26002,#26003);
#23623=AXIS2_PLACEMENT_3D('',#32133,#26004,#26005);
#23624=AXIS2_PLACEMENT_3D('',#32134,#26006,#26007);
#23625=AXIS2_PLACEMENT_3D('',#32136,#26008,#26009);
#23626=AXIS2_PLACEMENT_3D('',#32138,#26011,#26012);
#23627=AXIS2_PLACEMENT_3D('',#32142,#26014,#26015);
#23628=AXIS2_PLACEMENT_3D('',#32143,#26016,#26017);
#23629=AXIS2_PLACEMENT_3D('',#32144,#26018,#26019);
#23630=AXIS2_PLACEMENT_3D('',#32146,#26020,#26021);
#23631=AXIS2_PLACEMENT_3D('',#32148,#26023,#26024);
#23632=AXIS2_PLACEMENT_3D('',#32151,#26026,#26027);
#23633=AXIS2_PLACEMENT_3D('',#32152,#26028,#26029);
#23634=AXIS2_PLACEMENT_3D('',#32155,#26031,#26032);
#23635=AXIS2_PLACEMENT_3D('',#32156,#26033,#26034);
#23636=AXIS2_PLACEMENT_3D('',#32159,#26036,#26037);
#23637=AXIS2_PLACEMENT_3D('',#32160,#26038,#26039);
#23638=AXIS2_PLACEMENT_3D('',#32161,#26040,#26041);
#23639=AXIS2_PLACEMENT_3D('',#32164,#26043,#26044);
#23640=AXIS2_PLACEMENT_3D('',#32165,#26045,#26046);
#23641=AXIS2_PLACEMENT_3D('',#32168,#26048,#26049);
#23642=AXIS2_PLACEMENT_3D('',#32169,#26050,#26051);
#23643=AXIS2_PLACEMENT_3D('',#32172,#26053,#26054);
#23644=AXIS2_PLACEMENT_3D('',#32173,#26055,#26056);
#23645=AXIS2_PLACEMENT_3D('',#32174,#26057,#26058);
#23646=AXIS2_PLACEMENT_3D('',#32177,#26060,#26061);
#23647=AXIS2_PLACEMENT_3D('',#32178,#26062,#26063);
#23648=AXIS2_PLACEMENT_3D('',#32181,#26065,#26066);
#23649=AXIS2_PLACEMENT_3D('',#32182,#26067,#26068);
#23650=AXIS2_PLACEMENT_3D('',#32185,#26070,#26071);
#23651=AXIS2_PLACEMENT_3D('',#32186,#26072,#26073);
#23652=AXIS2_PLACEMENT_3D('',#32187,#26074,#26075);
#23653=AXIS2_PLACEMENT_3D('',#32190,#26077,#26078);
#23654=AXIS2_PLACEMENT_3D('',#32191,#26079,#26080);
#23655=AXIS2_PLACEMENT_3D('',#32194,#26082,#26083);
#23656=AXIS2_PLACEMENT_3D('',#32195,#26084,#26085);
#23657=AXIS2_PLACEMENT_3D('',#32198,#26087,#26088);
#23658=AXIS2_PLACEMENT_3D('',#32199,#26089,#26090);
#23659=AXIS2_PLACEMENT_3D('',#32200,#26091,#26092);
#23660=AXIS2_PLACEMENT_3D('',#32203,#26094,#26095);
#23661=AXIS2_PLACEMENT_3D('',#32204,#26096,#26097);
#23662=AXIS2_PLACEMENT_3D('',#32207,#26099,#26100);
#23663=AXIS2_PLACEMENT_3D('',#32208,#26101,#26102);
#23664=AXIS2_PLACEMENT_3D('',#32211,#26104,#26105);
#23665=AXIS2_PLACEMENT_3D('',#32212,#26106,#26107);
#23666=AXIS2_PLACEMENT_3D('',#32213,#26108,#26109);
#23667=AXIS2_PLACEMENT_3D('',#32216,#26111,#26112);
#23668=AXIS2_PLACEMENT_3D('',#32217,#26113,#26114);
#23669=AXIS2_PLACEMENT_3D('',#32220,#26116,#26117);
#23670=AXIS2_PLACEMENT_3D('',#32221,#26118,#26119);
#23671=AXIS2_PLACEMENT_3D('',#32224,#26121,#26122);
#23672=AXIS2_PLACEMENT_3D('',#32225,#26123,#26124);
#23673=AXIS2_PLACEMENT_3D('',#32226,#26125,#26126);
#23674=AXIS2_PLACEMENT_3D('',#32229,#26128,#26129);
#23675=AXIS2_PLACEMENT_3D('',#32230,#26130,#26131);
#23676=AXIS2_PLACEMENT_3D('',#32233,#26133,#26134);
#23677=AXIS2_PLACEMENT_3D('',#32234,#26135,#26136);
#23678=AXIS2_PLACEMENT_3D('',#32237,#26138,#26139);
#23679=AXIS2_PLACEMENT_3D('',#32238,#26140,#26141);
#23680=AXIS2_PLACEMENT_3D('',#32239,#26142,#26143);
#23681=AXIS2_PLACEMENT_3D('',#32240,#26144,#26145);
#23682=AXIS2_PLACEMENT_3D('',#32241,#26146,#26147);
#23683=AXIS2_PLACEMENT_3D('',#32243,#26149,#26150);
#23684=AXIS2_PLACEMENT_3D('',#32245,#26152,#26153);
#23685=AXIS2_PLACEMENT_3D('',#32247,#26155,#26156);
#23686=AXIS2_PLACEMENT_3D('',#32248,#26157,#26158);
#23687=AXIS2_PLACEMENT_3D('',#32249,#26159,#26160);
#23688=AXIS2_PLACEMENT_3D('',#32258,#26165,#26166);
#23689=AXIS2_PLACEMENT_3D('',#32264,#26170,#26171);
#23690=AXIS2_PLACEMENT_3D('',#32268,#26173,#26174);
#23691=AXIS2_PLACEMENT_3D('',#32269,#26175,#26176);
#23692=AXIS2_PLACEMENT_3D('',#32270,#26177,#26178);
#23693=AXIS2_PLACEMENT_3D('',#32276,#26182,#26183);
#23694=AXIS2_PLACEMENT_3D('',#32280,#26185,#26186);
#23695=AXIS2_PLACEMENT_3D('',#32281,#26187,#26188);
#23696=AXIS2_PLACEMENT_3D('',#32282,#26189,#26190);
#23697=AXIS2_PLACEMENT_3D('',#32285,#26193,#26194);
#23698=AXIS2_PLACEMENT_3D('',#32289,#26196,#26197);
#23699=AXIS2_PLACEMENT_3D('',#32291,#26199,#26200);
#23700=AXIS2_PLACEMENT_3D('',#32295,#26203,#26204);
#23701=AXIS2_PLACEMENT_3D('',#32299,#26207,#26208);
#23702=AXIS2_PLACEMENT_3D('',#32301,#26209,#26210);
#23703=AXIS2_PLACEMENT_3D('',#32303,#26211,#26212);
#23704=AXIS2_PLACEMENT_3D('',#32305,#26213,#26214);
#23705=AXIS2_PLACEMENT_3D('',#32307,#26215,#26216);
#23706=AXIS2_PLACEMENT_3D('',#32309,#26217,#26218);
#23707=AXIS2_PLACEMENT_3D('',#32311,#26219,#26220);
#23708=AXIS2_PLACEMENT_3D('',#32313,#26221,#26222);
#23709=AXIS2_PLACEMENT_3D('',#32314,#26223,#26224);
#23710=AXIS2_PLACEMENT_3D('',#32324,#26230,#26231);
#23711=AXIS2_PLACEMENT_3D('',#32331,#26235,#26236);
#23712=AXIS2_PLACEMENT_3D('',#32333,#26237,#26238);
#23713=AXIS2_PLACEMENT_3D('',#32335,#26239,#26240);
#23714=AXIS2_PLACEMENT_3D('',#32336,#26241,#26242);
#23715=AXIS2_PLACEMENT_3D('',#32344,#26247,#26248);
#23716=AXIS2_PLACEMENT_3D('',#32350,#26252,#26253);
#23717=AXIS2_PLACEMENT_3D('',#32356,#26257,#26258);
#23718=AXIS2_PLACEMENT_3D('',#32359,#26260,#26261);
#23719=AXIS2_PLACEMENT_3D('',#32360,#26262,#26263);
#23720=AXIS2_PLACEMENT_3D('',#32366,#26267,#26268);
#23721=AXIS2_PLACEMENT_3D('',#32367,#26269,#26270);
#23722=AXIS2_PLACEMENT_3D('',#32368,#26271,#26272);
#23723=AXIS2_PLACEMENT_3D('',#32369,#26273,#26274);
#23724=AXIS2_PLACEMENT_3D('',#32371,#26276,#26277);
#23725=AXIS2_PLACEMENT_3D('',#32373,#26279,#26280);
#23726=AXIS2_PLACEMENT_3D('',#32374,#26281,#26282);
#23727=AXIS2_PLACEMENT_3D('',#32382,#26287,#26288);
#23728=AXIS2_PLACEMENT_3D('',#32386,#26291,#26292);
#23729=AXIS2_PLACEMENT_3D('',#32390,#26295,#26296);
#23730=AXIS2_PLACEMENT_3D('',#32394,#26299,#26300);
#23731=AXIS2_PLACEMENT_3D('',#32400,#26304,#26305);
#23732=AXIS2_PLACEMENT_3D('',#32404,#26307,#26308);
#23733=AXIS2_PLACEMENT_3D('',#32405,#26309,#26310);
#23734=AXIS2_PLACEMENT_3D('',#32406,#26311,#26312);
#23735=AXIS2_PLACEMENT_3D('',#32412,#26316,#26317);
#23736=AXIS2_PLACEMENT_3D('',#32413,#26318,#26319);
#23737=AXIS2_PLACEMENT_3D('',#32414,#26320,#26321);
#23738=AXIS2_PLACEMENT_3D('',#32415,#26322,#26323);
#23739=AXIS2_PLACEMENT_3D('',#32419,#26325,#26326);
#23740=AXIS2_PLACEMENT_3D('',#32421,#26328,#26329);
#23741=AXIS2_PLACEMENT_3D('',#32425,#26332,#26333);
#23742=AXIS2_PLACEMENT_3D('',#32429,#26336,#26337);
#23743=AXIS2_PLACEMENT_3D('',#32432,#26340,#26341);
#23744=AXIS2_PLACEMENT_3D('',#32433,#26342,#26343);
#23745=AXIS2_PLACEMENT_3D('',#32439,#26347,#26348);
#23746=AXIS2_PLACEMENT_3D('',#32443,#26351,#26352);
#23747=AXIS2_PLACEMENT_3D('',#32446,#26354,#26355);
#23748=AXIS2_PLACEMENT_3D('',#32447,#26356,#26357);
#23749=AXIS2_PLACEMENT_3D('',#32453,#26361,#26362);
#23750=AXIS2_PLACEMENT_3D('',#32457,#26364,#26365);
#23751=AXIS2_PLACEMENT_3D('',#32458,#26366,#26367);
#23752=AXIS2_PLACEMENT_3D('',#32459,#26368,#26369);
#23753=AXIS2_PLACEMENT_3D('',#32462,#26372,#26373);
#23754=AXIS2_PLACEMENT_3D('',#32465,#26376,#26377);
#23755=AXIS2_PLACEMENT_3D('',#32466,#26378,#26379);
#23756=AXIS2_PLACEMENT_3D('',#32468,#26380,#26381);
#23757=AXIS2_PLACEMENT_3D('',#32470,#26382,#26383);
#23758=AXIS2_PLACEMENT_3D('',#32472,#26384,#26385);
#23759=AXIS2_PLACEMENT_3D('',#32474,#26386,#26387);
#23760=AXIS2_PLACEMENT_3D('',#32476,#26388,#26389);
#23761=AXIS2_PLACEMENT_3D('',#32478,#26390,#26391);
#23762=AXIS2_PLACEMENT_3D('',#32480,#26392,#26393);
#23763=AXIS2_PLACEMENT_3D('',#32482,#26394,#26395);
#23764=AXIS2_PLACEMENT_3D('',#32484,#26396,#26397);
#23765=AXIS2_PLACEMENT_3D('',#32486,#26398,#26399);
#23766=AXIS2_PLACEMENT_3D('',#32487,#26400,#26401);
#23767=AXIS2_PLACEMENT_3D('',#32490,#26403,#26404);
#23768=AXIS2_PLACEMENT_3D('',#32491,#26405,#26406);
#23769=AXIS2_PLACEMENT_3D('',#32494,#26408,#26409);
#23770=AXIS2_PLACEMENT_3D('',#32495,#26410,#26411);
#23771=AXIS2_PLACEMENT_3D('',#32499,#26413,#26414);
#23772=AXIS2_PLACEMENT_3D('',#32500,#26415,#26416);
#23773=AXIS2_PLACEMENT_3D('',#32501,#26417,#26418);
#23774=AXIS2_PLACEMENT_3D('',#32503,#26419,#26420);
#23775=AXIS2_PLACEMENT_3D('',#32505,#26422,#26423);
#23776=AXIS2_PLACEMENT_3D('',#32508,#26425,#26426);
#23777=AXIS2_PLACEMENT_3D('',#32509,#26427,#26428);
#23778=AXIS2_PLACEMENT_3D('',#32510,#26429,#26430);
#23779=AXIS2_PLACEMENT_3D('',#32514,#26432,#26433);
#23780=AXIS2_PLACEMENT_3D('',#32515,#26434,#26435);
#23781=AXIS2_PLACEMENT_3D('',#32516,#26436,#26437);
#23782=AXIS2_PLACEMENT_3D('',#32518,#26438,#26439);
#23783=AXIS2_PLACEMENT_3D('',#32520,#26441,#26442);
#23784=AXIS2_PLACEMENT_3D('',#32522,#26444,#26445);
#23785=AXIS2_PLACEMENT_3D('',#32526,#26447,#26448);
#23786=AXIS2_PLACEMENT_3D('',#32527,#26449,#26450);
#23787=AXIS2_PLACEMENT_3D('',#32528,#26451,#26452);
#23788=AXIS2_PLACEMENT_3D('',#32530,#26453,#26454);
#23789=AXIS2_PLACEMENT_3D('',#32532,#26456,#26457);
#23790=AXIS2_PLACEMENT_3D('',#32534,#26459,#26460);
#23791=AXIS2_PLACEMENT_3D('',#32538,#26462,#26463);
#23792=AXIS2_PLACEMENT_3D('',#32539,#26464,#26465);
#23793=AXIS2_PLACEMENT_3D('',#32540,#26466,#26467);
#23794=AXIS2_PLACEMENT_3D('',#32542,#26468,#26469);
#23795=AXIS2_PLACEMENT_3D('',#32544,#26471,#26472);
#23796=AXIS2_PLACEMENT_3D('',#32546,#26474,#26475);
#23797=AXIS2_PLACEMENT_3D('',#32549,#26477,#26478);
#23798=AXIS2_PLACEMENT_3D('',#32550,#26479,#26480);
#23799=AXIS2_PLACEMENT_3D('',#32553,#26482,#26483);
#23800=AXIS2_PLACEMENT_3D('',#32554,#26484,#26485);
#23801=AXIS2_PLACEMENT_3D('',#32557,#26487,#26488);
#23802=AXIS2_PLACEMENT_3D('',#32558,#26489,#26490);
#23803=AXIS2_PLACEMENT_3D('',#32561,#26492,#26493);
#23804=AXIS2_PLACEMENT_3D('',#32562,#26494,#26495);
#23805=AXIS2_PLACEMENT_3D('',#32565,#26497,#26498);
#23806=AXIS2_PLACEMENT_3D('',#32566,#26499,#26500);
#23807=AXIS2_PLACEMENT_3D('',#32569,#26502,#26503);
#23808=AXIS2_PLACEMENT_3D('',#32570,#26504,#26505);
#23809=AXIS2_PLACEMENT_3D('',#32572,#26506,#26507);
#23810=AXIS2_PLACEMENT_3D('',#32575,#26509,#26510);
#23811=AXIS2_PLACEMENT_3D('',#32576,#26511,#26512);
#23812=AXIS2_PLACEMENT_3D('',#32579,#26513,#26514);
#23813=AXIS2_PLACEMENT_3D('',#32580,#26515,#26516);
#23814=AXIS2_PLACEMENT_3D('',#32582,#26518,#26519);
#23815=AXIS2_PLACEMENT_3D('',#32584,#26521,#26522);
#23816=AXIS2_PLACEMENT_3D('',#32587,#26523,#26524);
#23817=AXIS2_PLACEMENT_3D('',#32588,#26525,#26526);
#23818=AXIS2_PLACEMENT_3D('',#32590,#26528,#26529);
#23819=AXIS2_PLACEMENT_3D('',#32592,#26530,#26531);
#23820=AXIS2_PLACEMENT_3D('',#32594,#26533,#26534);
#23821=AXIS2_PLACEMENT_3D('',#32597,#26536,#26537);
#23822=AXIS2_PLACEMENT_3D('',#32601,#26539,#26540);
#23823=AXIS2_PLACEMENT_3D('',#32602,#26541,#26542);
#23824=AXIS2_PLACEMENT_3D('',#32605,#26544,#26545);
#23825=AXIS2_PLACEMENT_3D('',#32606,#26546,#26547);
#23826=AXIS2_PLACEMENT_3D('',#32608,#26549,#26550);
#23827=AXIS2_PLACEMENT_3D('',#32612,#26552,#26553);
#23828=AXIS2_PLACEMENT_3D('',#32613,#26554,#26555);
#23829=AXIS2_PLACEMENT_3D('',#32616,#26557,#26558);
#23830=AXIS2_PLACEMENT_3D('',#32617,#26559,#26560);
#23831=AXIS2_PLACEMENT_3D('',#32619,#26562,#26563);
#23832=AXIS2_PLACEMENT_3D('',#32623,#26565,#26566);
#23833=AXIS2_PLACEMENT_3D('',#32624,#26567,#26568);
#23834=AXIS2_PLACEMENT_3D('',#32627,#26570,#26571);
#23835=AXIS2_PLACEMENT_3D('',#32628,#26572,#26573);
#23836=AXIS2_PLACEMENT_3D('',#32630,#26575,#26576);
#23837=AXIS2_PLACEMENT_3D('',#32632,#26578,#26579);
#23838=AXIS2_PLACEMENT_3D('',#32634,#26581,#26582);
#23839=AXIS2_PLACEMENT_3D('',#32636,#26584,#26585);
#23840=AXIS2_PLACEMENT_3D('',#32640,#26587,#26588);
#23841=AXIS2_PLACEMENT_3D('',#32641,#26589,#26590);
#23842=AXIS2_PLACEMENT_3D('',#32644,#26592,#26593);
#23843=AXIS2_PLACEMENT_3D('',#32645,#26594,#26595);
#23844=AXIS2_PLACEMENT_3D('',#32647,#26597,#26598);
#23845=AXIS2_PLACEMENT_3D('',#32651,#26600,#26601);
#23846=AXIS2_PLACEMENT_3D('',#32652,#26602,#26603);
#23847=AXIS2_PLACEMENT_3D('',#32655,#26605,#26606);
#23848=AXIS2_PLACEMENT_3D('',#32656,#26607,#26608);
#23849=AXIS2_PLACEMENT_3D('',#32658,#26610,#26611);
#23850=AXIS2_PLACEMENT_3D('',#32662,#26613,#26614);
#23851=AXIS2_PLACEMENT_3D('',#32663,#26615,#26616);
#23852=AXIS2_PLACEMENT_3D('',#32666,#26618,#26619);
#23853=AXIS2_PLACEMENT_3D('',#32667,#26620,#26621);
#23854=AXIS2_PLACEMENT_3D('',#32669,#26623,#26624);
#23855=AXIS2_PLACEMENT_3D('',#32670,#26625,#26626);
#23856=AXIS2_PLACEMENT_3D('',#32671,#26627,#26628);
#23857=AXIS2_PLACEMENT_3D('',#32672,#26629,#26630);
#23858=AXIS2_PLACEMENT_3D('',#32677,#26632,#26633);
#23859=AXIS2_PLACEMENT_3D('',#32680,#26635,#26636);
#23860=AXIS2_PLACEMENT_3D('',#32681,#26637,#26638);
#23861=AXIS2_PLACEMENT_3D('',#32687,#26642,#26643);
#23862=AXIS2_PLACEMENT_3D('',#32691,#26645,#26646);
#23863=AXIS2_PLACEMENT_3D('',#32692,#26647,#26648);
#23864=AXIS2_PLACEMENT_3D('',#32693,#26649,#26650);
#23865=AXIS2_PLACEMENT_3D('',#32699,#26654,#26655);
#23866=AXIS2_PLACEMENT_3D('',#32703,#26657,#26658);
#23867=AXIS2_PLACEMENT_3D('',#32704,#26659,#26660);
#23868=AXIS2_PLACEMENT_3D('',#32705,#26661,#26662);
#23869=AXIS2_PLACEMENT_3D('',#32711,#26666,#26667);
#23870=AXIS2_PLACEMENT_3D('',#32715,#26669,#26670);
#23871=AXIS2_PLACEMENT_3D('',#32716,#26671,#26672);
#23872=AXIS2_PLACEMENT_3D('',#32717,#26673,#26674);
#23873=AXIS2_PLACEMENT_3D('',#32720,#26677,#26678);
#23874=AXIS2_PLACEMENT_3D('',#32726,#26682,#26683);
#23875=AXIS2_PLACEMENT_3D('',#32729,#26685,#26686);
#23876=AXIS2_PLACEMENT_3D('',#32730,#26687,#26688);
#23877=AXIS2_PLACEMENT_3D('',#32734,#26691,#26692);
#23878=AXIS2_PLACEMENT_3D('',#32737,#26694,#26695);
#23879=AXIS2_PLACEMENT_3D('',#32738,#26696,#26697);
#23880=AXIS2_PLACEMENT_3D('',#32740,#26698,#26699);
#23881=AXIS2_PLACEMENT_3D('',#32742,#26700,#26701);
#23882=AXIS2_PLACEMENT_3D('',#32744,#26702,#26703);
#23883=AXIS2_PLACEMENT_3D('',#32746,#26704,#26705);
#23884=AXIS2_PLACEMENT_3D('',#32747,#26706,#26707);
#23885=AXIS2_PLACEMENT_3D('',#32756,#26712,#26713);
#23886=AXIS2_PLACEMENT_3D('',#32760,#26715,#26716);
#23887=AXIS2_PLACEMENT_3D('',#32761,#26717,#26718);
#23888=AXIS2_PLACEMENT_3D('',#32762,#26719,#26720);
#23889=AXIS2_PLACEMENT_3D('',#32767,#26724,#26725);
#23890=AXIS2_PLACEMENT_3D('',#32770,#26727,#26728);
#23891=AXIS2_PLACEMENT_3D('',#32771,#26729,#26730);
#23892=AXIS2_PLACEMENT_3D('',#32775,#26733,#26734);
#23893=AXIS2_PLACEMENT_3D('',#32778,#26736,#26737);
#23894=AXIS2_PLACEMENT_3D('',#32779,#26738,#26739);
#23895=AXIS2_PLACEMENT_3D('',#32783,#26742,#26743);
#23896=AXIS2_PLACEMENT_3D('',#32784,#26744,#26745);
#23897=AXIS2_PLACEMENT_3D('',#32785,#26746,#26747);
#23898=AXIS2_PLACEMENT_3D('',#32786,#26748,#26749);
#23899=AXIS2_PLACEMENT_3D('',#32790,#26751,#26752);
#23900=AXIS2_PLACEMENT_3D('',#32792,#26754,#26755);
#23901=AXIS2_PLACEMENT_3D('',#32796,#26758,#26759);
#23902=AXIS2_PLACEMENT_3D('',#32799,#26761,#26762);
#23903=AXIS2_PLACEMENT_3D('',#32800,#26763,#26764);
#23904=AXIS2_PLACEMENT_3D('',#32804,#26767,#26768);
#23905=AXIS2_PLACEMENT_3D('',#32806,#26770,#26771);
#23906=AXIS2_PLACEMENT_3D('',#32808,#26773,#26774);
#23907=AXIS2_PLACEMENT_3D('',#32812,#26776,#26777);
#23908=AXIS2_PLACEMENT_3D('',#32814,#26779,#26780);
#23909=AXIS2_PLACEMENT_3D('',#32818,#26783,#26784);
#23910=AXIS2_PLACEMENT_3D('',#32821,#26786,#26787);
#23911=AXIS2_PLACEMENT_3D('',#32822,#26788,#26789);
#23912=AXIS2_PLACEMENT_3D('',#32826,#26792,#26793);
#23913=AXIS2_PLACEMENT_3D('',#32830,#26795,#26796);
#23914=AXIS2_PLACEMENT_3D('',#32831,#26797,#26798);
#23915=AXIS2_PLACEMENT_3D('',#32832,#26799,#26800);
#23916=AXIS2_PLACEMENT_3D('',#32838,#26804,#26805);
#23917=AXIS2_PLACEMENT_3D('',#32842,#26807,#26808);
#23918=AXIS2_PLACEMENT_3D('',#32843,#26809,#26810);
#23919=AXIS2_PLACEMENT_3D('',#32844,#26811,#26812);
#23920=AXIS2_PLACEMENT_3D('',#32847,#26815,#26816);
#23921=AXIS2_PLACEMENT_3D('',#32853,#26820,#26821);
#23922=AXIS2_PLACEMENT_3D('',#32856,#26823,#26824);
#23923=AXIS2_PLACEMENT_3D('',#32857,#26825,#26826);
#23924=AXIS2_PLACEMENT_3D('',#32861,#26829,#26830);
#23925=AXIS2_PLACEMENT_3D('',#32864,#26832,#26833);
#23926=AXIS2_PLACEMENT_3D('',#32865,#26834,#26835);
#23927=AXIS2_PLACEMENT_3D('',#32869,#26837,#26838);
#23928=AXIS2_PLACEMENT_3D('',#32870,#26839,#26840);
#23929=AXIS2_PLACEMENT_3D('',#32871,#26841,#26842);
#23930=AXIS2_PLACEMENT_3D('',#32873,#26843,#26844);
#23931=AXIS2_PLACEMENT_3D('',#32875,#26846,#26847);
#23932=AXIS2_PLACEMENT_3D('',#32880,#26850,#26851);
#23933=AXIS2_PLACEMENT_3D('',#32881,#26852,#26853);
#23934=AXIS2_PLACEMENT_3D('',#32885,#26856,#26857);
#23935=AXIS2_PLACEMENT_3D('',#32888,#26859,#26860);
#23936=AXIS2_PLACEMENT_3D('',#32889,#26861,#26862);
#23937=AXIS2_PLACEMENT_3D('',#32893,#26865,#26866);
#23938=AXIS2_PLACEMENT_3D('',#32897,#26868,#26869);
#23939=AXIS2_PLACEMENT_3D('',#32898,#26870,#26871);
#23940=AXIS2_PLACEMENT_3D('',#32899,#26872,#26873);
#23941=AXIS2_PLACEMENT_3D('',#32905,#26877,#26878);
#23942=AXIS2_PLACEMENT_3D('',#32909,#26880,#26881);
#23943=AXIS2_PLACEMENT_3D('',#32910,#26882,#26883);
#23944=AXIS2_PLACEMENT_3D('',#32911,#26884,#26885);
#23945=AXIS2_PLACEMENT_3D('',#32914,#26888,#26889);
#23946=AXIS2_PLACEMENT_3D('',#32917,#26892,#26893);
#23947=AXIS2_PLACEMENT_3D('',#32919,#26895,#26896);
#23948=AXIS2_PLACEMENT_3D('',#32920,#26897,#26898);
#23949=AXIS2_PLACEMENT_3D('',#32922,#26899,#26900);
#23950=AXIS2_PLACEMENT_3D('',#32923,#26901,#26902);
#23951=AXIS2_PLACEMENT_3D('',#32925,#26903,#26904);
#23952=AXIS2_PLACEMENT_3D('',#32928,#26906,#26907);
#23953=AXIS2_PLACEMENT_3D('',#32929,#26908,#26909);
#23954=AXIS2_PLACEMENT_3D('',#32931,#26910,#26911);
#23955=AXIS2_PLACEMENT_3D('',#32933,#26913,#26914);
#23956=AXIS2_PLACEMENT_3D('',#32934,#26915,#26916);
#23957=AXIS2_PLACEMENT_3D('',#32936,#26917,#26918);
#23958=AXIS2_PLACEMENT_3D('',#32938,#26920,#26921);
#23959=AXIS2_PLACEMENT_3D('',#32941,#26923,#26924);
#23960=AXIS2_PLACEMENT_3D('',#32942,#26925,#26926);
#23961=AXIS2_PLACEMENT_3D('',#32944,#26928,#26929);
#23962=AXIS2_PLACEMENT_3D('',#32948,#26931,#26932);
#23963=AXIS2_PLACEMENT_3D('',#32949,#26933,#26934);
#23964=AXIS2_PLACEMENT_3D('',#32952,#26936,#26937);
#23965=AXIS2_PLACEMENT_3D('',#32953,#26938,#26939);
#23966=AXIS2_PLACEMENT_3D('',#32955,#26941,#26942);
#23967=AXIS2_PLACEMENT_3D('',#32959,#26944,#26945);
#23968=AXIS2_PLACEMENT_3D('',#32960,#26946,#26947);
#23969=AXIS2_PLACEMENT_3D('',#32963,#26949,#26950);
#23970=AXIS2_PLACEMENT_3D('',#32964,#26951,#26952);
#23971=AXIS2_PLACEMENT_3D('',#32966,#26954,#26955);
#23972=AXIS2_PLACEMENT_3D('',#32970,#26957,#26958);
#23973=AXIS2_PLACEMENT_3D('',#32971,#26959,#26960);
#23974=AXIS2_PLACEMENT_3D('',#32974,#26962,#26963);
#23975=AXIS2_PLACEMENT_3D('',#32975,#26964,#26965);
#23976=AXIS2_PLACEMENT_3D('',#32977,#26967,#26968);
#23977=AXIS2_PLACEMENT_3D('',#32978,#26969,#26970);
#23978=AXIS2_PLACEMENT_3D('',#32980,#26972,#26973);
#23979=AXIS2_PLACEMENT_3D('',#32981,#26974,#26975);
#23980=AXIS2_PLACEMENT_3D('',#32984,#26978,#26979);
#23981=AXIS2_PLACEMENT_3D('',#32986,#26981,#26982);
#23982=AXIS2_PLACEMENT_3D('',#32987,#26983,#26984);
#23983=AXIS2_PLACEMENT_3D('',#32988,#26985,#26986);
#23984=AXIS2_PLACEMENT_3D('',#32989,#26987,#26988);
#23985=AXIS2_PLACEMENT_3D('',#32991,#26989,#26990);
#23986=AXIS2_PLACEMENT_3D('',#32995,#26992,#26993);
#23987=AXIS2_PLACEMENT_3D('',#32996,#26994,#26995);
#23988=AXIS2_PLACEMENT_3D('',#32997,#26996,#26997);
#23989=AXIS2_PLACEMENT_3D('',#33001,#26999,#27000);
#23990=AXIS2_PLACEMENT_3D('',#33002,#27001,#27002);
#23991=AXIS2_PLACEMENT_3D('',#33003,#27003,#27004);
#23992=AXIS2_PLACEMENT_3D('',#33006,#27006,#27007);
#23993=AXIS2_PLACEMENT_3D('',#33007,#27008,#27009);
#23994=AXIS2_PLACEMENT_3D('',#33009,#27010,#27011);
#23995=AXIS2_PLACEMENT_3D('',#33011,#27013,#27014);
#23996=AXIS2_PLACEMENT_3D('',#33013,#27015,#27016);
#23997=AXIS2_PLACEMENT_3D('',#33015,#27018,#27019);
#23998=AXIS2_PLACEMENT_3D('',#33018,#27021,#27022);
#23999=AXIS2_PLACEMENT_3D('',#33019,#27023,#27024);
#24000=AXIS2_PLACEMENT_3D('',#33021,#27025,#27026);
#24001=AXIS2_PLACEMENT_3D('',#33023,#27027,#27028);
#24002=AXIS2_PLACEMENT_3D('',#33025,#27029,#27030);
#24003=AXIS2_PLACEMENT_3D('',#33027,#27031,#27032);
#24004=AXIS2_PLACEMENT_3D('',#33028,#27033,#27034);
#24005=AXIS2_PLACEMENT_3D('',#33030,#27035,#27036);
#24006=AXIS2_PLACEMENT_3D('',#33032,#27038,#27039);
#24007=AXIS2_PLACEMENT_3D('',#33034,#27040,#27041);
#24008=AXIS2_PLACEMENT_3D('',#33036,#27043,#27044);
#24009=AXIS2_PLACEMENT_3D('',#33039,#27046,#27047);
#24010=AXIS2_PLACEMENT_3D('',#33040,#27048,#27049);
#24011=AXIS2_PLACEMENT_3D('',#33042,#27050,#27051);
#24012=AXIS2_PLACEMENT_3D('',#33043,#27052,#27053);
#24013=AXIS2_PLACEMENT_3D('',#33047,#27055,#27056);
#24014=AXIS2_PLACEMENT_3D('',#33048,#27057,#27058);
#24015=AXIS2_PLACEMENT_3D('',#33049,#27059,#27060);
#24016=AXIS2_PLACEMENT_3D('',#33052,#27061,#27062);
#24017=AXIS2_PLACEMENT_3D('',#33053,#27063,#27064);
#24018=AXIS2_PLACEMENT_3D('',#33055,#27066,#27067);
#24019=AXIS2_PLACEMENT_3D('',#33057,#27068,#27069);
#24020=AXIS2_PLACEMENT_3D('',#33059,#27071,#27072);
#24021=AXIS2_PLACEMENT_3D('',#33062,#27074,#27075);
#24022=AXIS2_PLACEMENT_3D('',#33063,#27076,#27077);
#24023=AXIS2_PLACEMENT_3D('',#33065,#27079,#27080);
#24024=AXIS2_PLACEMENT_3D('',#33069,#27082,#27083);
#24025=AXIS2_PLACEMENT_3D('',#33070,#27084,#27085);
#24026=AXIS2_PLACEMENT_3D('',#33073,#27087,#27088);
#24027=AXIS2_PLACEMENT_3D('',#33074,#27089,#27090);
#24028=AXIS2_PLACEMENT_3D('',#33076,#27092,#27093);
#24029=AXIS2_PLACEMENT_3D('',#33080,#27095,#27096);
#24030=AXIS2_PLACEMENT_3D('',#33081,#27097,#27098);
#24031=AXIS2_PLACEMENT_3D('',#33084,#27100,#27101);
#24032=AXIS2_PLACEMENT_3D('',#33085,#27102,#27103);
#24033=AXIS2_PLACEMENT_3D('',#33087,#27105,#27106);
#24034=AXIS2_PLACEMENT_3D('',#33091,#27108,#27109);
#24035=AXIS2_PLACEMENT_3D('',#33092,#27110,#27111);
#24036=AXIS2_PLACEMENT_3D('',#33095,#27113,#27114);
#24037=AXIS2_PLACEMENT_3D('',#33096,#27115,#27116);
#24038=AXIS2_PLACEMENT_3D('',#33098,#27118,#27119);
#24039=AXIS2_PLACEMENT_3D('',#33099,#27120,#27121);
#24040=AXIS2_PLACEMENT_3D('',#33101,#27122,#27123);
#24041=AXIS2_PLACEMENT_3D('',#33105,#27125,#27126);
#24042=AXIS2_PLACEMENT_3D('',#33106,#27127,#27128);
#24043=AXIS2_PLACEMENT_3D('',#33107,#27129,#27130);
#24044=AXIS2_PLACEMENT_3D('',#33109,#27131,#27132);
#24045=AXIS2_PLACEMENT_3D('',#33111,#27134,#27135);
#24046=AXIS2_PLACEMENT_3D('',#33113,#27136,#27137);
#24047=AXIS2_PLACEMENT_3D('',#33115,#27138,#27139);
#24048=AXIS2_PLACEMENT_3D('',#33117,#27140,#27141);
#24049=AXIS2_PLACEMENT_3D('',#33119,#27142,#27143);
#24050=AXIS2_PLACEMENT_3D('',#33121,#27144,#27145);
#24051=AXIS2_PLACEMENT_3D('',#33123,#27146,#27147);
#24052=AXIS2_PLACEMENT_3D('',#33125,#27148,#27149);
#24053=AXIS2_PLACEMENT_3D('',#33126,#27150,#27151);
#24054=AXIS2_PLACEMENT_3D('',#33128,#27152,#27153);
#24055=AXIS2_PLACEMENT_3D('',#33130,#27155,#27156);
#24056=AXIS2_PLACEMENT_3D('',#33132,#27157,#27158);
#24057=AXIS2_PLACEMENT_3D('',#33134,#27159,#27160);
#24058=AXIS2_PLACEMENT_3D('',#33136,#27161,#27162);
#24059=AXIS2_PLACEMENT_3D('',#33138,#27163,#27164);
#24060=AXIS2_PLACEMENT_3D('',#33140,#27165,#27166);
#24061=AXIS2_PLACEMENT_3D('',#33142,#27167,#27168);
#24062=AXIS2_PLACEMENT_3D('',#33144,#27169,#27170);
#24063=AXIS2_PLACEMENT_3D('',#33145,#27171,#27172);
#24064=AXIS2_PLACEMENT_3D('',#33149,#27174,#27175);
#24065=AXIS2_PLACEMENT_3D('',#33150,#27176,#27177);
#24066=AXIS2_PLACEMENT_3D('',#33151,#27178,#27179);
#24067=AXIS2_PLACEMENT_3D('',#33153,#27180,#27181);
#24068=AXIS2_PLACEMENT_3D('',#33155,#27183,#27184);
#24069=AXIS2_PLACEMENT_3D('',#33157,#27186,#27187);
#24070=AXIS2_PLACEMENT_3D('',#33161,#27189,#27190);
#24071=AXIS2_PLACEMENT_3D('',#33162,#27191,#27192);
#24072=AXIS2_PLACEMENT_3D('',#33163,#27193,#27194);
#24073=AXIS2_PLACEMENT_3D('',#33165,#27195,#27196);
#24074=AXIS2_PLACEMENT_3D('',#33167,#27198,#27199);
#24075=AXIS2_PLACEMENT_3D('',#33169,#27201,#27202);
#24076=AXIS2_PLACEMENT_3D('',#33173,#27204,#27205);
#24077=AXIS2_PLACEMENT_3D('',#33174,#27206,#27207);
#24078=AXIS2_PLACEMENT_3D('',#33175,#27208,#27209);
#24079=AXIS2_PLACEMENT_3D('',#33177,#27210,#27211);
#24080=AXIS2_PLACEMENT_3D('',#33179,#27213,#27214);
#24081=AXIS2_PLACEMENT_3D('',#33181,#27216,#27217);
#24082=AXIS2_PLACEMENT_3D('',#33185,#27219,#27220);
#24083=AXIS2_PLACEMENT_3D('',#33186,#27221,#27222);
#24084=AXIS2_PLACEMENT_3D('',#33187,#27223,#27224);
#24085=AXIS2_PLACEMENT_3D('',#33189,#27225,#27226);
#24086=AXIS2_PLACEMENT_3D('',#33191,#27228,#27229);
#24087=AXIS2_PLACEMENT_3D('',#33193,#27231,#27232);
#24088=AXIS2_PLACEMENT_3D('',#33197,#27234,#27235);
#24089=AXIS2_PLACEMENT_3D('',#33198,#27236,#27237);
#24090=AXIS2_PLACEMENT_3D('',#33199,#27238,#27239);
#24091=AXIS2_PLACEMENT_3D('',#33201,#27240,#27241);
#24092=AXIS2_PLACEMENT_3D('',#33203,#27243,#27244);
#24093=AXIS2_PLACEMENT_3D('',#33205,#27246,#27247);
#24094=AXIS2_PLACEMENT_3D('',#33209,#27249,#27250);
#24095=AXIS2_PLACEMENT_3D('',#33210,#27251,#27252);
#24096=AXIS2_PLACEMENT_3D('',#33211,#27253,#27254);
#24097=AXIS2_PLACEMENT_3D('',#33215,#27256,#27257);
#24098=AXIS2_PLACEMENT_3D('',#33216,#27258,#27259);
#24099=AXIS2_PLACEMENT_3D('',#33217,#27260,#27261);
#24100=AXIS2_PLACEMENT_3D('',#33219,#27263,#27264);
#24101=AXIS2_PLACEMENT_3D('',#33223,#27266,#27267);
#24102=AXIS2_PLACEMENT_3D('',#33224,#27268,#27269);
#24103=AXIS2_PLACEMENT_3D('',#33225,#27270,#27271);
#24104=AXIS2_PLACEMENT_3D('',#33228,#27272,#27273);
#24105=AXIS2_PLACEMENT_3D('',#33229,#27274,#27275);
#24106=AXIS2_PLACEMENT_3D('',#33231,#27277,#27278);
#24107=AXIS2_PLACEMENT_3D('',#33233,#27280,#27281);
#24108=AXIS2_PLACEMENT_3D('',#33234,#27282,#27283);
#24109=AXIS2_PLACEMENT_3D('',#33266,#27286,#27287);
#24110=AXIS2_PLACEMENT_3D('',#33273,#27288,#27289);
#24111=AXIS2_PLACEMENT_3D('',#33296,#27290,#27291);
#24112=AXIS2_PLACEMENT_3D('',#33344,#27293,#27294);
#24113=AXIS2_PLACEMENT_3D('',#33392,#27296,#27297);
#24114=AXIS2_PLACEMENT_3D('',#33440,#27299,#27300);
#24115=AXIS2_PLACEMENT_3D('',#33488,#27302,#27303);
#24116=AXIS2_PLACEMENT_3D('',#33542,#27305,#27306);
#24117=AXIS2_PLACEMENT_3D('',#33590,#27308,#27309);
#24118=AXIS2_PLACEMENT_3D('',#33638,#27311,#27312);
#24119=AXIS2_PLACEMENT_3D('',#33692,#27314,#27315);
#24120=AXIS2_PLACEMENT_3D('',#33740,#27317,#27318);
#24121=AXIS2_PLACEMENT_3D('',#33751,#27320,#27321);
#24122=AXIS2_PLACEMENT_3D('',#33756,#27322,#27323);
#24123=AXIS2_PLACEMENT_3D('',#33780,#27325,#27326);
#24124=AXIS2_PLACEMENT_3D('',#33805,#27328,#27329);
#24125=AXIS2_PLACEMENT_3D('',#33830,#27331,#27332);
#24126=AXIS2_PLACEMENT_3D('',#33854,#27334,#27335);
#24127=AXIS2_PLACEMENT_3D('',#33879,#27337,#27338);
#24128=AXIS2_PLACEMENT_3D('',#33904,#27340,#27341);
#24129=AXIS2_PLACEMENT_3D('',#33928,#27343,#27344);
#24130=AXIS2_PLACEMENT_3D('',#33954,#27346,#27347);
#24131=AXIS2_PLACEMENT_3D('',#33978,#27349,#27350);
#24132=AXIS2_PLACEMENT_3D('',#34446,#27352,#27353);
#24133=AXIS2_PLACEMENT_3D('',#34509,#27354,#27355);
#24134=AXIS2_PLACEMENT_3D('',#34510,#27356,#27357);
#24135=AXIS2_PLACEMENT_3D('',#34887,#27358,#27359);
#24136=AXIS2_PLACEMENT_3D('',#34889,#27360,#27361);
#24137=AXIS2_PLACEMENT_3D('',#34892,#27363,#27364);
#24138=AXIS2_PLACEMENT_3D('',#34893,#27365,#27366);
#24139=AXIS2_PLACEMENT_3D('',#34895,#27367,#27368);
#24140=AXIS2_PLACEMENT_3D('',#34898,#27370,#27371);
#24141=AXIS2_PLACEMENT_3D('',#34899,#27372,#27373);
#24142=AXIS2_PLACEMENT_3D('',#34901,#27374,#27375);
#24143=AXIS2_PLACEMENT_3D('',#34904,#27377,#27378);
#24144=AXIS2_PLACEMENT_3D('',#34905,#27379,#27380);
#24145=AXIS2_PLACEMENT_3D('',#34907,#27381,#27382);
#24146=AXIS2_PLACEMENT_3D('',#34910,#27384,#27385);
#24147=AXIS2_PLACEMENT_3D('',#34911,#27386,#27387);
#24148=AXIS2_PLACEMENT_3D('',#34920,#27392,#27393);
#24149=AXIS2_PLACEMENT_3D('',#34922,#27394,#27395);
#24150=AXIS2_PLACEMENT_3D('',#34924,#27397,#27398);
#24151=AXIS2_PLACEMENT_3D('',#34928,#27401,#27402);
#24152=AXIS2_PLACEMENT_3D('',#34929,#27403,#27404);
#24153=AXIS2_PLACEMENT_3D('',#34930,#27405,#27406);
#24154=AXIS2_PLACEMENT_3D('',#34939,#27411,#27412);
#24155=AXIS2_PLACEMENT_3D('',#34941,#27413,#27414);
#24156=AXIS2_PLACEMENT_3D('',#34943,#27416,#27417);
#24157=AXIS2_PLACEMENT_3D('',#34947,#27420,#27421);
#24158=AXIS2_PLACEMENT_3D('',#34948,#27422,#27423);
#24159=AXIS2_PLACEMENT_3D('',#34949,#27424,#27425);
#24160=AXIS2_PLACEMENT_3D('',#34958,#27430,#27431);
#24161=AXIS2_PLACEMENT_3D('',#34960,#27432,#27433);
#24162=AXIS2_PLACEMENT_3D('',#34962,#27435,#27436);
#24163=AXIS2_PLACEMENT_3D('',#34966,#27439,#27440);
#24164=AXIS2_PLACEMENT_3D('',#34967,#27441,#27442);
#24165=AXIS2_PLACEMENT_3D('',#34968,#27443,#27444);
#24166=AXIS2_PLACEMENT_3D('',#34977,#27449,#27450);
#24167=AXIS2_PLACEMENT_3D('',#34979,#27451,#27452);
#24168=AXIS2_PLACEMENT_3D('',#34981,#27454,#27455);
#24169=AXIS2_PLACEMENT_3D('',#34985,#27458,#27459);
#24170=AXIS2_PLACEMENT_3D('',#34986,#27460,#27461);
#24171=AXIS2_PLACEMENT_3D('',#34987,#27462,#27463);
#24172=AXIS2_PLACEMENT_3D('',#34996,#27468,#27469);
#24173=AXIS2_PLACEMENT_3D('',#34998,#27470,#27471);
#24174=AXIS2_PLACEMENT_3D('',#35000,#27473,#27474);
#24175=AXIS2_PLACEMENT_3D('',#35004,#27477,#27478);
#24176=AXIS2_PLACEMENT_3D('',#35005,#27479,#27480);
#24177=AXIS2_PLACEMENT_3D('',#35006,#27481,#27482);
#24178=AXIS2_PLACEMENT_3D('',#35015,#27487,#27488);
#24179=AXIS2_PLACEMENT_3D('',#35017,#27489,#27490);
#24180=AXIS2_PLACEMENT_3D('',#35019,#27492,#27493);
#24181=AXIS2_PLACEMENT_3D('',#35023,#27496,#27497);
#24182=AXIS2_PLACEMENT_3D('',#35024,#27498,#27499);
#24183=AXIS2_PLACEMENT_3D('',#35025,#27500,#27501);
#24184=AXIS2_PLACEMENT_3D('',#35034,#27506,#27507);
#24185=AXIS2_PLACEMENT_3D('',#35036,#27508,#27509);
#24186=AXIS2_PLACEMENT_3D('',#35038,#27511,#27512);
#24187=AXIS2_PLACEMENT_3D('',#35042,#27515,#27516);
#24188=AXIS2_PLACEMENT_3D('',#35043,#27517,#27518);
#24189=AXIS2_PLACEMENT_3D('',#35044,#27519,#27520);
#24190=AXIS2_PLACEMENT_3D('',#35053,#27525,#27526);
#24191=AXIS2_PLACEMENT_3D('',#35055,#27527,#27528);
#24192=AXIS2_PLACEMENT_3D('',#35057,#27530,#27531);
#24193=AXIS2_PLACEMENT_3D('',#35061,#27534,#27535);
#24194=AXIS2_PLACEMENT_3D('',#35062,#27536,#27537);
#24195=AXIS2_PLACEMENT_3D('',#35063,#27538,#27539);
#24196=AXIS2_PLACEMENT_3D('',#35072,#27544,#27545);
#24197=AXIS2_PLACEMENT_3D('',#35074,#27546,#27547);
#24198=AXIS2_PLACEMENT_3D('',#35076,#27549,#27550);
#24199=AXIS2_PLACEMENT_3D('',#35080,#27553,#27554);
#24200=AXIS2_PLACEMENT_3D('',#35081,#27555,#27556);
#24201=AXIS2_PLACEMENT_3D('',#35082,#27557,#27558);
#24202=AXIS2_PLACEMENT_3D('',#35091,#27563,#27564);
#24203=AXIS2_PLACEMENT_3D('',#35093,#27565,#27566);
#24204=AXIS2_PLACEMENT_3D('',#35095,#27568,#27569);
#24205=AXIS2_PLACEMENT_3D('',#35099,#27572,#27573);
#24206=AXIS2_PLACEMENT_3D('',#35100,#27574,#27575);
#24207=AXIS2_PLACEMENT_3D('',#35101,#27576,#27577);
#24208=AXIS2_PLACEMENT_3D('',#35110,#27582,#27583);
#24209=AXIS2_PLACEMENT_3D('',#35112,#27584,#27585);
#24210=AXIS2_PLACEMENT_3D('',#35114,#27587,#27588);
#24211=AXIS2_PLACEMENT_3D('',#35118,#27591,#27592);
#24212=AXIS2_PLACEMENT_3D('',#35119,#27593,#27594);
#24213=AXIS2_PLACEMENT_3D('',#35120,#27595,#27596);
#24214=AXIS2_PLACEMENT_3D('',#35129,#27601,#27602);
#24215=AXIS2_PLACEMENT_3D('',#35131,#27603,#27604);
#24216=AXIS2_PLACEMENT_3D('',#35134,#27606,#27607);
#24217=AXIS2_PLACEMENT_3D('',#35135,#27608,#27609);
#24218=AXIS2_PLACEMENT_3D('',#35139,#27612,#27613);
#24219=AXIS2_PLACEMENT_3D('',#35141,#27614,#27615);
#24220=AXIS2_PLACEMENT_3D('',#35142,#27616,#27617);
#24221=AXIS2_PLACEMENT_3D('',#35143,#27618,#27619);
#24222=AXIS2_PLACEMENT_3D('',#35152,#27624,#27625);
#24223=AXIS2_PLACEMENT_3D('',#35154,#27626,#27627);
#24224=AXIS2_PLACEMENT_3D('',#35156,#27629,#27630);
#24225=AXIS2_PLACEMENT_3D('',#35160,#27633,#27634);
#24226=AXIS2_PLACEMENT_3D('',#35161,#27635,#27636);
#24227=AXIS2_PLACEMENT_3D('',#35162,#27637,#27638);
#24228=AXIS2_PLACEMENT_3D('',#35171,#27643,#27644);
#24229=AXIS2_PLACEMENT_3D('',#35173,#27645,#27646);
#24230=AXIS2_PLACEMENT_3D('',#35175,#27648,#27649);
#24231=AXIS2_PLACEMENT_3D('',#35179,#27652,#27653);
#24232=AXIS2_PLACEMENT_3D('',#35180,#27654,#27655);
#24233=AXIS2_PLACEMENT_3D('',#35181,#27656,#27657);
#24234=AXIS2_PLACEMENT_3D('',#35190,#27662,#27663);
#24235=AXIS2_PLACEMENT_3D('',#35192,#27664,#27665);
#24236=AXIS2_PLACEMENT_3D('',#35194,#27667,#27668);
#24237=AXIS2_PLACEMENT_3D('',#35198,#27671,#27672);
#24238=AXIS2_PLACEMENT_3D('',#35199,#27673,#27674);
#24239=AXIS2_PLACEMENT_3D('',#35200,#27675,#27676);
#24240=AXIS2_PLACEMENT_3D('',#35209,#27681,#27682);
#24241=AXIS2_PLACEMENT_3D('',#35211,#27683,#27684);
#24242=AXIS2_PLACEMENT_3D('',#35213,#27686,#27687);
#24243=AXIS2_PLACEMENT_3D('',#35217,#27690,#27691);
#24244=AXIS2_PLACEMENT_3D('',#35218,#27692,#27693);
#24245=AXIS2_PLACEMENT_3D('',#35219,#27694,#27695);
#24246=AXIS2_PLACEMENT_3D('',#35228,#27700,#27701);
#24247=AXIS2_PLACEMENT_3D('',#35230,#27702,#27703);
#24248=AXIS2_PLACEMENT_3D('',#35232,#27705,#27706);
#24249=AXIS2_PLACEMENT_3D('',#35236,#27709,#27710);
#24250=AXIS2_PLACEMENT_3D('',#35237,#27711,#27712);
#24251=AXIS2_PLACEMENT_3D('',#35238,#27713,#27714);
#24252=AXIS2_PLACEMENT_3D('',#35247,#27719,#27720);
#24253=AXIS2_PLACEMENT_3D('',#35249,#27721,#27722);
#24254=AXIS2_PLACEMENT_3D('',#35251,#27724,#27725);
#24255=AXIS2_PLACEMENT_3D('',#35255,#27728,#27729);
#24256=AXIS2_PLACEMENT_3D('',#35256,#27730,#27731);
#24257=AXIS2_PLACEMENT_3D('',#35257,#27732,#27733);
#24258=AXIS2_PLACEMENT_3D('',#35266,#27738,#27739);
#24259=AXIS2_PLACEMENT_3D('',#35268,#27740,#27741);
#24260=AXIS2_PLACEMENT_3D('',#35270,#27743,#27744);
#24261=AXIS2_PLACEMENT_3D('',#35274,#27747,#27748);
#24262=AXIS2_PLACEMENT_3D('',#35275,#27749,#27750);
#24263=AXIS2_PLACEMENT_3D('',#35276,#27751,#27752);
#24264=AXIS2_PLACEMENT_3D('',#35285,#27757,#27758);
#24265=AXIS2_PLACEMENT_3D('',#35287,#27759,#27760);
#24266=AXIS2_PLACEMENT_3D('',#35289,#27762,#27763);
#24267=AXIS2_PLACEMENT_3D('',#35293,#27766,#27767);
#24268=AXIS2_PLACEMENT_3D('',#35294,#27768,#27769);
#24269=AXIS2_PLACEMENT_3D('',#35295,#27770,#27771);
#24270=AXIS2_PLACEMENT_3D('',#35304,#27776,#27777);
#24271=AXIS2_PLACEMENT_3D('',#35306,#27778,#27779);
#24272=AXIS2_PLACEMENT_3D('',#35308,#27781,#27782);
#24273=AXIS2_PLACEMENT_3D('',#35312,#27785,#27786);
#24274=AXIS2_PLACEMENT_3D('',#35313,#27787,#27788);
#24275=AXIS2_PLACEMENT_3D('',#35314,#27789,#27790);
#24276=AXIS2_PLACEMENT_3D('',#35323,#27795,#27796);
#24277=AXIS2_PLACEMENT_3D('',#35325,#27797,#27798);
#24278=AXIS2_PLACEMENT_3D('',#35327,#27800,#27801);
#24279=AXIS2_PLACEMENT_3D('',#35331,#27804,#27805);
#24280=AXIS2_PLACEMENT_3D('',#35332,#27806,#27807);
#24281=AXIS2_PLACEMENT_3D('',#35333,#27808,#27809);
#24282=AXIS2_PLACEMENT_3D('',#35342,#27814,#27815);
#24283=AXIS2_PLACEMENT_3D('',#35344,#27816,#27817);
#24284=AXIS2_PLACEMENT_3D('',#35346,#27819,#27820);
#24285=AXIS2_PLACEMENT_3D('',#35350,#27823,#27824);
#24286=AXIS2_PLACEMENT_3D('',#35351,#27825,#27826);
#24287=AXIS2_PLACEMENT_3D('',#35352,#27827,#27828);
#24288=AXIS2_PLACEMENT_3D('',#35361,#27833,#27834);
#24289=AXIS2_PLACEMENT_3D('',#35363,#27835,#27836);
#24290=AXIS2_PLACEMENT_3D('',#35365,#27838,#27839);
#24291=AXIS2_PLACEMENT_3D('',#35369,#27842,#27843);
#24292=AXIS2_PLACEMENT_3D('',#35370,#27844,#27845);
#24293=AXIS2_PLACEMENT_3D('',#35371,#27846,#27847);
#24294=AXIS2_PLACEMENT_3D('',#35373,#27848,#27849);
#24295=AXIS2_PLACEMENT_3D('',#35376,#27851,#27852);
#24296=AXIS2_PLACEMENT_3D('',#35377,#27853,#27854);
#24297=AXIS2_PLACEMENT_3D('',#35379,#27855,#27856);
#24298=AXIS2_PLACEMENT_3D('',#35381,#27858,#27859);
#24299=AXIS2_PLACEMENT_3D('',#35382,#27860,#27861);
#24300=AXIS2_PLACEMENT_3D('',#35384,#27862,#27863);
#24301=AXIS2_PLACEMENT_3D('',#35385,#27864,#27865);
#24302=AXIS2_PLACEMENT_3D('',#35388,#27867,#27868);
#24303=AXIS2_PLACEMENT_3D('',#35389,#27869,#27870);
#24304=AXIS2_PLACEMENT_3D('',#35391,#27871,#27872);
#24305=AXIS2_PLACEMENT_3D('',#35395,#27875,#27876);
#24306=AXIS2_PLACEMENT_3D('',#35396,#27877,#27878);
#24307=AXIS2_PLACEMENT_3D('',#35398,#27879,#27880);
#24308=AXIS2_PLACEMENT_3D('',#35399,#27881,#27882);
#24309=AXIS2_PLACEMENT_3D('',#35401,#27883,#27884);
#24310=AXIS2_PLACEMENT_3D('',#35403,#27886,#27887);
#24311=AXIS2_PLACEMENT_3D('',#35405,#27888,#27889);
#24312=AXIS2_PLACEMENT_3D('',#35407,#27891,#27892);
#24313=AXIS2_PLACEMENT_3D('',#35408,#27893,#27894);
#24314=AXIS2_PLACEMENT_3D('',#35417,#27899,#27900);
#24315=AXIS2_PLACEMENT_3D('',#35423,#27904,#27905);
#24316=AXIS2_PLACEMENT_3D('',#35429,#27909,#27910);
#24317=AXIS2_PLACEMENT_3D('',#35435,#27914,#27915);
#24318=AXIS2_PLACEMENT_3D('',#35441,#27919,#27920);
#24319=AXIS2_PLACEMENT_3D('',#35444,#27923,#27924);
#24320=AXIS2_PLACEMENT_3D('',#35445,#27925,#27926);
#24321=AXIS2_PLACEMENT_3D('',#35454,#27931,#27932);
#24322=AXIS2_PLACEMENT_3D('',#35455,#27933,#27934);
#24323=AXIS2_PLACEMENT_3D('',#35461,#27938,#27939);
#24324=AXIS2_PLACEMENT_3D('',#35465,#27942,#27943);
#24325=AXIS2_PLACEMENT_3D('',#35469,#27946,#27947);
#24326=AXIS2_PLACEMENT_3D('',#35471,#27949,#27950);
#24327=AXIS2_PLACEMENT_3D('',#35472,#27951,#27952);
#24328=AXIS2_PLACEMENT_3D('',#35474,#27953,#27954);
#24329=AXIS2_PLACEMENT_3D('',#35475,#27955,#27956);
#24330=AXIS2_PLACEMENT_3D('',#35477,#27958,#27959);
#24331=AXIS2_PLACEMENT_3D('',#35478,#27960,#27961);
#24332=AXIS2_PLACEMENT_3D('',#35479,#27962,#27963);
#24333=AXIS2_PLACEMENT_3D('',#35481,#27964,#27965);
#24334=AXIS2_PLACEMENT_3D('',#35485,#27967,#27968);
#24335=AXIS2_PLACEMENT_3D('',#35486,#27969,#27970);
#24336=AXIS2_PLACEMENT_3D('',#35487,#27971,#27972);
#24337=AXIS2_PLACEMENT_3D('',#35491,#27974,#27975);
#24338=AXIS2_PLACEMENT_3D('',#35492,#27976,#27977);
#24339=AXIS2_PLACEMENT_3D('',#35493,#27978,#27979);
#24340=AXIS2_PLACEMENT_3D('',#35494,#27980,#27981);
#24341=AXIS2_PLACEMENT_3D('',#35497,#27983,#27984);
#24342=AXIS2_PLACEMENT_3D('',#35498,#27985,#27986);
#24343=AXIS2_PLACEMENT_3D('',#35499,#27987,#27988);
#24344=AXIS2_PLACEMENT_3D('',#35500,#27989,#27990);
#24345=AXIS2_PLACEMENT_3D('',#35502,#27991,#27992);
#24346=AXIS2_PLACEMENT_3D('',#35505,#27994,#27995);
#24347=AXIS2_PLACEMENT_3D('',#35506,#27996,#27997);
#24348=AXIS2_PLACEMENT_3D('',#35508,#27998,#27999);
#24349=AXIS2_PLACEMENT_3D('',#35509,#28000,#28001);
#24350=AXIS2_PLACEMENT_3D('',#35511,#28002,#28003);
#24351=AXIS2_PLACEMENT_3D('',#35512,#28004,#28005);
#24352=AXIS2_PLACEMENT_3D('',#35515,#28006,#28007);
#24353=AXIS2_PLACEMENT_3D('',#35516,#28008,#28009);
#24354=AXIS2_PLACEMENT_3D('',#35518,#28011,#28012);
#24355=AXIS2_PLACEMENT_3D('',#35520,#28013,#28014);
#24356=AXIS2_PLACEMENT_3D('',#35523,#28016,#28017);
#24357=AXIS2_PLACEMENT_3D('',#35524,#28018,#28019);
#24358=AXIS2_PLACEMENT_3D('',#35526,#28020,#28021);
#24359=AXIS2_PLACEMENT_3D('',#35527,#28022,#28023);
#24360=AXIS2_PLACEMENT_3D('',#35529,#28024,#28025);
#24361=AXIS2_PLACEMENT_3D('',#35530,#28026,#28027);
#24362=AXIS2_PLACEMENT_3D('',#35532,#28029,#28030);
#24363=AXIS2_PLACEMENT_3D('',#35534,#28031,#28032);
#24364=AXIS2_PLACEMENT_3D('',#35536,#28034,#28035);
#24365=AXIS2_PLACEMENT_3D('',#35540,#28037,#28038);
#24366=AXIS2_PLACEMENT_3D('',#35541,#28039,#28040);
#24367=AXIS2_PLACEMENT_3D('',#35542,#28041,#28042);
#24368=AXIS2_PLACEMENT_3D('',#35544,#28043,#28044);
#24369=AXIS2_PLACEMENT_3D('',#35545,#28045,#28046);
#24370=AXIS2_PLACEMENT_3D('',#35548,#28048,#28049);
#24371=AXIS2_PLACEMENT_3D('',#35549,#28050,#28051);
#24372=AXIS2_PLACEMENT_3D('',#35551,#28052,#28053);
#24373=AXIS2_PLACEMENT_3D('',#35552,#28054,#28055);
#24374=AXIS2_PLACEMENT_3D('',#35554,#28057,#28058);
#24375=AXIS2_PLACEMENT_3D('',#35555,#28059,#28060);
#24376=AXIS2_PLACEMENT_3D('',#35558,#28061,#28062);
#24377=AXIS2_PLACEMENT_3D('',#35559,#28063,#28064);
#24378=AXIS2_PLACEMENT_3D('',#35563,#28066,#28067);
#24379=AXIS2_PLACEMENT_3D('',#35564,#28068,#28069);
#24380=AXIS2_PLACEMENT_3D('',#35565,#28070,#28071);
#24381=AXIS2_PLACEMENT_3D('',#35569,#28073,#28074);
#24382=AXIS2_PLACEMENT_3D('',#35570,#28075,#28076);
#24383=AXIS2_PLACEMENT_3D('',#35571,#28077,#28078);
#24384=AXIS2_PLACEMENT_3D('',#35573,#28079,#28080);
#24385=AXIS2_PLACEMENT_3D('',#35575,#28082,#28083);
#24386=AXIS2_PLACEMENT_3D('',#35578,#28085,#28086);
#24387=AXIS2_PLACEMENT_3D('',#35579,#28087,#28088);
#24388=AXIS2_PLACEMENT_3D('',#35581,#28089,#28090);
#24389=AXIS2_PLACEMENT_3D('',#35582,#28091,#28092);
#24390=AXIS2_PLACEMENT_3D('',#35591,#28097,#28098);
#24391=AXIS2_PLACEMENT_3D('',#35593,#28099,#28100);
#24392=AXIS2_PLACEMENT_3D('',#35595,#28102,#28103);
#24393=AXIS2_PLACEMENT_3D('',#35599,#28106,#28107);
#24394=AXIS2_PLACEMENT_3D('',#35600,#28108,#28109);
#24395=AXIS2_PLACEMENT_3D('',#35601,#28110,#28111);
#24396=AXIS2_PLACEMENT_3D('',#35610,#28116,#28117);
#24397=AXIS2_PLACEMENT_3D('',#35612,#28118,#28119);
#24398=AXIS2_PLACEMENT_3D('',#35614,#28121,#28122);
#24399=AXIS2_PLACEMENT_3D('',#35618,#28125,#28126);
#24400=AXIS2_PLACEMENT_3D('',#35619,#28127,#28128);
#24401=AXIS2_PLACEMENT_3D('',#35620,#28129,#28130);
#24402=AXIS2_PLACEMENT_3D('',#35629,#28135,#28136);
#24403=AXIS2_PLACEMENT_3D('',#35631,#28137,#28138);
#24404=AXIS2_PLACEMENT_3D('',#35633,#28140,#28141);
#24405=AXIS2_PLACEMENT_3D('',#35637,#28144,#28145);
#24406=AXIS2_PLACEMENT_3D('',#35638,#28146,#28147);
#24407=AXIS2_PLACEMENT_3D('',#35639,#28148,#28149);
#24408=AXIS2_PLACEMENT_3D('',#35648,#28154,#28155);
#24409=AXIS2_PLACEMENT_3D('',#35650,#28156,#28157);
#24410=AXIS2_PLACEMENT_3D('',#35652,#28159,#28160);
#24411=AXIS2_PLACEMENT_3D('',#35656,#28163,#28164);
#24412=AXIS2_PLACEMENT_3D('',#35657,#28165,#28166);
#24413=AXIS2_PLACEMENT_3D('',#35658,#28167,#28168);
#24414=AXIS2_PLACEMENT_3D('',#35667,#28173,#28174);
#24415=AXIS2_PLACEMENT_3D('',#35669,#28175,#28176);
#24416=AXIS2_PLACEMENT_3D('',#35671,#28178,#28179);
#24417=AXIS2_PLACEMENT_3D('',#35675,#28182,#28183);
#24418=AXIS2_PLACEMENT_3D('',#35676,#28184,#28185);
#24419=AXIS2_PLACEMENT_3D('',#35677,#28186,#28187);
#24420=AXIS2_PLACEMENT_3D('',#35686,#28192,#28193);
#24421=AXIS2_PLACEMENT_3D('',#35688,#28194,#28195);
#24422=AXIS2_PLACEMENT_3D('',#35690,#28197,#28198);
#24423=AXIS2_PLACEMENT_3D('',#35694,#28201,#28202);
#24424=AXIS2_PLACEMENT_3D('',#35695,#28203,#28204);
#24425=AXIS2_PLACEMENT_3D('',#35696,#28205,#28206);
#24426=AXIS2_PLACEMENT_3D('',#35705,#28211,#28212);
#24427=AXIS2_PLACEMENT_3D('',#35707,#28213,#28214);
#24428=AXIS2_PLACEMENT_3D('',#35709,#28216,#28217);
#24429=AXIS2_PLACEMENT_3D('',#35713,#28220,#28221);
#24430=AXIS2_PLACEMENT_3D('',#35714,#28222,#28223);
#24431=AXIS2_PLACEMENT_3D('',#35715,#28224,#28225);
#24432=AXIS2_PLACEMENT_3D('',#35724,#28230,#28231);
#24433=AXIS2_PLACEMENT_3D('',#35726,#28232,#28233);
#24434=AXIS2_PLACEMENT_3D('',#35728,#28235,#28236);
#24435=AXIS2_PLACEMENT_3D('',#35732,#28239,#28240);
#24436=AXIS2_PLACEMENT_3D('',#35733,#28241,#28242);
#24437=AXIS2_PLACEMENT_3D('',#35734,#28243,#28244);
#24438=AXIS2_PLACEMENT_3D('',#35743,#28249,#28250);
#24439=AXIS2_PLACEMENT_3D('',#35745,#28251,#28252);
#24440=AXIS2_PLACEMENT_3D('',#35748,#28254,#28255);
#24441=AXIS2_PLACEMENT_3D('',#35749,#28256,#28257);
#24442=AXIS2_PLACEMENT_3D('',#35753,#28260,#28261);
#24443=AXIS2_PLACEMENT_3D('',#35755,#28262,#28263);
#24444=AXIS2_PLACEMENT_3D('',#35756,#28264,#28265);
#24445=AXIS2_PLACEMENT_3D('',#35757,#28266,#28267);
#24446=AXIS2_PLACEMENT_3D('',#35766,#28272,#28273);
#24447=AXIS2_PLACEMENT_3D('',#35768,#28274,#28275);
#24448=AXIS2_PLACEMENT_3D('',#35770,#28277,#28278);
#24449=AXIS2_PLACEMENT_3D('',#35774,#28281,#28282);
#24450=AXIS2_PLACEMENT_3D('',#35775,#28283,#28284);
#24451=AXIS2_PLACEMENT_3D('',#35776,#28285,#28286);
#24452=AXIS2_PLACEMENT_3D('',#35785,#28291,#28292);
#24453=AXIS2_PLACEMENT_3D('',#35787,#28293,#28294);
#24454=AXIS2_PLACEMENT_3D('',#35789,#28296,#28297);
#24455=AXIS2_PLACEMENT_3D('',#35793,#28300,#28301);
#24456=AXIS2_PLACEMENT_3D('',#35794,#28302,#28303);
#24457=AXIS2_PLACEMENT_3D('',#35795,#28304,#28305);
#24458=AXIS2_PLACEMENT_3D('',#35804,#28310,#28311);
#24459=AXIS2_PLACEMENT_3D('',#35806,#28312,#28313);
#24460=AXIS2_PLACEMENT_3D('',#35808,#28315,#28316);
#24461=AXIS2_PLACEMENT_3D('',#35812,#28319,#28320);
#24462=AXIS2_PLACEMENT_3D('',#35813,#28321,#28322);
#24463=AXIS2_PLACEMENT_3D('',#35814,#28323,#28324);
#24464=AXIS2_PLACEMENT_3D('',#35823,#28329,#28330);
#24465=AXIS2_PLACEMENT_3D('',#35825,#28331,#28332);
#24466=AXIS2_PLACEMENT_3D('',#35827,#28334,#28335);
#24467=AXIS2_PLACEMENT_3D('',#35831,#28338,#28339);
#24468=AXIS2_PLACEMENT_3D('',#35832,#28340,#28341);
#24469=AXIS2_PLACEMENT_3D('',#35833,#28342,#28343);
#24470=AXIS2_PLACEMENT_3D('',#35842,#28348,#28349);
#24471=AXIS2_PLACEMENT_3D('',#35844,#28350,#28351);
#24472=AXIS2_PLACEMENT_3D('',#35846,#28353,#28354);
#24473=AXIS2_PLACEMENT_3D('',#35850,#28357,#28358);
#24474=AXIS2_PLACEMENT_3D('',#35851,#28359,#28360);
#24475=AXIS2_PLACEMENT_3D('',#35852,#28361,#28362);
#24476=AXIS2_PLACEMENT_3D('',#35861,#28367,#28368);
#24477=AXIS2_PLACEMENT_3D('',#35863,#28369,#28370);
#24478=AXIS2_PLACEMENT_3D('',#35865,#28372,#28373);
#24479=AXIS2_PLACEMENT_3D('',#35869,#28376,#28377);
#24480=AXIS2_PLACEMENT_3D('',#35870,#28378,#28379);
#24481=AXIS2_PLACEMENT_3D('',#35871,#28380,#28381);
#24482=AXIS2_PLACEMENT_3D('',#35880,#28386,#28387);
#24483=AXIS2_PLACEMENT_3D('',#35882,#28388,#28389);
#24484=AXIS2_PLACEMENT_3D('',#35884,#28391,#28392);
#24485=AXIS2_PLACEMENT_3D('',#35888,#28395,#28396);
#24486=AXIS2_PLACEMENT_3D('',#35889,#28397,#28398);
#24487=AXIS2_PLACEMENT_3D('',#35890,#28399,#28400);
#24488=AXIS2_PLACEMENT_3D('',#35899,#28405,#28406);
#24489=AXIS2_PLACEMENT_3D('',#35901,#28407,#28408);
#24490=AXIS2_PLACEMENT_3D('',#35903,#28410,#28411);
#24491=AXIS2_PLACEMENT_3D('',#35907,#28414,#28415);
#24492=AXIS2_PLACEMENT_3D('',#35908,#28416,#28417);
#24493=AXIS2_PLACEMENT_3D('',#35909,#28418,#28419);
#24494=AXIS2_PLACEMENT_3D('',#35918,#28424,#28425);
#24495=AXIS2_PLACEMENT_3D('',#35920,#28426,#28427);
#24496=AXIS2_PLACEMENT_3D('',#35922,#28429,#28430);
#24497=AXIS2_PLACEMENT_3D('',#35926,#28433,#28434);
#24498=AXIS2_PLACEMENT_3D('',#35927,#28435,#28436);
#24499=AXIS2_PLACEMENT_3D('',#35928,#28437,#28438);
#24500=AXIS2_PLACEMENT_3D('',#35930,#28439,#28440);
#24501=AXIS2_PLACEMENT_3D('',#35933,#28442,#28443);
#24502=AXIS2_PLACEMENT_3D('',#35934,#28444,#28445);
#24503=AXIS2_PLACEMENT_3D('',#35936,#28446,#28447);
#24504=AXIS2_PLACEMENT_3D('',#35939,#28449,#28450);
#24505=AXIS2_PLACEMENT_3D('',#35940,#28451,#28452);
#24506=AXIS2_PLACEMENT_3D('',#35941,#28453,#28454);
#24507=AXIS2_PLACEMENT_3D('',#35943,#28455,#28456);
#24508=AXIS2_PLACEMENT_3D('',#35944,#28457,#28458);
#24509=AXIS2_PLACEMENT_3D('',#35945,#28459,#28460);
#24510=AXIS2_PLACEMENT_3D('',#35947,#28461,#28462);
#24511=AXIS2_PLACEMENT_3D('',#35949,#28464,#28465);
#24512=AXIS2_PLACEMENT_3D('',#35951,#28467,#28468);
#24513=AXIS2_PLACEMENT_3D('',#35953,#28469,#28470);
#24514=AXIS2_PLACEMENT_3D('',#35954,#28471,#28472);
#24515=AXIS2_PLACEMENT_3D('',#35956,#28473,#28474);
#24516=AXIS2_PLACEMENT_3D('',#35959,#28477,#28478);
#24517=AXIS2_PLACEMENT_3D('',#35961,#28479,#28480);
#24518=AXIS2_PLACEMENT_3D('',#35962,#28481,#28482);
#24519=AXIS2_PLACEMENT_3D('',#35964,#28483,#28484);
#24520=AXIS2_PLACEMENT_3D('',#35966,#28486,#28487);
#24521=AXIS2_PLACEMENT_3D('',#35967,#28488,#28489);
#24522=AXIS2_PLACEMENT_3D('',#35968,#28490,#28491);
#24523=AXIS2_PLACEMENT_3D('',#35970,#28492,#28493);
#24524=AXIS2_PLACEMENT_3D('',#35973,#28495,#28496);
#24525=AXIS2_PLACEMENT_3D('',#35974,#28497,#28498);
#24526=AXIS2_PLACEMENT_3D('',#35976,#28499,#28500);
#24527=AXIS2_PLACEMENT_3D('',#35977,#28501,#28502);
#24528=AXIS2_PLACEMENT_3D('',#35979,#28503,#28504);
#24529=AXIS2_PLACEMENT_3D('',#35981,#28506,#28507);
#24530=AXIS2_PLACEMENT_3D('',#35982,#28508,#28509);
#24531=AXIS2_PLACEMENT_3D('',#35983,#28510,#28511);
#24532=AXIS2_PLACEMENT_3D('',#35985,#28512,#28513);
#24533=AXIS2_PLACEMENT_3D('',#35988,#28515,#28516);
#24534=AXIS2_PLACEMENT_3D('',#35989,#28517,#28518);
#24535=AXIS2_PLACEMENT_3D('',#35993,#28520,#28521);
#24536=AXIS2_PLACEMENT_3D('',#35994,#28522,#28523);
#24537=AXIS2_PLACEMENT_3D('',#35995,#28524,#28525);
#24538=AXIS2_PLACEMENT_3D('',#36000,#28527,#28528);
#24539=AXIS2_PLACEMENT_3D('',#36004,#28530,#28531);
#24540=AXIS2_PLACEMENT_3D('',#36008,#28534,#28535);
#24541=AXIS2_PLACEMENT_3D('',#36010,#28536,#28537);
#24542=AXIS2_PLACEMENT_3D('',#36012,#28539,#28540);
#24543=AXIS2_PLACEMENT_3D('',#36015,#28541,#28542);
#24544=AXIS2_PLACEMENT_3D('',#36019,#28544,#28545);
#24545=AXIS2_PLACEMENT_3D('',#36023,#28547,#28548);
#24546=AXIS2_PLACEMENT_3D('',#36027,#28550,#28551);
#24547=AXIS2_PLACEMENT_3D('',#36029,#28553,#28554);
#24548=AXIS2_PLACEMENT_3D('',#36035,#28558,#28559);
#24549=AXIS2_PLACEMENT_3D('',#36038,#28561,#28562);
#24550=AXIS2_PLACEMENT_3D('',#36039,#28563,#28564);
#24551=AXIS2_PLACEMENT_3D('',#36043,#28567,#28568);
#24552=AXIS2_PLACEMENT_3D('',#36046,#28570,#28571);
#24553=AXIS2_PLACEMENT_3D('',#36047,#28572,#28573);
#24554=AXIS2_PLACEMENT_3D('',#36051,#28576,#28577);
#24555=AXIS2_PLACEMENT_3D('',#36060,#28582,#28583);
#24556=AXIS2_PLACEMENT_3D('',#36066,#28587,#28588);
#24557=AXIS2_PLACEMENT_3D('',#36070,#28590,#28591);
#24558=AXIS2_PLACEMENT_3D('',#36071,#28592,#28593);
#24559=AXIS2_PLACEMENT_3D('',#36072,#28594,#28595);
#24560=AXIS2_PLACEMENT_3D('',#36078,#28599,#28600);
#24561=AXIS2_PLACEMENT_3D('',#36082,#28602,#28603);
#24562=AXIS2_PLACEMENT_3D('',#36083,#28604,#28605);
#24563=AXIS2_PLACEMENT_3D('',#36084,#28606,#28607);
#24564=AXIS2_PLACEMENT_3D('',#36087,#28610,#28611);
#24565=AXIS2_PLACEMENT_3D('',#36091,#28613,#28614);
#24566=AXIS2_PLACEMENT_3D('',#36093,#28616,#28617);
#24567=AXIS2_PLACEMENT_3D('',#36098,#28621,#28622);
#24568=AXIS2_PLACEMENT_3D('',#36100,#28624,#28625);
#24569=AXIS2_PLACEMENT_3D('',#36101,#28626,#28627);
#24570=AXIS2_PLACEMENT_3D('',#36105,#28629,#28630);
#24571=AXIS2_PLACEMENT_3D('',#36107,#28632,#28633);
#24572=AXIS2_PLACEMENT_3D('',#36111,#28636,#28637);
#24573=AXIS2_PLACEMENT_3D('',#36114,#28639,#28640);
#24574=AXIS2_PLACEMENT_3D('',#36115,#28641,#28642);
#24575=AXIS2_PLACEMENT_3D('',#36119,#28645,#28646);
#24576=AXIS2_PLACEMENT_3D('',#36121,#28648,#28649);
#24577=AXIS2_PLACEMENT_3D('',#36122,#28650,#28651);
#24578=AXIS2_PLACEMENT_3D('',#36124,#28653,#28654);
#24579=AXIS2_PLACEMENT_3D('',#36126,#28656,#28657);
#24580=AXIS2_PLACEMENT_3D('',#36128,#28659,#28660);
#24581=AXIS2_PLACEMENT_3D('',#36130,#28662,#28663);
#24582=AXIS2_PLACEMENT_3D('',#36132,#28665,#28666);
#24583=AXIS2_PLACEMENT_3D('',#36134,#28668,#28669);
#24584=AXIS2_PLACEMENT_3D('',#36136,#28671,#28672);
#24585=AXIS2_PLACEMENT_3D('',#36138,#28674,#28675);
#24586=AXIS2_PLACEMENT_3D('',#36139,#28676,#28677);
#24587=AXIS2_PLACEMENT_3D('',#36140,#28678,#28679);
#24588=AXIS2_PLACEMENT_3D('',#36142,#28680,#28681);
#24589=AXIS2_PLACEMENT_3D('',#36145,#28683,#28684);
#24590=AXIS2_PLACEMENT_3D('',#36146,#28685,#28686);
#24591=AXIS2_PLACEMENT_3D('',#36149,#28688,#28689);
#24592=AXIS2_PLACEMENT_3D('',#36150,#28690,#28691);
#24593=AXIS2_PLACEMENT_3D('',#36152,#28692,#28693);
#24594=AXIS2_PLACEMENT_3D('',#36154,#28695,#28696);
#24595=AXIS2_PLACEMENT_3D('',#36156,#28698,#28699);
#24596=AXIS2_PLACEMENT_3D('',#36157,#28700,#28701);
#24597=AXIS2_PLACEMENT_3D('',#36176,#28703,#28704);
#24598=AXIS2_PLACEMENT_3D('',#36179,#28706,#28707);
#24599=AXIS2_PLACEMENT_3D('',#36181,#28708,#28709);
#24600=AXIS2_PLACEMENT_3D('',#36192,#28710,#28711);
#24601=AXIS2_PLACEMENT_3D('',#36240,#28713,#28714);
#24602=AXIS2_PLACEMENT_3D('',#36294,#28716,#28717);
#24603=AXIS2_PLACEMENT_3D('',#36342,#28719,#28720);
#24604=AXIS2_PLACEMENT_3D('',#36390,#28722,#28723);
#24605=AXIS2_PLACEMENT_3D('',#36438,#28725,#28726);
#24606=AXIS2_PLACEMENT_3D('',#36492,#28728,#28729);
#24607=AXIS2_PLACEMENT_3D('',#36540,#28731,#28732);
#24608=AXIS2_PLACEMENT_3D('',#36588,#28734,#28735);
#24609=AXIS2_PLACEMENT_3D('',#36642,#28737,#28738);
#24610=AXIS2_PLACEMENT_3D('',#36690,#28740,#28741);
#24611=AXIS2_PLACEMENT_3D('',#36738,#28743,#28744);
#24612=AXIS2_PLACEMENT_3D('',#36792,#28746,#28747);
#24613=AXIS2_PLACEMENT_3D('',#36840,#28749,#28750);
#24614=AXIS2_PLACEMENT_3D('',#36852,#28752,#28753);
#24615=AXIS2_PLACEMENT_3D('',#36858,#28754,#28755);
#24616=AXIS2_PLACEMENT_3D('',#36882,#28757,#28758);
#24617=AXIS2_PLACEMENT_3D('',#36907,#28760,#28761);
#24618=AXIS2_PLACEMENT_3D('',#36932,#28763,#28764);
#24619=AXIS2_PLACEMENT_3D('',#36956,#28766,#28767);
#24620=AXIS2_PLACEMENT_3D('',#36981,#28769,#28770);
#24621=AXIS2_PLACEMENT_3D('',#37006,#28772,#28773);
#24622=AXIS2_PLACEMENT_3D('',#37030,#28775,#28776);
#24623=AXIS2_PLACEMENT_3D('',#37055,#28778,#28779);
#24624=AXIS2_PLACEMENT_3D('',#37080,#28781,#28782);
#24625=AXIS2_PLACEMENT_3D('',#37104,#28784,#28785);
#24626=AXIS2_PLACEMENT_3D('',#37128,#28787,#28788);
#24627=AXIS2_PLACEMENT_3D('',#37153,#28790,#28791);
#24628=AXIS2_PLACEMENT_3D('',#37178,#28793,#28794);
#24629=AXIS2_PLACEMENT_3D('',#37183,#28796,#28797);
#24630=AXIS2_PLACEMENT_3D('',#37712,#28798,#28799);
#24631=AXIS2_PLACEMENT_3D('',#37765,#28800,#28801);
#24632=AXIS2_PLACEMENT_3D('',#37766,#28802,#28803);
#24633=AXIS2_PLACEMENT_3D('',#38216,#28804,#28805);
#24634=AXIS2_PLACEMENT_3D('',#38217,#28806,#28807);
#24635=AXIS2_PLACEMENT_3D('',#38218,#28808,#28809);
#24636=AXIS2_PLACEMENT_3D('',#38222,#28811,#28812);
#24637=AXIS2_PLACEMENT_3D('',#38223,#28813,#28814);
#24638=AXIS2_PLACEMENT_3D('',#38232,#28819,#28820);
#24639=AXIS2_PLACEMENT_3D('',#38234,#28821,#28822);
#24640=AXIS2_PLACEMENT_3D('',#38236,#28824,#28825);
#24641=AXIS2_PLACEMENT_3D('',#38240,#28828,#28829);
#24642=AXIS2_PLACEMENT_3D('',#38241,#28830,#28831);
#24643=AXIS2_PLACEMENT_3D('',#38242,#28832,#28833);
#24644=AXIS2_PLACEMENT_3D('',#38251,#28838,#28839);
#24645=AXIS2_PLACEMENT_3D('',#38253,#28840,#28841);
#24646=AXIS2_PLACEMENT_3D('',#38255,#28843,#28844);
#24647=AXIS2_PLACEMENT_3D('',#38259,#28847,#28848);
#24648=AXIS2_PLACEMENT_3D('',#38260,#28849,#28850);
#24649=AXIS2_PLACEMENT_3D('',#38261,#28851,#28852);
#24650=AXIS2_PLACEMENT_3D('',#38270,#28857,#28858);
#24651=AXIS2_PLACEMENT_3D('',#38272,#28859,#28860);
#24652=AXIS2_PLACEMENT_3D('',#38274,#28862,#28863);
#24653=AXIS2_PLACEMENT_3D('',#38278,#28866,#28867);
#24654=AXIS2_PLACEMENT_3D('',#38279,#28868,#28869);
#24655=AXIS2_PLACEMENT_3D('',#38280,#28870,#28871);
#24656=AXIS2_PLACEMENT_3D('',#38289,#28876,#28877);
#24657=AXIS2_PLACEMENT_3D('',#38291,#28878,#28879);
#24658=AXIS2_PLACEMENT_3D('',#38293,#28881,#28882);
#24659=AXIS2_PLACEMENT_3D('',#38297,#28885,#28886);
#24660=AXIS2_PLACEMENT_3D('',#38298,#28887,#28888);
#24661=AXIS2_PLACEMENT_3D('',#38299,#28889,#28890);
#24662=AXIS2_PLACEMENT_3D('',#38308,#28895,#28896);
#24663=AXIS2_PLACEMENT_3D('',#38310,#28897,#28898);
#24664=AXIS2_PLACEMENT_3D('',#38312,#28900,#28901);
#24665=AXIS2_PLACEMENT_3D('',#38316,#28904,#28905);
#24666=AXIS2_PLACEMENT_3D('',#38317,#28906,#28907);
#24667=AXIS2_PLACEMENT_3D('',#38318,#28908,#28909);
#24668=AXIS2_PLACEMENT_3D('',#38327,#28914,#28915);
#24669=AXIS2_PLACEMENT_3D('',#38329,#28916,#28917);
#24670=AXIS2_PLACEMENT_3D('',#38331,#28919,#28920);
#24671=AXIS2_PLACEMENT_3D('',#38335,#28923,#28924);
#24672=AXIS2_PLACEMENT_3D('',#38336,#28925,#28926);
#24673=AXIS2_PLACEMENT_3D('',#38337,#28927,#28928);
#24674=AXIS2_PLACEMENT_3D('',#38346,#28933,#28934);
#24675=AXIS2_PLACEMENT_3D('',#38348,#28935,#28936);
#24676=AXIS2_PLACEMENT_3D('',#38350,#28938,#28939);
#24677=AXIS2_PLACEMENT_3D('',#38354,#28942,#28943);
#24678=AXIS2_PLACEMENT_3D('',#38355,#28944,#28945);
#24679=AXIS2_PLACEMENT_3D('',#38356,#28946,#28947);
#24680=AXIS2_PLACEMENT_3D('',#38365,#28952,#28953);
#24681=AXIS2_PLACEMENT_3D('',#38367,#28954,#28955);
#24682=AXIS2_PLACEMENT_3D('',#38369,#28957,#28958);
#24683=AXIS2_PLACEMENT_3D('',#38373,#28961,#28962);
#24684=AXIS2_PLACEMENT_3D('',#38374,#28963,#28964);
#24685=AXIS2_PLACEMENT_3D('',#38375,#28965,#28966);
#24686=AXIS2_PLACEMENT_3D('',#38384,#28971,#28972);
#24687=AXIS2_PLACEMENT_3D('',#38386,#28973,#28974);
#24688=AXIS2_PLACEMENT_3D('',#38388,#28976,#28977);
#24689=AXIS2_PLACEMENT_3D('',#38392,#28980,#28981);
#24690=AXIS2_PLACEMENT_3D('',#38393,#28982,#28983);
#24691=AXIS2_PLACEMENT_3D('',#38394,#28984,#28985);
#24692=AXIS2_PLACEMENT_3D('',#38403,#28990,#28991);
#24693=AXIS2_PLACEMENT_3D('',#38405,#28992,#28993);
#24694=AXIS2_PLACEMENT_3D('',#38407,#28995,#28996);
#24695=AXIS2_PLACEMENT_3D('',#38411,#28999,#29000);
#24696=AXIS2_PLACEMENT_3D('',#38412,#29001,#29002);
#24697=AXIS2_PLACEMENT_3D('',#38413,#29003,#29004);
#24698=AXIS2_PLACEMENT_3D('',#38422,#29009,#29010);
#24699=AXIS2_PLACEMENT_3D('',#38424,#29011,#29012);
#24700=AXIS2_PLACEMENT_3D('',#38426,#29014,#29015);
#24701=AXIS2_PLACEMENT_3D('',#38430,#29018,#29019);
#24702=AXIS2_PLACEMENT_3D('',#38431,#29020,#29021);
#24703=AXIS2_PLACEMENT_3D('',#38432,#29022,#29023);
#24704=AXIS2_PLACEMENT_3D('',#38441,#29028,#29029);
#24705=AXIS2_PLACEMENT_3D('',#38443,#29030,#29031);
#24706=AXIS2_PLACEMENT_3D('',#38446,#29033,#29034);
#24707=AXIS2_PLACEMENT_3D('',#38447,#29035,#29036);
#24708=AXIS2_PLACEMENT_3D('',#38451,#29039,#29040);
#24709=AXIS2_PLACEMENT_3D('',#38453,#29041,#29042);
#24710=AXIS2_PLACEMENT_3D('',#38454,#29043,#29044);
#24711=AXIS2_PLACEMENT_3D('',#38455,#29045,#29046);
#24712=AXIS2_PLACEMENT_3D('',#38464,#29051,#29052);
#24713=AXIS2_PLACEMENT_3D('',#38466,#29053,#29054);
#24714=AXIS2_PLACEMENT_3D('',#38468,#29056,#29057);
#24715=AXIS2_PLACEMENT_3D('',#38472,#29060,#29061);
#24716=AXIS2_PLACEMENT_3D('',#38473,#29062,#29063);
#24717=AXIS2_PLACEMENT_3D('',#38474,#29064,#29065);
#24718=AXIS2_PLACEMENT_3D('',#38483,#29070,#29071);
#24719=AXIS2_PLACEMENT_3D('',#38485,#29072,#29073);
#24720=AXIS2_PLACEMENT_3D('',#38487,#29075,#29076);
#24721=AXIS2_PLACEMENT_3D('',#38491,#29079,#29080);
#24722=AXIS2_PLACEMENT_3D('',#38492,#29081,#29082);
#24723=AXIS2_PLACEMENT_3D('',#38493,#29083,#29084);
#24724=AXIS2_PLACEMENT_3D('',#38502,#29089,#29090);
#24725=AXIS2_PLACEMENT_3D('',#38504,#29091,#29092);
#24726=AXIS2_PLACEMENT_3D('',#38506,#29094,#29095);
#24727=AXIS2_PLACEMENT_3D('',#38510,#29098,#29099);
#24728=AXIS2_PLACEMENT_3D('',#38511,#29100,#29101);
#24729=AXIS2_PLACEMENT_3D('',#38512,#29102,#29103);
#24730=AXIS2_PLACEMENT_3D('',#38521,#29108,#29109);
#24731=AXIS2_PLACEMENT_3D('',#38523,#29110,#29111);
#24732=AXIS2_PLACEMENT_3D('',#38525,#29113,#29114);
#24733=AXIS2_PLACEMENT_3D('',#38529,#29117,#29118);
#24734=AXIS2_PLACEMENT_3D('',#38530,#29119,#29120);
#24735=AXIS2_PLACEMENT_3D('',#38531,#29121,#29122);
#24736=AXIS2_PLACEMENT_3D('',#38540,#29127,#29128);
#24737=AXIS2_PLACEMENT_3D('',#38542,#29129,#29130);
#24738=AXIS2_PLACEMENT_3D('',#38544,#29132,#29133);
#24739=AXIS2_PLACEMENT_3D('',#38548,#29136,#29137);
#24740=AXIS2_PLACEMENT_3D('',#38549,#29138,#29139);
#24741=AXIS2_PLACEMENT_3D('',#38550,#29140,#29141);
#24742=AXIS2_PLACEMENT_3D('',#38559,#29146,#29147);
#24743=AXIS2_PLACEMENT_3D('',#38561,#29148,#29149);
#24744=AXIS2_PLACEMENT_3D('',#38563,#29151,#29152);
#24745=AXIS2_PLACEMENT_3D('',#38567,#29155,#29156);
#24746=AXIS2_PLACEMENT_3D('',#38568,#29157,#29158);
#24747=AXIS2_PLACEMENT_3D('',#38569,#29159,#29160);
#24748=AXIS2_PLACEMENT_3D('',#38578,#29165,#29166);
#24749=AXIS2_PLACEMENT_3D('',#38580,#29167,#29168);
#24750=AXIS2_PLACEMENT_3D('',#38582,#29170,#29171);
#24751=AXIS2_PLACEMENT_3D('',#38586,#29174,#29175);
#24752=AXIS2_PLACEMENT_3D('',#38587,#29176,#29177);
#24753=AXIS2_PLACEMENT_3D('',#38588,#29178,#29179);
#24754=AXIS2_PLACEMENT_3D('',#38597,#29184,#29185);
#24755=AXIS2_PLACEMENT_3D('',#38599,#29186,#29187);
#24756=AXIS2_PLACEMENT_3D('',#38601,#29189,#29190);
#24757=AXIS2_PLACEMENT_3D('',#38605,#29193,#29194);
#24758=AXIS2_PLACEMENT_3D('',#38606,#29195,#29196);
#24759=AXIS2_PLACEMENT_3D('',#38607,#29197,#29198);
#24760=AXIS2_PLACEMENT_3D('',#38616,#29203,#29204);
#24761=AXIS2_PLACEMENT_3D('',#38618,#29205,#29206);
#24762=AXIS2_PLACEMENT_3D('',#38620,#29208,#29209);
#24763=AXIS2_PLACEMENT_3D('',#38624,#29212,#29213);
#24764=AXIS2_PLACEMENT_3D('',#38625,#29214,#29215);
#24765=AXIS2_PLACEMENT_3D('',#38626,#29216,#29217);
#24766=AXIS2_PLACEMENT_3D('',#38635,#29222,#29223);
#24767=AXIS2_PLACEMENT_3D('',#38637,#29224,#29225);
#24768=AXIS2_PLACEMENT_3D('',#38639,#29227,#29228);
#24769=AXIS2_PLACEMENT_3D('',#38643,#29231,#29232);
#24770=AXIS2_PLACEMENT_3D('',#38644,#29233,#29234);
#24771=AXIS2_PLACEMENT_3D('',#38645,#29235,#29236);
#24772=AXIS2_PLACEMENT_3D('',#38654,#29241,#29242);
#24773=AXIS2_PLACEMENT_3D('',#38656,#29243,#29244);
#24774=AXIS2_PLACEMENT_3D('',#38658,#29246,#29247);
#24775=AXIS2_PLACEMENT_3D('',#38662,#29250,#29251);
#24776=AXIS2_PLACEMENT_3D('',#38663,#29252,#29253);
#24777=AXIS2_PLACEMENT_3D('',#38664,#29254,#29255);
#24778=AXIS2_PLACEMENT_3D('',#38673,#29260,#29261);
#24779=AXIS2_PLACEMENT_3D('',#38675,#29262,#29263);
#24780=AXIS2_PLACEMENT_3D('',#38677,#29265,#29266);
#24781=AXIS2_PLACEMENT_3D('',#38681,#29269,#29270);
#24782=AXIS2_PLACEMENT_3D('',#38682,#29271,#29272);
#24783=AXIS2_PLACEMENT_3D('',#38683,#29273,#29274);
#24784=AXIS2_PLACEMENT_3D('',#38685,#29275,#29276);
#24785=AXIS2_PLACEMENT_3D('',#38686,#29277,#29278);
#24786=AXIS2_PLACEMENT_3D('',#38688,#29280,#29281);
#24787=AXIS2_PLACEMENT_3D('',#38690,#29282,#29283);
#24788=AXIS2_PLACEMENT_3D('',#38691,#29284,#29285);
#24789=AXIS2_PLACEMENT_3D('',#38693,#29286,#29287);
#24790=AXIS2_PLACEMENT_3D('',#38695,#29289,#29290);
#24791=AXIS2_PLACEMENT_3D('',#38697,#29291,#29292);
#24792=AXIS2_PLACEMENT_3D('',#38700,#29295,#29296);
#24793=AXIS2_PLACEMENT_3D('',#38702,#29297,#29298);
#24794=AXIS2_PLACEMENT_3D('',#38704,#29300,#29301);
#24795=AXIS2_PLACEMENT_3D('',#38705,#29302,#29303);
#24796=AXIS2_PLACEMENT_3D('',#38706,#29304,#29305);
#24797=AXIS2_PLACEMENT_3D('',#38728,#29307,#29308);
#24798=AXIS2_PLACEMENT_3D('',#38731,#29310,#29311);
#24799=AXIS2_PLACEMENT_3D('',#38733,#29312,#29313);
#24800=AXIS2_PLACEMENT_3D('',#38747,#29314,#29315);
#24801=AXIS2_PLACEMENT_3D('',#38801,#29317,#29318);
#24802=AXIS2_PLACEMENT_3D('',#38849,#29320,#29321);
#24803=AXIS2_PLACEMENT_3D('',#38897,#29323,#29324);
#24804=AXIS2_PLACEMENT_3D('',#38951,#29326,#29327);
#24805=AXIS2_PLACEMENT_3D('',#38999,#29329,#29330);
#24806=AXIS2_PLACEMENT_3D('',#39047,#29332,#29333);
#24807=AXIS2_PLACEMENT_3D('',#39101,#29335,#29336);
#24808=AXIS2_PLACEMENT_3D('',#39149,#29338,#29339);
#24809=AXIS2_PLACEMENT_3D('',#39197,#29341,#29342);
#24810=AXIS2_PLACEMENT_3D('',#39251,#29344,#29345);
#24811=AXIS2_PLACEMENT_3D('',#39299,#29347,#29348);
#24812=AXIS2_PLACEMENT_3D('',#39347,#29350,#29351);
#24813=AXIS2_PLACEMENT_3D('',#39401,#29353,#29354);
#24814=AXIS2_PLACEMENT_3D('',#39413,#29356,#29357);
#24815=AXIS2_PLACEMENT_3D('',#39419,#29358,#29359);
#24816=AXIS2_PLACEMENT_3D('',#39444,#29361,#29362);
#24817=AXIS2_PLACEMENT_3D('',#39469,#29364,#29365);
#24818=AXIS2_PLACEMENT_3D('',#39493,#29367,#29368);
#24819=AXIS2_PLACEMENT_3D('',#39518,#29370,#29371);
#24820=AXIS2_PLACEMENT_3D('',#39543,#29373,#29374);
#24821=AXIS2_PLACEMENT_3D('',#39567,#29376,#29377);
#24822=AXIS2_PLACEMENT_3D('',#39592,#29379,#29380);
#24823=AXIS2_PLACEMENT_3D('',#39617,#29382,#29383);
#24824=AXIS2_PLACEMENT_3D('',#39641,#29385,#29386);
#24825=AXIS2_PLACEMENT_3D('',#39666,#29388,#29389);
#24826=AXIS2_PLACEMENT_3D('',#39691,#29391,#29392);
#24827=AXIS2_PLACEMENT_3D('',#39715,#29394,#29395);
#24828=AXIS2_PLACEMENT_3D('',#39740,#29397,#29398);
#24829=AXIS2_PLACEMENT_3D('',#39765,#29400,#29401);
#24830=AXIS2_PLACEMENT_3D('',#39820,#29402,#29403);
#24831=AXIS2_PLACEMENT_3D('',#39822,#29404,#29405);
#24832=AXIS2_PLACEMENT_3D('',#40340,#29406,#29407);
#24833=AXIS2_PLACEMENT_3D('',#40394,#29408,#29409);
#24834=AXIS2_PLACEMENT_3D('',#40395,#29410,#29411);
#24835=AXIS2_PLACEMENT_3D('',#40804,#29412,#29413);
#24836=AXIS2_PLACEMENT_3D('',#40807,#29414,#29415);
#24837=AXIS2_PLACEMENT_3D('',#40811,#29418,#29419);
#24838=AXIS2_PLACEMENT_3D('',#40819,#29422,#29423);
#24839=AXIS2_PLACEMENT_3D('',#40825,#29425,#29426);
#24840=AXIS2_PLACEMENT_3D('',#40828,#29427,#29428);
#24841=AXIS2_PLACEMENT_3D('',#40832,#29431,#29432);
#24842=AXIS2_PLACEMENT_3D('',#40840,#29435,#29436);
#24843=AXIS2_PLACEMENT_3D('',#40846,#29438,#29439);
#24844=AXIS2_PLACEMENT_3D('',#40849,#29440,#29441);
#24845=AXIS2_PLACEMENT_3D('',#40853,#29444,#29445);
#24846=AXIS2_PLACEMENT_3D('',#40861,#29448,#29449);
#24847=AXIS2_PLACEMENT_3D('',#40867,#29451,#29452);
#24848=AXIS2_PLACEMENT_3D('',#40870,#29453,#29454);
#24849=AXIS2_PLACEMENT_3D('',#40874,#29457,#29458);
#24850=AXIS2_PLACEMENT_3D('',#40882,#29461,#29462);
#24851=AXIS2_PLACEMENT_3D('',#40888,#29464,#29465);
#24852=AXIS2_PLACEMENT_3D('',#40891,#29466,#29467);
#24853=AXIS2_PLACEMENT_3D('',#40895,#29470,#29471);
#24854=AXIS2_PLACEMENT_3D('',#40903,#29474,#29475);
#24855=AXIS2_PLACEMENT_3D('',#40909,#29477,#29478);
#24856=AXIS2_PLACEMENT_3D('',#40912,#29479,#29480);
#24857=AXIS2_PLACEMENT_3D('',#40916,#29483,#29484);
#24858=AXIS2_PLACEMENT_3D('',#40924,#29487,#29488);
#24859=AXIS2_PLACEMENT_3D('',#40930,#29490,#29491);
#24860=AXIS2_PLACEMENT_3D('',#40933,#29492,#29493);
#24861=AXIS2_PLACEMENT_3D('',#40937,#29496,#29497);
#24862=AXIS2_PLACEMENT_3D('',#40945,#29500,#29501);
#24863=AXIS2_PLACEMENT_3D('',#40951,#29503,#29504);
#24864=AXIS2_PLACEMENT_3D('',#40954,#29505,#29506);
#24865=AXIS2_PLACEMENT_3D('',#40958,#29509,#29510);
#24866=AXIS2_PLACEMENT_3D('',#40966,#29513,#29514);
#24867=AXIS2_PLACEMENT_3D('',#40972,#29516,#29517);
#24868=AXIS2_PLACEMENT_3D('',#40975,#29518,#29519);
#24869=AXIS2_PLACEMENT_3D('',#40979,#29522,#29523);
#24870=AXIS2_PLACEMENT_3D('',#40987,#29526,#29527);
#24871=AXIS2_PLACEMENT_3D('',#40993,#29529,#29530);
#24872=AXIS2_PLACEMENT_3D('',#40996,#29531,#29532);
#24873=AXIS2_PLACEMENT_3D('',#41000,#29535,#29536);
#24874=AXIS2_PLACEMENT_3D('',#41008,#29539,#29540);
#24875=AXIS2_PLACEMENT_3D('',#41014,#29542,#29543);
#24876=AXIS2_PLACEMENT_3D('',#41017,#29544,#29545);
#24877=AXIS2_PLACEMENT_3D('',#41021,#29548,#29549);
#24878=AXIS2_PLACEMENT_3D('',#41029,#29552,#29553);
#24879=AXIS2_PLACEMENT_3D('',#41035,#29555,#29556);
#24880=AXIS2_PLACEMENT_3D('',#41038,#29557,#29558);
#24881=AXIS2_PLACEMENT_3D('',#41042,#29561,#29562);
#24882=AXIS2_PLACEMENT_3D('',#41050,#29565,#29566);
#24883=AXIS2_PLACEMENT_3D('',#41056,#29568,#29569);
#24884=AXIS2_PLACEMENT_3D('',#41059,#29570,#29571);
#24885=AXIS2_PLACEMENT_3D('',#41063,#29574,#29575);
#24886=AXIS2_PLACEMENT_3D('',#41071,#29578,#29579);
#24887=AXIS2_PLACEMENT_3D('',#41077,#29581,#29582);
#24888=AXIS2_PLACEMENT_3D('',#41080,#29583,#29584);
#24889=AXIS2_PLACEMENT_3D('',#41084,#29587,#29588);
#24890=AXIS2_PLACEMENT_3D('',#41092,#29591,#29592);
#24891=AXIS2_PLACEMENT_3D('',#41098,#29594,#29595);
#24892=AXIS2_PLACEMENT_3D('',#41101,#29596,#29597);
#24893=AXIS2_PLACEMENT_3D('',#41105,#29600,#29601);
#24894=AXIS2_PLACEMENT_3D('',#41113,#29604,#29605);
#24895=AXIS2_PLACEMENT_3D('',#41119,#29607,#29608);
#24896=AXIS2_PLACEMENT_3D('',#41122,#29609,#29610);
#24897=AXIS2_PLACEMENT_3D('',#41126,#29613,#29614);
#24898=AXIS2_PLACEMENT_3D('',#41134,#29617,#29618);
#24899=AXIS2_PLACEMENT_3D('',#41140,#29620,#29621);
#24900=AXIS2_PLACEMENT_3D('',#41143,#29622,#29623);
#24901=AXIS2_PLACEMENT_3D('',#41147,#29626,#29627);
#24902=AXIS2_PLACEMENT_3D('',#41155,#29630,#29631);
#24903=AXIS2_PLACEMENT_3D('',#41161,#29633,#29634);
#24904=AXIS2_PLACEMENT_3D('',#41164,#29635,#29636);
#24905=AXIS2_PLACEMENT_3D('',#41169,#29639,#29640);
#24906=AXIS2_PLACEMENT_3D('',#41170,#29641,#29642);
#24907=AXIS2_PLACEMENT_3D('',#41178,#29645,#29646);
#24908=AXIS2_PLACEMENT_3D('',#41184,#29648,#29649);
#24909=AXIS2_PLACEMENT_3D('',#41187,#29650,#29651);
#24910=AXIS2_PLACEMENT_3D('',#41191,#29654,#29655);
#24911=AXIS2_PLACEMENT_3D('',#41199,#29658,#29659);
#24912=AXIS2_PLACEMENT_3D('',#41205,#29661,#29662);
#24913=AXIS2_PLACEMENT_3D('',#41208,#29663,#29664);
#24914=AXIS2_PLACEMENT_3D('',#41212,#29667,#29668);
#24915=AXIS2_PLACEMENT_3D('',#41220,#29671,#29672);
#24916=AXIS2_PLACEMENT_3D('',#41226,#29674,#29675);
#24917=AXIS2_PLACEMENT_3D('',#41229,#29676,#29677);
#24918=AXIS2_PLACEMENT_3D('',#41233,#29680,#29681);
#24919=AXIS2_PLACEMENT_3D('',#41241,#29684,#29685);
#24920=AXIS2_PLACEMENT_3D('',#41247,#29687,#29688);
#24921=AXIS2_PLACEMENT_3D('',#41250,#29689,#29690);
#24922=AXIS2_PLACEMENT_3D('',#41254,#29693,#29694);
#24923=AXIS2_PLACEMENT_3D('',#41262,#29697,#29698);
#24924=AXIS2_PLACEMENT_3D('',#41268,#29700,#29701);
#24925=AXIS2_PLACEMENT_3D('',#41271,#29702,#29703);
#24926=AXIS2_PLACEMENT_3D('',#41275,#29706,#29707);
#24927=AXIS2_PLACEMENT_3D('',#41283,#29710,#29711);
#24928=AXIS2_PLACEMENT_3D('',#41289,#29713,#29714);
#24929=AXIS2_PLACEMENT_3D('',#41292,#29715,#29716);
#24930=AXIS2_PLACEMENT_3D('',#41296,#29719,#29720);
#24931=AXIS2_PLACEMENT_3D('',#41304,#29723,#29724);
#24932=AXIS2_PLACEMENT_3D('',#41310,#29726,#29727);
#24933=AXIS2_PLACEMENT_3D('',#41313,#29728,#29729);
#24934=AXIS2_PLACEMENT_3D('',#41317,#29732,#29733);
#24935=AXIS2_PLACEMENT_3D('',#41325,#29736,#29737);
#24936=AXIS2_PLACEMENT_3D('',#41331,#29739,#29740);
#24937=AXIS2_PLACEMENT_3D('',#41334,#29741,#29742);
#24938=AXIS2_PLACEMENT_3D('',#41338,#29745,#29746);
#24939=AXIS2_PLACEMENT_3D('',#41346,#29749,#29750);
#24940=AXIS2_PLACEMENT_3D('',#41352,#29752,#29753);
#24941=AXIS2_PLACEMENT_3D('',#41355,#29754,#29755);
#24942=AXIS2_PLACEMENT_3D('',#41359,#29758,#29759);
#24943=AXIS2_PLACEMENT_3D('',#41367,#29762,#29763);
#24944=AXIS2_PLACEMENT_3D('',#41373,#29765,#29766);
#24945=AXIS2_PLACEMENT_3D('',#41376,#29767,#29768);
#24946=AXIS2_PLACEMENT_3D('',#41380,#29771,#29772);
#24947=AXIS2_PLACEMENT_3D('',#41388,#29775,#29776);
#24948=AXIS2_PLACEMENT_3D('',#41394,#29778,#29779);
#24949=AXIS2_PLACEMENT_3D('',#41397,#29780,#29781);
#24950=AXIS2_PLACEMENT_3D('',#41401,#29784,#29785);
#24951=AXIS2_PLACEMENT_3D('',#41409,#29788,#29789);
#24952=AXIS2_PLACEMENT_3D('',#41415,#29791,#29792);
#24953=AXIS2_PLACEMENT_3D('',#41418,#29793,#29794);
#24954=AXIS2_PLACEMENT_3D('',#41422,#29797,#29798);
#24955=AXIS2_PLACEMENT_3D('',#41430,#29801,#29802);
#24956=AXIS2_PLACEMENT_3D('',#41436,#29804,#29805);
#24957=AXIS2_PLACEMENT_3D('',#41439,#29806,#29807);
#24958=AXIS2_PLACEMENT_3D('',#41443,#29810,#29811);
#24959=AXIS2_PLACEMENT_3D('',#41451,#29814,#29815);
#24960=AXIS2_PLACEMENT_3D('',#41457,#29817,#29818);
#24961=AXIS2_PLACEMENT_3D('',#41460,#29819,#29820);
#24962=AXIS2_PLACEMENT_3D('',#41464,#29823,#29824);
#24963=AXIS2_PLACEMENT_3D('',#41472,#29827,#29828);
#24964=AXIS2_PLACEMENT_3D('',#41478,#29830,#29831);
#24965=AXIS2_PLACEMENT_3D('',#41481,#29832,#29833);
#24966=AXIS2_PLACEMENT_3D('',#41485,#29836,#29837);
#24967=AXIS2_PLACEMENT_3D('',#41493,#29840,#29841);
#24968=AXIS2_PLACEMENT_3D('',#41499,#29843,#29844);
#24969=AXIS2_PLACEMENT_3D('',#41502,#29845,#29846);
#24970=AXIS2_PLACEMENT_3D('',#41506,#29849,#29850);
#24971=AXIS2_PLACEMENT_3D('',#41514,#29853,#29854);
#24972=AXIS2_PLACEMENT_3D('',#41520,#29856,#29857);
#24973=AXIS2_PLACEMENT_3D('',#41523,#29858,#29859);
#24974=AXIS2_PLACEMENT_3D('',#41527,#29862,#29863);
#24975=AXIS2_PLACEMENT_3D('',#41535,#29866,#29867);
#24976=AXIS2_PLACEMENT_3D('',#41541,#29869,#29870);
#24977=AXIS2_PLACEMENT_3D('',#41542,#29871,#29872);
#24978=AXIS2_PLACEMENT_3D('',#41543,#29873,#29874);
#24979=AXIS2_PLACEMENT_3D('',#41544,#29875,#29876);
#24980=AXIS2_PLACEMENT_3D('',#41545,#29877,#29878);
#24981=AXIS2_PLACEMENT_3D('',#41546,#29879,#29880);
#24982=AXIS2_PLACEMENT_3D('',#41547,#29881,#29882);
#24983=AXIS2_PLACEMENT_3D('',#41548,#29883,#29884);
#24984=AXIS2_PLACEMENT_3D('',#41549,#29885,#29886);
#24985=AXIS2_PLACEMENT_3D('',#41550,#29887,#29888);
#24986=AXIS2_PLACEMENT_3D('',#41551,#29889,#29890);
#24987=AXIS2_PLACEMENT_3D('',#41552,#29891,#29892);
#24988=AXIS2_PLACEMENT_3D('',#41553,#29893,#29894);
#24989=AXIS2_PLACEMENT_3D('',#41554,#29895,#29896);
#24990=AXIS2_PLACEMENT_3D('',#41555,#29897,#29898);
#24991=AXIS2_PLACEMENT_3D('',#41556,#29899,#29900);
#24992=AXIS2_PLACEMENT_3D('',#41557,#29901,#29902);
#24993=AXIS2_PLACEMENT_3D('',#41558,#29903,#29904);
#24994=AXIS2_PLACEMENT_3D('',#41561,#29906,#29907);
#24995=AXIS2_PLACEMENT_3D('',#41562,#29908,#29909);
#24996=AXIS2_PLACEMENT_3D('',#41563,#29910,#29911);
#24997=AXIS2_PLACEMENT_3D('',#41564,#29912,#29913);
#24998=AXIS2_PLACEMENT_3D('',#41565,#29914,#29915);
#24999=AXIS2_PLACEMENT_3D('',#41566,#29916,#29917);
#25000=AXIS2_PLACEMENT_3D('',#41567,#29918,#29919);
#25001=AXIS2_PLACEMENT_3D('',#41568,#29920,#29921);
#25002=AXIS2_PLACEMENT_3D('',#41569,#29922,#29923);
#25003=AXIS2_PLACEMENT_3D('',#41570,#29924,#29925);
#25004=AXIS2_PLACEMENT_3D('',#41571,#29926,#29927);
#25005=AXIS2_PLACEMENT_3D('',#41572,#29928,#29929);
#25006=AXIS2_PLACEMENT_3D('',#41573,#29930,#29931);
#25007=AXIS2_PLACEMENT_3D('',#41574,#29932,#29933);
#25008=AXIS2_PLACEMENT_3D('',#41575,#29934,#29935);
#25009=AXIS2_PLACEMENT_3D('',#41576,#29936,#29937);
#25010=AXIS2_PLACEMENT_3D('',#41577,#29938,#29939);
#25011=AXIS2_PLACEMENT_3D('',#41578,#29940,#29941);
#25012=AXIS2_PLACEMENT_3D('',#41580,#29942,#29943);
#25013=AXIS2_PLACEMENT_3D('',#41584,#29945,#29946);
#25014=AXIS2_PLACEMENT_3D('',#41587,#29948,#29949);
#25015=AXIS2_PLACEMENT_3D('',#41588,#29950,#29951);
#25016=AXIS2_PLACEMENT_3D('',#41596,#29954,#29955);
#25017=AXIS2_PLACEMENT_3D('',#41601,#29957,#29958);
#25018=AXIS2_PLACEMENT_3D('',#41602,#29959,#29960);
#25019=AXIS2_PLACEMENT_3D('',#41604,#29961,#29962);
#25020=AXIS2_PLACEMENT_3D('',#41606,#29964,#29965);
#25021=AXIS2_PLACEMENT_3D('',#41610,#29967,#29968);
#25022=AXIS2_PLACEMENT_3D('',#41611,#29969,#29970);
#25023=AXIS2_PLACEMENT_3D('',#41620,#29975,#29976);
#25024=AXIS2_PLACEMENT_3D('',#41626,#29980,#29981);
#25025=AXIS2_PLACEMENT_3D('',#41632,#29985,#29986);
#25026=AXIS2_PLACEMENT_3D('',#41638,#29990,#29991);
#25027=AXIS2_PLACEMENT_3D('',#41644,#29995,#29996);
#25028=AXIS2_PLACEMENT_3D('',#41647,#29999,#30000);
#25029=AXIS2_PLACEMENT_3D('',#41648,#30001,#30002);
#25030=AXIS2_PLACEMENT_3D('',#41650,#30003,#30004);
#25031=AXIS2_PLACEMENT_3D('',#41651,#30005,#30006);
#25032=AXIS2_PLACEMENT_3D('',#41653,#30008,#30009);
#25033=AXIS2_PLACEMENT_3D('',#41654,#30010,#30011);
#25034=AXIS2_PLACEMENT_3D('',#41655,#30012,#30013);
#25035=AXIS2_PLACEMENT_3D('',#41657,#30014,#30015);
#25036=AXIS2_PLACEMENT_3D('',#41659,#30017,#30018);
#25037=AXIS2_PLACEMENT_3D('',#41660,#30019,#30020);
#25038=AXIS2_PLACEMENT_3D('',#41661,#30021,#30022);
#25039=AXIS2_PLACEMENT_3D('',#41662,#30023,#30024);
#25040=AXIS2_PLACEMENT_3D('',#41684,#30026,#30027);
#25041=AXIS2_PLACEMENT_3D('',#41687,#30029,#30030);
#25042=AXIS2_PLACEMENT_3D('',#41689,#30031,#30032);
#25043=AXIS2_PLACEMENT_3D('',#41703,#30033,#30034);
#25044=AXIS2_PLACEMENT_3D('',#41751,#30036,#30037);
#25045=AXIS2_PLACEMENT_3D('',#41805,#30039,#30040);
#25046=AXIS2_PLACEMENT_3D('',#41853,#30042,#30043);
#25047=AXIS2_PLACEMENT_3D('',#41901,#30045,#30046);
#25048=AXIS2_PLACEMENT_3D('',#41955,#30048,#30049);
#25049=AXIS2_PLACEMENT_3D('',#42003,#30051,#30052);
#25050=AXIS2_PLACEMENT_3D('',#42051,#30054,#30055);
#25051=AXIS2_PLACEMENT_3D('',#42099,#30057,#30058);
#25052=AXIS2_PLACEMENT_3D('',#42153,#30060,#30061);
#25053=AXIS2_PLACEMENT_3D('',#42201,#30063,#30064);
#25054=AXIS2_PLACEMENT_3D('',#42249,#30066,#30067);
#25055=AXIS2_PLACEMENT_3D('',#42303,#30069,#30070);
#25056=AXIS2_PLACEMENT_3D('',#42351,#30072,#30073);
#25057=AXIS2_PLACEMENT_3D('',#42399,#30075,#30076);
#25058=AXIS2_PLACEMENT_3D('',#42450,#30078,#30079);
#25059=AXIS2_PLACEMENT_3D('',#42501,#30081,#30082);
#25060=AXIS2_PLACEMENT_3D('',#42549,#30084,#30085);
#25061=AXIS2_PLACEMENT_3D('',#42597,#30087,#30088);
#25062=AXIS2_PLACEMENT_3D('',#42651,#30090,#30091);
#25063=AXIS2_PLACEMENT_3D('',#42699,#30093,#30094);
#25064=AXIS2_PLACEMENT_3D('',#42747,#30096,#30097);
#25065=AXIS2_PLACEMENT_3D('',#42801,#30099,#30100);
#25066=AXIS2_PLACEMENT_3D('',#42849,#30102,#30103);
#25067=AXIS2_PLACEMENT_3D('',#42897,#30105,#30106);
#25068=AXIS2_PLACEMENT_3D('',#42945,#30108,#30109);
#25069=AXIS2_PLACEMENT_3D('',#42999,#30111,#30112);
#25070=AXIS2_PLACEMENT_3D('',#43047,#30114,#30115);
#25071=AXIS2_PLACEMENT_3D('',#43095,#30117,#30118);
#25072=AXIS2_PLACEMENT_3D('',#43149,#30120,#30121);
#25073=AXIS2_PLACEMENT_3D('',#43197,#30123,#30124);
#25074=AXIS2_PLACEMENT_3D('',#43245,#30126,#30127);
#25075=AXIS2_PLACEMENT_3D('',#43293,#30129,#30130);
#25076=AXIS2_PLACEMENT_3D('',#43347,#30132,#30133);
#25077=AXIS2_PLACEMENT_3D('',#43395,#30135,#30136);
#25078=AXIS2_PLACEMENT_3D('',#43443,#30138,#30139);
#25079=AXIS2_PLACEMENT_3D('',#43497,#30141,#30142);
#25080=AXIS2_PLACEMENT_3D('',#43545,#30144,#30145);
#25081=AXIS2_PLACEMENT_3D('',#43593,#30147,#30148);
#25082=AXIS2_PLACEMENT_3D('',#43644,#30150,#30151);
#25083=AXIS2_PLACEMENT_3D('',#43695,#30153,#30154);
#25084=AXIS2_PLACEMENT_3D('',#43743,#30156,#30157);
#25085=AXIS2_PLACEMENT_3D('',#43791,#30159,#30160);
#25086=AXIS2_PLACEMENT_3D('',#43845,#30162,#30163);
#25087=AXIS2_PLACEMENT_3D('',#43893,#30165,#30166);
#25088=AXIS2_PLACEMENT_3D('',#43941,#30168,#30169);
#25089=AXIS2_PLACEMENT_3D('',#43995,#30171,#30172);
#25090=AXIS2_PLACEMENT_3D('',#44043,#30174,#30175);
#25091=AXIS2_PLACEMENT_3D('',#44091,#30177,#30178);
#25092=AXIS2_PLACEMENT_3D('',#44139,#30180,#30181);
#25093=AXIS2_PLACEMENT_3D('',#44193,#30183,#30184);
#25094=AXIS2_PLACEMENT_3D('',#44241,#30186,#30187);
#25095=AXIS2_PLACEMENT_3D('',#44289,#30189,#30190);
#25096=AXIS2_PLACEMENT_3D('',#44343,#30192,#30193);
#25097=AXIS2_PLACEMENT_3D('',#44391,#30195,#30196);
#25098=AXIS2_PLACEMENT_3D('',#44439,#30198,#30199);
#25099=AXIS2_PLACEMENT_3D('',#44487,#30201,#30202);
#25100=AXIS2_PLACEMENT_3D('',#44541,#30204,#30205);
#25101=AXIS2_PLACEMENT_3D('',#44553,#30207,#30208);
#25102=AXIS2_PLACEMENT_3D('',#44559,#30209,#30210);
#25103=AXIS2_PLACEMENT_3D('',#44584,#30212,#30213);
#25104=AXIS2_PLACEMENT_3D('',#44609,#30215,#30216);
#25105=AXIS2_PLACEMENT_3D('',#44633,#30218,#30219);
#25106=AXIS2_PLACEMENT_3D('',#44657,#30221,#30222);
#25107=AXIS2_PLACEMENT_3D('',#44682,#30224,#30225);
#25108=AXIS2_PLACEMENT_3D('',#44707,#30227,#30228);
#25109=AXIS2_PLACEMENT_3D('',#44731,#30230,#30231);
#25110=AXIS2_PLACEMENT_3D('',#44756,#30233,#30234);
#25111=AXIS2_PLACEMENT_3D('',#44781,#30236,#30237);
#25112=AXIS2_PLACEMENT_3D('',#44805,#30239,#30240);
#25113=AXIS2_PLACEMENT_3D('',#44829,#30242,#30243);
#25114=AXIS2_PLACEMENT_3D('',#44854,#30245,#30246);
#25115=AXIS2_PLACEMENT_3D('',#44879,#30248,#30249);
#25116=AXIS2_PLACEMENT_3D('',#44903,#30251,#30252);
#25117=AXIS2_PLACEMENT_3D('',#44928,#30254,#30255);
#25118=AXIS2_PLACEMENT_3D('',#44953,#30257,#30258);
#25119=AXIS2_PLACEMENT_3D('',#44977,#30260,#30261);
#25120=AXIS2_PLACEMENT_3D('',#45002,#30263,#30264);
#25121=AXIS2_PLACEMENT_3D('',#45026,#30266,#30267);
#25122=AXIS2_PLACEMENT_3D('',#45051,#30269,#30270);
#25123=AXIS2_PLACEMENT_3D('',#45075,#30272,#30273);
#25124=AXIS2_PLACEMENT_3D('',#45100,#30275,#30276);
#25125=AXIS2_PLACEMENT_3D('',#45125,#30278,#30279);
#25126=AXIS2_PLACEMENT_3D('',#45149,#30281,#30282);
#25127=AXIS2_PLACEMENT_3D('',#45174,#30284,#30285);
#25128=AXIS2_PLACEMENT_3D('',#45199,#30287,#30288);
#25129=AXIS2_PLACEMENT_3D('',#45223,#30290,#30291);
#25130=AXIS2_PLACEMENT_3D('',#45247,#30293,#30294);
#25131=AXIS2_PLACEMENT_3D('',#45272,#30296,#30297);
#25132=AXIS2_PLACEMENT_3D('',#45297,#30299,#30300);
#25133=AXIS2_PLACEMENT_3D('',#45321,#30302,#30303);
#25134=AXIS2_PLACEMENT_3D('',#45346,#30305,#30306);
#25135=AXIS2_PLACEMENT_3D('',#45371,#30308,#30309);
#25136=AXIS2_PLACEMENT_3D('',#45395,#30311,#30312);
#25137=AXIS2_PLACEMENT_3D('',#45419,#30314,#30315);
#25138=AXIS2_PLACEMENT_3D('',#45444,#30317,#30318);
#25139=AXIS2_PLACEMENT_3D('',#45469,#30320,#30321);
#25140=AXIS2_PLACEMENT_3D('',#45493,#30323,#30324);
#25141=AXIS2_PLACEMENT_3D('',#45518,#30326,#30327);
#25142=AXIS2_PLACEMENT_3D('',#45543,#30329,#30330);
#25143=AXIS2_PLACEMENT_3D('',#45567,#30332,#30333);
#25144=AXIS2_PLACEMENT_3D('',#45592,#30335,#30336);
#25145=AXIS2_PLACEMENT_3D('',#45616,#30338,#30339);
#25146=AXIS2_PLACEMENT_3D('',#45641,#30341,#30342);
#25147=AXIS2_PLACEMENT_3D('',#45665,#30344,#30345);
#25148=AXIS2_PLACEMENT_3D('',#45690,#30347,#30348);
#25149=AXIS2_PLACEMENT_3D('',#45715,#30350,#30351);
#25150=AXIS2_PLACEMENT_3D('',#45739,#30353,#30354);
#25151=AXIS2_PLACEMENT_3D('',#45764,#30356,#30357);
#25152=AXIS2_PLACEMENT_3D('',#45789,#30359,#30360);
#25153=AXIS2_PLACEMENT_3D('',#45813,#30362,#30363);
#25154=AXIS2_PLACEMENT_3D('',#45837,#30365,#30366);
#25155=AXIS2_PLACEMENT_3D('',#45862,#30368,#30369);
#25156=AXIS2_PLACEMENT_3D('',#45887,#30371,#30372);
#25157=AXIS2_PLACEMENT_3D('',#45911,#30374,#30375);
#25158=AXIS2_PLACEMENT_3D('',#45936,#30377,#30378);
#25159=AXIS2_PLACEMENT_3D('',#45961,#30380,#30381);
#25160=AXIS2_PLACEMENT_3D('',#45985,#30383,#30384);
#25161=AXIS2_PLACEMENT_3D('',#46040,#30385,#30386);
#25162=AXIS2_PLACEMENT_3D('',#46042,#30387,#30388);
#25163=AXIS2_PLACEMENT_3D('',#47664,#30389,#30390);
#25164=AXIS2_PLACEMENT_3D('',#47718,#30391,#30392);
#25165=AXIS2_PLACEMENT_3D('',#47719,#30393,#30394);
#25166=AXIS2_PLACEMENT_3D('',#49232,#30395,#30396);
#25167=AXIS2_PLACEMENT_3D('',#49235,#30397,#30398);
#25168=AXIS2_PLACEMENT_3D('',#49239,#30401,#30402);
#25169=AXIS2_PLACEMENT_3D('',#49247,#30405,#30406);
#25170=AXIS2_PLACEMENT_3D('',#49253,#30408,#30409);
#25171=AXIS2_PLACEMENT_3D('',#49256,#30410,#30411);
#25172=AXIS2_PLACEMENT_3D('',#49260,#30414,#30415);
#25173=AXIS2_PLACEMENT_3D('',#49268,#30418,#30419);
#25174=AXIS2_PLACEMENT_3D('',#49274,#30421,#30422);
#25175=AXIS2_PLACEMENT_3D('',#49277,#30423,#30424);
#25176=AXIS2_PLACEMENT_3D('',#49281,#30427,#30428);
#25177=AXIS2_PLACEMENT_3D('',#49289,#30431,#30432);
#25178=AXIS2_PLACEMENT_3D('',#49295,#30434,#30435);
#25179=AXIS2_PLACEMENT_3D('',#49298,#30436,#30437);
#25180=AXIS2_PLACEMENT_3D('',#49302,#30440,#30441);
#25181=AXIS2_PLACEMENT_3D('',#49310,#30444,#30445);
#25182=AXIS2_PLACEMENT_3D('',#49316,#30447,#30448);
#25183=AXIS2_PLACEMENT_3D('',#49319,#30449,#30450);
#25184=AXIS2_PLACEMENT_3D('',#49323,#30453,#30454);
#25185=AXIS2_PLACEMENT_3D('',#49331,#30457,#30458);
#25186=AXIS2_PLACEMENT_3D('',#49337,#30460,#30461);
#25187=AXIS2_PLACEMENT_3D('',#49340,#30462,#30463);
#25188=AXIS2_PLACEMENT_3D('',#49344,#30466,#30467);
#25189=AXIS2_PLACEMENT_3D('',#49352,#30470,#30471);
#25190=AXIS2_PLACEMENT_3D('',#49358,#30473,#30474);
#25191=AXIS2_PLACEMENT_3D('',#49361,#30475,#30476);
#25192=AXIS2_PLACEMENT_3D('',#49365,#30479,#30480);
#25193=AXIS2_PLACEMENT_3D('',#49373,#30483,#30484);
#25194=AXIS2_PLACEMENT_3D('',#49379,#30486,#30487);
#25195=AXIS2_PLACEMENT_3D('',#49382,#30488,#30489);
#25196=AXIS2_PLACEMENT_3D('',#49386,#30492,#30493);
#25197=AXIS2_PLACEMENT_3D('',#49394,#30496,#30497);
#25198=AXIS2_PLACEMENT_3D('',#49400,#30499,#30500);
#25199=AXIS2_PLACEMENT_3D('',#49403,#30501,#30502);
#25200=AXIS2_PLACEMENT_3D('',#49407,#30505,#30506);
#25201=AXIS2_PLACEMENT_3D('',#49415,#30509,#30510);
#25202=AXIS2_PLACEMENT_3D('',#49421,#30512,#30513);
#25203=AXIS2_PLACEMENT_3D('',#49424,#30514,#30515);
#25204=AXIS2_PLACEMENT_3D('',#49428,#30518,#30519);
#25205=AXIS2_PLACEMENT_3D('',#49436,#30522,#30523);
#25206=AXIS2_PLACEMENT_3D('',#49442,#30525,#30526);
#25207=AXIS2_PLACEMENT_3D('',#49445,#30527,#30528);
#25208=AXIS2_PLACEMENT_3D('',#49449,#30531,#30532);
#25209=AXIS2_PLACEMENT_3D('',#49457,#30535,#30536);
#25210=AXIS2_PLACEMENT_3D('',#49463,#30538,#30539);
#25211=AXIS2_PLACEMENT_3D('',#49466,#30540,#30541);
#25212=AXIS2_PLACEMENT_3D('',#49470,#30544,#30545);
#25213=AXIS2_PLACEMENT_3D('',#49478,#30548,#30549);
#25214=AXIS2_PLACEMENT_3D('',#49484,#30551,#30552);
#25215=AXIS2_PLACEMENT_3D('',#49487,#30553,#30554);
#25216=AXIS2_PLACEMENT_3D('',#49491,#30557,#30558);
#25217=AXIS2_PLACEMENT_3D('',#49499,#30561,#30562);
#25218=AXIS2_PLACEMENT_3D('',#49505,#30564,#30565);
#25219=AXIS2_PLACEMENT_3D('',#49508,#30566,#30567);
#25220=AXIS2_PLACEMENT_3D('',#49512,#30570,#30571);
#25221=AXIS2_PLACEMENT_3D('',#49520,#30574,#30575);
#25222=AXIS2_PLACEMENT_3D('',#49526,#30577,#30578);
#25223=AXIS2_PLACEMENT_3D('',#49529,#30579,#30580);
#25224=AXIS2_PLACEMENT_3D('',#49533,#30583,#30584);
#25225=AXIS2_PLACEMENT_3D('',#49541,#30587,#30588);
#25226=AXIS2_PLACEMENT_3D('',#49547,#30590,#30591);
#25227=AXIS2_PLACEMENT_3D('',#49550,#30592,#30593);
#25228=AXIS2_PLACEMENT_3D('',#49554,#30596,#30597);
#25229=AXIS2_PLACEMENT_3D('',#49562,#30600,#30601);
#25230=AXIS2_PLACEMENT_3D('',#49568,#30603,#30604);
#25231=AXIS2_PLACEMENT_3D('',#49571,#30605,#30606);
#25232=AXIS2_PLACEMENT_3D('',#49575,#30609,#30610);
#25233=AXIS2_PLACEMENT_3D('',#49583,#30613,#30614);
#25234=AXIS2_PLACEMENT_3D('',#49589,#30616,#30617);
#25235=AXIS2_PLACEMENT_3D('',#49592,#30618,#30619);
#25236=AXIS2_PLACEMENT_3D('',#49597,#30622,#30623);
#25237=AXIS2_PLACEMENT_3D('',#49598,#30624,#30625);
#25238=AXIS2_PLACEMENT_3D('',#49606,#30628,#30629);
#25239=AXIS2_PLACEMENT_3D('',#49612,#30631,#30632);
#25240=AXIS2_PLACEMENT_3D('',#49615,#30633,#30634);
#25241=AXIS2_PLACEMENT_3D('',#49619,#30637,#30638);
#25242=AXIS2_PLACEMENT_3D('',#49627,#30641,#30642);
#25243=AXIS2_PLACEMENT_3D('',#49633,#30644,#30645);
#25244=AXIS2_PLACEMENT_3D('',#49636,#30646,#30647);
#25245=AXIS2_PLACEMENT_3D('',#49640,#30650,#30651);
#25246=AXIS2_PLACEMENT_3D('',#49648,#30654,#30655);
#25247=AXIS2_PLACEMENT_3D('',#49654,#30657,#30658);
#25248=AXIS2_PLACEMENT_3D('',#49657,#30659,#30660);
#25249=AXIS2_PLACEMENT_3D('',#49661,#30663,#30664);
#25250=AXIS2_PLACEMENT_3D('',#49669,#30667,#30668);
#25251=AXIS2_PLACEMENT_3D('',#49675,#30670,#30671);
#25252=AXIS2_PLACEMENT_3D('',#49678,#30672,#30673);
#25253=AXIS2_PLACEMENT_3D('',#49682,#30676,#30677);
#25254=AXIS2_PLACEMENT_3D('',#49690,#30680,#30681);
#25255=AXIS2_PLACEMENT_3D('',#49696,#30683,#30684);
#25256=AXIS2_PLACEMENT_3D('',#49699,#30685,#30686);
#25257=AXIS2_PLACEMENT_3D('',#49703,#30689,#30690);
#25258=AXIS2_PLACEMENT_3D('',#49711,#30693,#30694);
#25259=AXIS2_PLACEMENT_3D('',#49717,#30696,#30697);
#25260=AXIS2_PLACEMENT_3D('',#49720,#30698,#30699);
#25261=AXIS2_PLACEMENT_3D('',#49724,#30702,#30703);
#25262=AXIS2_PLACEMENT_3D('',#49732,#30706,#30707);
#25263=AXIS2_PLACEMENT_3D('',#49738,#30709,#30710);
#25264=AXIS2_PLACEMENT_3D('',#49741,#30711,#30712);
#25265=AXIS2_PLACEMENT_3D('',#49745,#30715,#30716);
#25266=AXIS2_PLACEMENT_3D('',#49753,#30719,#30720);
#25267=AXIS2_PLACEMENT_3D('',#49759,#30722,#30723);
#25268=AXIS2_PLACEMENT_3D('',#49762,#30724,#30725);
#25269=AXIS2_PLACEMENT_3D('',#49766,#30728,#30729);
#25270=AXIS2_PLACEMENT_3D('',#49774,#30732,#30733);
#25271=AXIS2_PLACEMENT_3D('',#49780,#30735,#30736);
#25272=AXIS2_PLACEMENT_3D('',#49783,#30737,#30738);
#25273=AXIS2_PLACEMENT_3D('',#49787,#30741,#30742);
#25274=AXIS2_PLACEMENT_3D('',#49795,#30745,#30746);
#25275=AXIS2_PLACEMENT_3D('',#49801,#30748,#30749);
#25276=AXIS2_PLACEMENT_3D('',#49804,#30750,#30751);
#25277=AXIS2_PLACEMENT_3D('',#49808,#30754,#30755);
#25278=AXIS2_PLACEMENT_3D('',#49816,#30758,#30759);
#25279=AXIS2_PLACEMENT_3D('',#49822,#30761,#30762);
#25280=AXIS2_PLACEMENT_3D('',#49825,#30763,#30764);
#25281=AXIS2_PLACEMENT_3D('',#49829,#30767,#30768);
#25282=AXIS2_PLACEMENT_3D('',#49837,#30771,#30772);
#25283=AXIS2_PLACEMENT_3D('',#49843,#30774,#30775);
#25284=AXIS2_PLACEMENT_3D('',#49846,#30776,#30777);
#25285=AXIS2_PLACEMENT_3D('',#49850,#30780,#30781);
#25286=AXIS2_PLACEMENT_3D('',#49858,#30784,#30785);
#25287=AXIS2_PLACEMENT_3D('',#49864,#30787,#30788);
#25288=AXIS2_PLACEMENT_3D('',#49867,#30789,#30790);
#25289=AXIS2_PLACEMENT_3D('',#49871,#30793,#30794);
#25290=AXIS2_PLACEMENT_3D('',#49879,#30797,#30798);
#25291=AXIS2_PLACEMENT_3D('',#49885,#30800,#30801);
#25292=AXIS2_PLACEMENT_3D('',#49888,#30802,#30803);
#25293=AXIS2_PLACEMENT_3D('',#49892,#30806,#30807);
#25294=AXIS2_PLACEMENT_3D('',#49900,#30810,#30811);
#25295=AXIS2_PLACEMENT_3D('',#49906,#30813,#30814);
#25296=AXIS2_PLACEMENT_3D('',#49909,#30815,#30816);
#25297=AXIS2_PLACEMENT_3D('',#49913,#30819,#30820);
#25298=AXIS2_PLACEMENT_3D('',#49921,#30823,#30824);
#25299=AXIS2_PLACEMENT_3D('',#49927,#30826,#30827);
#25300=AXIS2_PLACEMENT_3D('',#49930,#30828,#30829);
#25301=AXIS2_PLACEMENT_3D('',#49934,#30832,#30833);
#25302=AXIS2_PLACEMENT_3D('',#49942,#30836,#30837);
#25303=AXIS2_PLACEMENT_3D('',#49948,#30839,#30840);
#25304=AXIS2_PLACEMENT_3D('',#49951,#30841,#30842);
#25305=AXIS2_PLACEMENT_3D('',#49955,#30845,#30846);
#25306=AXIS2_PLACEMENT_3D('',#49963,#30849,#30850);
#25307=AXIS2_PLACEMENT_3D('',#49969,#30852,#30853);
#25308=AXIS2_PLACEMENT_3D('',#49970,#30854,#30855);
#25309=AXIS2_PLACEMENT_3D('',#49971,#30856,#30857);
#25310=AXIS2_PLACEMENT_3D('',#49972,#30858,#30859);
#25311=AXIS2_PLACEMENT_3D('',#49973,#30860,#30861);
#25312=AXIS2_PLACEMENT_3D('',#49974,#30862,#30863);
#25313=AXIS2_PLACEMENT_3D('',#49975,#30864,#30865);
#25314=AXIS2_PLACEMENT_3D('',#49976,#30866,#30867);
#25315=AXIS2_PLACEMENT_3D('',#49977,#30868,#30869);
#25316=AXIS2_PLACEMENT_3D('',#49978,#30870,#30871);
#25317=AXIS2_PLACEMENT_3D('',#49979,#30872,#30873);
#25318=AXIS2_PLACEMENT_3D('',#49980,#30874,#30875);
#25319=AXIS2_PLACEMENT_3D('',#49981,#30876,#30877);
#25320=AXIS2_PLACEMENT_3D('',#49982,#30878,#30879);
#25321=AXIS2_PLACEMENT_3D('',#49983,#30880,#30881);
#25322=AXIS2_PLACEMENT_3D('',#49984,#30882,#30883);
#25323=AXIS2_PLACEMENT_3D('',#49985,#30884,#30885);
#25324=AXIS2_PLACEMENT_3D('',#49986,#30886,#30887);
#25325=AXIS2_PLACEMENT_3D('',#49989,#30889,#30890);
#25326=AXIS2_PLACEMENT_3D('',#49990,#30891,#30892);
#25327=AXIS2_PLACEMENT_3D('',#49991,#30893,#30894);
#25328=AXIS2_PLACEMENT_3D('',#49992,#30895,#30896);
#25329=AXIS2_PLACEMENT_3D('',#49993,#30897,#30898);
#25330=AXIS2_PLACEMENT_3D('',#49994,#30899,#30900);
#25331=AXIS2_PLACEMENT_3D('',#49995,#30901,#30902);
#25332=AXIS2_PLACEMENT_3D('',#49996,#30903,#30904);
#25333=AXIS2_PLACEMENT_3D('',#49997,#30905,#30906);
#25334=AXIS2_PLACEMENT_3D('',#49998,#30907,#30908);
#25335=AXIS2_PLACEMENT_3D('',#49999,#30909,#30910);
#25336=AXIS2_PLACEMENT_3D('',#50000,#30911,#30912);
#25337=AXIS2_PLACEMENT_3D('',#50001,#30913,#30914);
#25338=AXIS2_PLACEMENT_3D('',#50002,#30915,#30916);
#25339=AXIS2_PLACEMENT_3D('',#50003,#30917,#30918);
#25340=AXIS2_PLACEMENT_3D('',#50004,#30919,#30920);
#25341=AXIS2_PLACEMENT_3D('',#50005,#30921,#30922);
#25342=AXIS2_PLACEMENT_3D('',#50006,#30923,#30924);
#25343=AXIS2_PLACEMENT_3D('',#50008,#30925,#30926);
#25344=AXIS2_PLACEMENT_3D('',#50012,#30928,#30929);
#25345=AXIS2_PLACEMENT_3D('',#50015,#30931,#30932);
#25346=AXIS2_PLACEMENT_3D('',#50016,#30933,#30934);
#25347=AXIS2_PLACEMENT_3D('',#50024,#30937,#30938);
#25348=AXIS2_PLACEMENT_3D('',#50029,#30940,#30941);
#25349=AXIS2_PLACEMENT_3D('',#50030,#30942,#30943);
#25350=AXIS2_PLACEMENT_3D('',#50032,#30944,#30945);
#25351=AXIS2_PLACEMENT_3D('',#50034,#30947,#30948);
#25352=AXIS2_PLACEMENT_3D('',#50038,#30950,#30951);
#25353=AXIS2_PLACEMENT_3D('',#50039,#30952,#30953);
#25354=AXIS2_PLACEMENT_3D('',#50048,#30958,#30959);
#25355=AXIS2_PLACEMENT_3D('',#50054,#30963,#30964);
#25356=AXIS2_PLACEMENT_3D('',#50060,#30968,#30969);
#25357=AXIS2_PLACEMENT_3D('',#50066,#30973,#30974);
#25358=AXIS2_PLACEMENT_3D('',#50072,#30978,#30979);
#25359=AXIS2_PLACEMENT_3D('',#50075,#30982,#30983);
#25360=AXIS2_PLACEMENT_3D('',#50076,#30984,#30985);
#25361=AXIS2_PLACEMENT_3D('',#50078,#30986,#30987);
#25362=AXIS2_PLACEMENT_3D('',#50079,#30988,#30989);
#25363=AXIS2_PLACEMENT_3D('',#50081,#30991,#30992);
#25364=AXIS2_PLACEMENT_3D('',#50082,#30993,#30994);
#25365=AXIS2_PLACEMENT_3D('',#50083,#30995,#30996);
#25366=AXIS2_PLACEMENT_3D('',#50085,#30997,#30998);
#25367=AXIS2_PLACEMENT_3D('',#50087,#31000,#31001);
#25368=AXIS2_PLACEMENT_3D('',#50088,#31002,#31003);
#25369=AXIS2_PLACEMENT_3D('',#50089,#31004,#31005);
#25370=AXIS2_PLACEMENT_3D('',#50090,#31006,#31007);
#25371=AXIS2_PLACEMENT_3D('',#50118,#31009,#31010);
#25372=AXIS2_PLACEMENT_3D('',#50121,#31012,#31013);
#25373=AXIS2_PLACEMENT_3D('',#50123,#31014,#31015);
#25374=AXIS2_PLACEMENT_3D('',#50143,#31016,#31017);
#25375=AXIS2_PLACEMENT_3D('',#50191,#31019,#31020);
#25376=AXIS2_PLACEMENT_3D('',#50239,#31022,#31023);
#25377=AXIS2_PLACEMENT_3D('',#50287,#31025,#31026);
#25378=AXIS2_PLACEMENT_3D('',#50341,#31028,#31029);
#25379=AXIS2_PLACEMENT_3D('',#50389,#31031,#31032);
#25380=AXIS2_PLACEMENT_3D('',#50437,#31034,#31035);
#25381=AXIS2_PLACEMENT_3D('',#50491,#31037,#31038);
#25382=AXIS2_PLACEMENT_3D('',#50539,#31040,#31041);
#25383=AXIS2_PLACEMENT_3D('',#50587,#31043,#31044);
#25384=AXIS2_PLACEMENT_3D('',#50635,#31046,#31047);
#25385=AXIS2_PLACEMENT_3D('',#50689,#31049,#31050);
#25386=AXIS2_PLACEMENT_3D('',#50737,#31052,#31053);
#25387=AXIS2_PLACEMENT_3D('',#50785,#31055,#31056);
#25388=AXIS2_PLACEMENT_3D('',#50839,#31058,#31059);
#25389=AXIS2_PLACEMENT_3D('',#50887,#31061,#31062);
#25390=AXIS2_PLACEMENT_3D('',#50935,#31064,#31065);
#25391=AXIS2_PLACEMENT_3D('',#50983,#31067,#31068);
#25392=AXIS2_PLACEMENT_3D('',#50996,#31070,#31071);
#25393=AXIS2_PLACEMENT_3D('',#51002,#31072,#31073);
#25394=AXIS2_PLACEMENT_3D('',#51027,#31075,#31076);
#25395=AXIS2_PLACEMENT_3D('',#51051,#31078,#31079);
#25396=AXIS2_PLACEMENT_3D('',#51075,#31081,#31082);
#25397=AXIS2_PLACEMENT_3D('',#51100,#31084,#31085);
#25398=AXIS2_PLACEMENT_3D('',#51125,#31087,#31088);
#25399=AXIS2_PLACEMENT_3D('',#51149,#31090,#31091);
#25400=AXIS2_PLACEMENT_3D('',#51174,#31093,#31094);
#25401=AXIS2_PLACEMENT_3D('',#51199,#31096,#31097);
#25402=AXIS2_PLACEMENT_3D('',#51223,#31099,#31100);
#25403=AXIS2_PLACEMENT_3D('',#51247,#31102,#31103);
#25404=AXIS2_PLACEMENT_3D('',#51272,#31105,#31106);
#25405=AXIS2_PLACEMENT_3D('',#51297,#31108,#31109);
#25406=AXIS2_PLACEMENT_3D('',#51321,#31111,#31112);
#25407=AXIS2_PLACEMENT_3D('',#51346,#31114,#31115);
#25408=AXIS2_PLACEMENT_3D('',#51371,#31117,#31118);
#25409=AXIS2_PLACEMENT_3D('',#51395,#31120,#31121);
#25410=AXIS2_PLACEMENT_3D('',#51419,#31123,#31124);
#25411=AXIS2_PLACEMENT_3D('',#51444,#31126,#31127);
#25412=AXIS2_PLACEMENT_3D('',#51505,#31128,#31129);
#25413=AXIS2_PLACEMENT_3D('',#51507,#31130,#31131);
#25414=AXIS2_PLACEMENT_3D('',#52146,#31132,#31133);
#25415=AXIS2_PLACEMENT_3D('',#52206,#31134,#31135);
#25416=AXIS2_PLACEMENT_3D('',#52207,#31136,#31137);
#25417=AXIS2_PLACEMENT_3D('',#52724,#31138,#31139);
#25418=AXIS2_PLACEMENT_3D('',#52727,#31140,#31141);
#25419=AXIS2_PLACEMENT_3D('',#52731,#31144,#31145);
#25420=AXIS2_PLACEMENT_3D('',#52739,#31148,#31149);
#25421=AXIS2_PLACEMENT_3D('',#52745,#31151,#31152);
#25422=AXIS2_PLACEMENT_3D('',#52748,#31153,#31154);
#25423=AXIS2_PLACEMENT_3D('',#52752,#31157,#31158);
#25424=AXIS2_PLACEMENT_3D('',#52760,#31161,#31162);
#25425=AXIS2_PLACEMENT_3D('',#52766,#31164,#31165);
#25426=AXIS2_PLACEMENT_3D('',#52769,#31166,#31167);
#25427=AXIS2_PLACEMENT_3D('',#52773,#31170,#31171);
#25428=AXIS2_PLACEMENT_3D('',#52781,#31174,#31175);
#25429=AXIS2_PLACEMENT_3D('',#52787,#31177,#31178);
#25430=AXIS2_PLACEMENT_3D('',#52790,#31179,#31180);
#25431=AXIS2_PLACEMENT_3D('',#52794,#31183,#31184);
#25432=AXIS2_PLACEMENT_3D('',#52802,#31187,#31188);
#25433=AXIS2_PLACEMENT_3D('',#52808,#31190,#31191);
#25434=AXIS2_PLACEMENT_3D('',#52811,#31192,#31193);
#25435=AXIS2_PLACEMENT_3D('',#52815,#31196,#31197);
#25436=AXIS2_PLACEMENT_3D('',#52823,#31200,#31201);
#25437=AXIS2_PLACEMENT_3D('',#52829,#31203,#31204);
#25438=AXIS2_PLACEMENT_3D('',#52832,#31205,#31206);
#25439=AXIS2_PLACEMENT_3D('',#52836,#31209,#31210);
#25440=AXIS2_PLACEMENT_3D('',#52844,#31213,#31214);
#25441=AXIS2_PLACEMENT_3D('',#52850,#31216,#31217);
#25442=AXIS2_PLACEMENT_3D('',#52853,#31218,#31219);
#25443=AXIS2_PLACEMENT_3D('',#52857,#31222,#31223);
#25444=AXIS2_PLACEMENT_3D('',#52865,#31226,#31227);
#25445=AXIS2_PLACEMENT_3D('',#52871,#31229,#31230);
#25446=AXIS2_PLACEMENT_3D('',#52874,#31231,#31232);
#25447=AXIS2_PLACEMENT_3D('',#52878,#31235,#31236);
#25448=AXIS2_PLACEMENT_3D('',#52886,#31239,#31240);
#25449=AXIS2_PLACEMENT_3D('',#52892,#31242,#31243);
#25450=AXIS2_PLACEMENT_3D('',#52895,#31244,#31245);
#25451=AXIS2_PLACEMENT_3D('',#52899,#31248,#31249);
#25452=AXIS2_PLACEMENT_3D('',#52907,#31252,#31253);
#25453=AXIS2_PLACEMENT_3D('',#52913,#31255,#31256);
#25454=AXIS2_PLACEMENT_3D('',#52916,#31257,#31258);
#25455=AXIS2_PLACEMENT_3D('',#52920,#31261,#31262);
#25456=AXIS2_PLACEMENT_3D('',#52928,#31265,#31266);
#25457=AXIS2_PLACEMENT_3D('',#52934,#31268,#31269);
#25458=AXIS2_PLACEMENT_3D('',#52937,#31270,#31271);
#25459=AXIS2_PLACEMENT_3D('',#52941,#31274,#31275);
#25460=AXIS2_PLACEMENT_3D('',#52949,#31278,#31279);
#25461=AXIS2_PLACEMENT_3D('',#52955,#31281,#31282);
#25462=AXIS2_PLACEMENT_3D('',#52958,#31283,#31284);
#25463=AXIS2_PLACEMENT_3D('',#52962,#31287,#31288);
#25464=AXIS2_PLACEMENT_3D('',#52970,#31291,#31292);
#25465=AXIS2_PLACEMENT_3D('',#52976,#31294,#31295);
#25466=AXIS2_PLACEMENT_3D('',#52979,#31296,#31297);
#25467=AXIS2_PLACEMENT_3D('',#52983,#31300,#31301);
#25468=AXIS2_PLACEMENT_3D('',#52991,#31304,#31305);
#25469=AXIS2_PLACEMENT_3D('',#52997,#31307,#31308);
#25470=AXIS2_PLACEMENT_3D('',#53000,#31309,#31310);
#25471=AXIS2_PLACEMENT_3D('',#53004,#31313,#31314);
#25472=AXIS2_PLACEMENT_3D('',#53012,#31317,#31318);
#25473=AXIS2_PLACEMENT_3D('',#53018,#31320,#31321);
#25474=AXIS2_PLACEMENT_3D('',#53021,#31322,#31323);
#25475=AXIS2_PLACEMENT_3D('',#53025,#31326,#31327);
#25476=AXIS2_PLACEMENT_3D('',#53033,#31330,#31331);
#25477=AXIS2_PLACEMENT_3D('',#53039,#31333,#31334);
#25478=AXIS2_PLACEMENT_3D('',#53042,#31335,#31336);
#25479=AXIS2_PLACEMENT_3D('',#53046,#31339,#31340);
#25480=AXIS2_PLACEMENT_3D('',#53054,#31343,#31344);
#25481=AXIS2_PLACEMENT_3D('',#53060,#31346,#31347);
#25482=AXIS2_PLACEMENT_3D('',#53063,#31348,#31349);
#25483=AXIS2_PLACEMENT_3D('',#53067,#31352,#31353);
#25484=AXIS2_PLACEMENT_3D('',#53075,#31356,#31357);
#25485=AXIS2_PLACEMENT_3D('',#53081,#31359,#31360);
#25486=AXIS2_PLACEMENT_3D('',#53084,#31361,#31362);
#25487=AXIS2_PLACEMENT_3D('',#53089,#31365,#31366);
#25488=AXIS2_PLACEMENT_3D('',#53090,#31367,#31368);
#25489=AXIS2_PLACEMENT_3D('',#53098,#31371,#31372);
#25490=AXIS2_PLACEMENT_3D('',#53104,#31374,#31375);
#25491=AXIS2_PLACEMENT_3D('',#53107,#31376,#31377);
#25492=AXIS2_PLACEMENT_3D('',#53111,#31380,#31381);
#25493=AXIS2_PLACEMENT_3D('',#53119,#31384,#31385);
#25494=AXIS2_PLACEMENT_3D('',#53125,#31387,#31388);
#25495=AXIS2_PLACEMENT_3D('',#53128,#31389,#31390);
#25496=AXIS2_PLACEMENT_3D('',#53132,#31393,#31394);
#25497=AXIS2_PLACEMENT_3D('',#53140,#31397,#31398);
#25498=AXIS2_PLACEMENT_3D('',#53146,#31400,#31401);
#25499=AXIS2_PLACEMENT_3D('',#53149,#31402,#31403);
#25500=AXIS2_PLACEMENT_3D('',#53153,#31406,#31407);
#25501=AXIS2_PLACEMENT_3D('',#53161,#31410,#31411);
#25502=AXIS2_PLACEMENT_3D('',#53167,#31413,#31414);
#25503=AXIS2_PLACEMENT_3D('',#53170,#31415,#31416);
#25504=AXIS2_PLACEMENT_3D('',#53174,#31419,#31420);
#25505=AXIS2_PLACEMENT_3D('',#53182,#31423,#31424);
#25506=AXIS2_PLACEMENT_3D('',#53188,#31426,#31427);
#25507=AXIS2_PLACEMENT_3D('',#53191,#31428,#31429);
#25508=AXIS2_PLACEMENT_3D('',#53195,#31432,#31433);
#25509=AXIS2_PLACEMENT_3D('',#53203,#31436,#31437);
#25510=AXIS2_PLACEMENT_3D('',#53209,#31439,#31440);
#25511=AXIS2_PLACEMENT_3D('',#53212,#31441,#31442);
#25512=AXIS2_PLACEMENT_3D('',#53216,#31445,#31446);
#25513=AXIS2_PLACEMENT_3D('',#53224,#31449,#31450);
#25514=AXIS2_PLACEMENT_3D('',#53230,#31452,#31453);
#25515=AXIS2_PLACEMENT_3D('',#53233,#31454,#31455);
#25516=AXIS2_PLACEMENT_3D('',#53237,#31458,#31459);
#25517=AXIS2_PLACEMENT_3D('',#53245,#31462,#31463);
#25518=AXIS2_PLACEMENT_3D('',#53251,#31465,#31466);
#25519=AXIS2_PLACEMENT_3D('',#53254,#31467,#31468);
#25520=AXIS2_PLACEMENT_3D('',#53258,#31471,#31472);
#25521=AXIS2_PLACEMENT_3D('',#53266,#31475,#31476);
#25522=AXIS2_PLACEMENT_3D('',#53272,#31478,#31479);
#25523=AXIS2_PLACEMENT_3D('',#53275,#31480,#31481);
#25524=AXIS2_PLACEMENT_3D('',#53279,#31484,#31485);
#25525=AXIS2_PLACEMENT_3D('',#53287,#31488,#31489);
#25526=AXIS2_PLACEMENT_3D('',#53293,#31491,#31492);
#25527=AXIS2_PLACEMENT_3D('',#53296,#31493,#31494);
#25528=AXIS2_PLACEMENT_3D('',#53300,#31497,#31498);
#25529=AXIS2_PLACEMENT_3D('',#53308,#31501,#31502);
#25530=AXIS2_PLACEMENT_3D('',#53314,#31504,#31505);
#25531=AXIS2_PLACEMENT_3D('',#53317,#31506,#31507);
#25532=AXIS2_PLACEMENT_3D('',#53321,#31510,#31511);
#25533=AXIS2_PLACEMENT_3D('',#53329,#31514,#31515);
#25534=AXIS2_PLACEMENT_3D('',#53335,#31517,#31518);
#25535=AXIS2_PLACEMENT_3D('',#53338,#31519,#31520);
#25536=AXIS2_PLACEMENT_3D('',#53342,#31523,#31524);
#25537=AXIS2_PLACEMENT_3D('',#53350,#31527,#31528);
#25538=AXIS2_PLACEMENT_3D('',#53356,#31530,#31531);
#25539=AXIS2_PLACEMENT_3D('',#53359,#31532,#31533);
#25540=AXIS2_PLACEMENT_3D('',#53363,#31536,#31537);
#25541=AXIS2_PLACEMENT_3D('',#53371,#31540,#31541);
#25542=AXIS2_PLACEMENT_3D('',#53377,#31543,#31544);
#25543=AXIS2_PLACEMENT_3D('',#53380,#31545,#31546);
#25544=AXIS2_PLACEMENT_3D('',#53384,#31549,#31550);
#25545=AXIS2_PLACEMENT_3D('',#53392,#31553,#31554);
#25546=AXIS2_PLACEMENT_3D('',#53398,#31556,#31557);
#25547=AXIS2_PLACEMENT_3D('',#53401,#31558,#31559);
#25548=AXIS2_PLACEMENT_3D('',#53405,#31562,#31563);
#25549=AXIS2_PLACEMENT_3D('',#53413,#31566,#31567);
#25550=AXIS2_PLACEMENT_3D('',#53419,#31569,#31570);
#25551=AXIS2_PLACEMENT_3D('',#53422,#31571,#31572);
#25552=AXIS2_PLACEMENT_3D('',#53426,#31575,#31576);
#25553=AXIS2_PLACEMENT_3D('',#53434,#31579,#31580);
#25554=AXIS2_PLACEMENT_3D('',#53440,#31582,#31583);
#25555=AXIS2_PLACEMENT_3D('',#53443,#31584,#31585);
#25556=AXIS2_PLACEMENT_3D('',#53447,#31588,#31589);
#25557=AXIS2_PLACEMENT_3D('',#53455,#31592,#31593);
#25558=AXIS2_PLACEMENT_3D('',#53461,#31595,#31596);
#25559=AXIS2_PLACEMENT_3D('',#53462,#31597,#31598);
#25560=AXIS2_PLACEMENT_3D('',#53463,#31599,#31600);
#25561=AXIS2_PLACEMENT_3D('',#53464,#31601,#31602);
#25562=AXIS2_PLACEMENT_3D('',#53465,#31603,#31604);
#25563=AXIS2_PLACEMENT_3D('',#53466,#31605,#31606);
#25564=AXIS2_PLACEMENT_3D('',#53467,#31607,#31608);
#25565=AXIS2_PLACEMENT_3D('',#53468,#31609,#31610);
#25566=AXIS2_PLACEMENT_3D('',#53469,#31611,#31612);
#25567=AXIS2_PLACEMENT_3D('',#53470,#31613,#31614);
#25568=AXIS2_PLACEMENT_3D('',#53471,#31615,#31616);
#25569=AXIS2_PLACEMENT_3D('',#53472,#31617,#31618);
#25570=AXIS2_PLACEMENT_3D('',#53473,#31619,#31620);
#25571=AXIS2_PLACEMENT_3D('',#53474,#31621,#31622);
#25572=AXIS2_PLACEMENT_3D('',#53475,#31623,#31624);
#25573=AXIS2_PLACEMENT_3D('',#53476,#31625,#31626);
#25574=AXIS2_PLACEMENT_3D('',#53477,#31627,#31628);
#25575=AXIS2_PLACEMENT_3D('',#53478,#31629,#31630);
#25576=AXIS2_PLACEMENT_3D('',#53481,#31632,#31633);
#25577=AXIS2_PLACEMENT_3D('',#53482,#31634,#31635);
#25578=AXIS2_PLACEMENT_3D('',#53483,#31636,#31637);
#25579=AXIS2_PLACEMENT_3D('',#53484,#31638,#31639);
#25580=AXIS2_PLACEMENT_3D('',#53485,#31640,#31641);
#25581=AXIS2_PLACEMENT_3D('',#53486,#31642,#31643);
#25582=AXIS2_PLACEMENT_3D('',#53487,#31644,#31645);
#25583=AXIS2_PLACEMENT_3D('',#53488,#31646,#31647);
#25584=AXIS2_PLACEMENT_3D('',#53489,#31648,#31649);
#25585=AXIS2_PLACEMENT_3D('',#53490,#31650,#31651);
#25586=AXIS2_PLACEMENT_3D('',#53491,#31652,#31653);
#25587=AXIS2_PLACEMENT_3D('',#53492,#31654,#31655);
#25588=AXIS2_PLACEMENT_3D('',#53493,#31656,#31657);
#25589=AXIS2_PLACEMENT_3D('',#53494,#31658,#31659);
#25590=AXIS2_PLACEMENT_3D('',#53495,#31660,#31661);
#25591=AXIS2_PLACEMENT_3D('',#53496,#31662,#31663);
#25592=AXIS2_PLACEMENT_3D('',#53497,#31664,#31665);
#25593=AXIS2_PLACEMENT_3D('',#53498,#31666,#31667);
#25594=AXIS2_PLACEMENT_3D('',#53500,#31668,#31669);
#25595=AXIS2_PLACEMENT_3D('',#53504,#31671,#31672);
#25596=AXIS2_PLACEMENT_3D('',#53507,#31674,#31675);
#25597=AXIS2_PLACEMENT_3D('',#53508,#31676,#31677);
#25598=AXIS2_PLACEMENT_3D('',#53516,#31680,#31681);
#25599=AXIS2_PLACEMENT_3D('',#53521,#31683,#31684);
#25600=AXIS2_PLACEMENT_3D('',#53522,#31685,#31686);
#25601=AXIS2_PLACEMENT_3D('',#53524,#31687,#31688);
#25602=AXIS2_PLACEMENT_3D('',#53526,#31690,#31691);
#25603=AXIS2_PLACEMENT_3D('',#53530,#31693,#31694);
#25604=AXIS2_PLACEMENT_3D('',#53531,#31695,#31696);
#25605=AXIS2_PLACEMENT_3D('',#53540,#31701,#31702);
#25606=AXIS2_PLACEMENT_3D('',#53546,#31706,#31707);
#25607=AXIS2_PLACEMENT_3D('',#53552,#31711,#31712);
#25608=AXIS2_PLACEMENT_3D('',#53558,#31716,#31717);
#25609=AXIS2_PLACEMENT_3D('',#53564,#31721,#31722);
#25610=AXIS2_PLACEMENT_3D('',#53567,#31725,#31726);
#25611=AXIS2_PLACEMENT_3D('',#53568,#31727,#31728);
#25612=AXIS2_PLACEMENT_3D('',#53570,#31729,#31730);
#25613=AXIS2_PLACEMENT_3D('',#53571,#31731,#31732);
#25614=AXIS2_PLACEMENT_3D('',#53573,#31734,#31735);
#25615=AXIS2_PLACEMENT_3D('',#53574,#31736,#31737);
#25616=AXIS2_PLACEMENT_3D('',#53575,#31738,#31739);
#25617=AXIS2_PLACEMENT_3D('',#53577,#31740,#31741);
#25618=AXIS2_PLACEMENT_3D('',#53579,#31743,#31744);
#25619=AXIS2_PLACEMENT_3D('',#53580,#31745,#31746);
#25620=AXIS2_PLACEMENT_3D('',#53581,#31747,#31748);
#25621=AXIS2_PLACEMENT_3D('',#53582,#31749,#31750);
#25622=AXIS2_PLACEMENT_3D('',#53583,#31751,#31752);
#25623=AXIS2_PLACEMENT_3D('',#53584,#31753,#31754);
#25624=AXIS2_PLACEMENT_3D('',#53585,#31755,#31756);
#25625=AXIS2_PLACEMENT_3D('',#53586,#31757,#31758);
#25626=AXIS2_PLACEMENT_3D('',#53587,#31759,#31760);
#25627=AXIS2_PLACEMENT_3D('',#53588,#31761,#31762);
#25628=AXIS2_PLACEMENT_3D('',#53589,#31763,#31764);
#25629=AXIS2_PLACEMENT_3D('',#53590,#31765,#31766);
#25630=AXIS2_PLACEMENT_3D('',#53591,#31767,#31768);
#25631=AXIS2_PLACEMENT_3D('',#53592,#31769,#31770);
#25632=AXIS2_PLACEMENT_3D('',#53593,#31771,#31772);
#25633=AXIS2_PLACEMENT_3D('',#53594,#31773,#31774);
#25634=AXIS2_PLACEMENT_3D('',#53595,#31775,#31776);
#25635=AXIS2_PLACEMENT_3D('',#53596,#31777,#31778);
#25636=AXIS2_PLACEMENT_3D('',#53597,#31779,#31780);
#25637=AXIS2_PLACEMENT_3D('',#53598,#31781,#31782);
#25638=AXIS2_PLACEMENT_3D('',#53599,#31783,#31784);
#25639=AXIS2_PLACEMENT_3D('',#53600,#31785,#31786);
#25640=AXIS2_PLACEMENT_3D('',#53601,#31787,#31788);
#25641=AXIS2_PLACEMENT_3D('',#53602,#31789,#31790);
#25642=AXIS2_PLACEMENT_3D('',#53603,#31791,#31792);
#25643=AXIS2_PLACEMENT_3D('',#53604,#31793,#31794);
#25644=AXIS2_PLACEMENT_3D('',#53605,#31795,#31796);
#25645=AXIS2_PLACEMENT_3D('',#53606,#31797,#31798);
#25646=AXIS2_PLACEMENT_3D('',#53607,#31799,#31800);
#25647=AXIS2_PLACEMENT_3D('',#53608,#31801,#31802);
#25648=AXIS2_PLACEMENT_3D('',#53609,#31803,#31804);
#25649=AXIS2_PLACEMENT_3D('',#53610,#31805,#31806);
#25650=AXIS2_PLACEMENT_3D('',#53611,#31807,#31808);
#25651=AXIS2_PLACEMENT_3D('',#53612,#31809,#31810);
#25652=AXIS2_PLACEMENT_3D('',#53613,#31811,#31812);
#25653=AXIS2_PLACEMENT_3D('',#53614,#31813,#31814);
#25654=DIRECTION('axis',(0.,0.,1.));
#25655=DIRECTION('refdir',(1.,0.,0.));
#25656=DIRECTION('axis',(0.,0.,1.));
#25657=DIRECTION('refdir',(1.,0.,0.));
#25658=DIRECTION('center_axis',(0.,0.,-1.));
#25659=DIRECTION('ref_axis',(-0.707106781186548,-0.707106781186548,0.));
#25660=DIRECTION('',(-0.923879532511286,0.,-0.382683432365092));
#25661=DIRECTION('center_axis',(0.,0.,1.));
#25662=DIRECTION('ref_axis',(-0.707106781186547,-0.707106781186547,0.));
#25663=DIRECTION('',(0.,0.923879532511286,0.382683432365092));
#25664=DIRECTION('center_axis',(0.,0.,-1.));
#25665=DIRECTION('ref_axis',(-0.707106781186547,-0.707106781186547,0.));
#25666=DIRECTION('center_axis',(-0.382683432365103,0.,0.923879532511281));
#25667=DIRECTION('ref_axis',(0.923879532511281,0.,0.382683432365103));
#25668=DIRECTION('',(-0.923879532511283,0.,-0.3826834323651));
#25669=DIRECTION('',(0.,-1.,0.));
#25670=DIRECTION('',(0.,1.,0.));
#25671=DIRECTION('center_axis',(0.,0.,-1.));
#25672=DIRECTION('ref_axis',(-0.707106781186548,0.707106781186548,0.));
#25673=DIRECTION('',(0.,0.923879532511286,-0.382683432365092));
#25674=DIRECTION('center_axis',(0.,0.,1.));
#25675=DIRECTION('ref_axis',(-0.707106781186547,0.707106781186547,0.));
#25676=DIRECTION('center_axis',(0.,0.,-1.));
#25677=DIRECTION('ref_axis',(-0.707106781186547,0.707106781186547,0.));
#25678=DIRECTION('center_axis',(0.,0.382683432365094,0.923879532511285));
#25679=DIRECTION('ref_axis',(1.,0.,0.));
#25680=DIRECTION('',(0.,0.923879532511285,-0.382683432365094));
#25681=DIRECTION('',(-1.,0.,0.));
#25682=DIRECTION('',(1.,0.,0.));
#25683=DIRECTION('center_axis',(0.,0.,-1.));
#25684=DIRECTION('ref_axis',(0.707106781186548,0.707106781186548,0.));
#25685=DIRECTION('',(0.923879532511286,0.,-0.382683432365092));
#25686=DIRECTION('center_axis',(0.,0.,1.));
#25687=DIRECTION('ref_axis',(0.707106781186547,0.707106781186547,0.));
#25688=DIRECTION('center_axis',(0.,0.,-1.));
#25689=DIRECTION('ref_axis',(0.707106781186547,0.707106781186547,0.));
#25690=DIRECTION('center_axis',(0.382683432365103,0.,0.923879532511281));
#25691=DIRECTION('ref_axis',(0.923879532511281,0.,-0.382683432365103));
#25692=DIRECTION('',(0.923879532511283,0.,-0.3826834323651));
#25693=DIRECTION('',(0.,1.,0.));
#25694=DIRECTION('',(0.,-1.,0.));
#25695=DIRECTION('center_axis',(0.,0.,-1.));
#25696=DIRECTION('ref_axis',(0.707106781186548,-0.707106781186548,0.));
#25697=DIRECTION('',(0.,-0.923879532511286,-0.382683432365092));
#25698=DIRECTION('center_axis',(0.,0.,1.));
#25699=DIRECTION('ref_axis',(0.707106781186547,-0.707106781186547,0.));
#25700=DIRECTION('center_axis',(0.,0.,-1.));
#25701=DIRECTION('ref_axis',(0.707106781186547,-0.707106781186547,0.));
#25702=DIRECTION('center_axis',(0.,-0.382683432365094,0.923879532511285));
#25703=DIRECTION('ref_axis',(1.,0.,0.));
#25704=DIRECTION('',(1.,0.,0.));
#25705=DIRECTION('',(-1.,0.,0.));
#25706=DIRECTION('center_axis',(0.707106781186549,0.,0.707106781186546));
#25707=DIRECTION('ref_axis',(0.707106781186546,0.,-0.707106781186549));
#25708=DIRECTION('',(0.707106781186546,0.,-0.707106781186549));
#25709=DIRECTION('',(0.,-1.,0.));
#25710=DIRECTION('',(0.707106781186546,0.,-0.707106781186549));
#25711=DIRECTION('center_axis',(0.,0.,-1.));
#25712=DIRECTION('ref_axis',(0.707106781186548,-0.707106781186548,0.));
#25713=DIRECTION('',(0.,-0.707106781186546,-0.707106781186549));
#25714=DIRECTION('center_axis',(0.,0.,-1.));
#25715=DIRECTION('ref_axis',(0.707106781186547,-0.707106781186547,0.));
#25716=DIRECTION('center_axis',(0.,-0.707106781186549,0.707106781186546));
#25717=DIRECTION('ref_axis',(1.,0.,0.));
#25718=DIRECTION('',(0.,0.707106781186546,0.707106781186549));
#25719=DIRECTION('',(-1.,0.,0.));
#25720=DIRECTION('center_axis',(0.,0.,-1.));
#25721=DIRECTION('ref_axis',(-0.707106781186548,-0.707106781186548,0.));
#25722=DIRECTION('',(-0.707106781186546,0.,-0.707106781186549));
#25723=DIRECTION('center_axis',(0.,0.,-1.));
#25724=DIRECTION('ref_axis',(-0.707106781186547,-0.707106781186547,0.));
#25725=DIRECTION('center_axis',(0.,0.,1.));
#25726=DIRECTION('ref_axis',(1.,0.,0.));
#25727=DIRECTION('center_axis',(0.,0.,1.));
#25728=DIRECTION('ref_axis',(-1.,0.,0.));
#25729=DIRECTION('center_axis',(0.,0.,1.));
#25730=DIRECTION('ref_axis',(-1.,0.,0.));
#25731=DIRECTION('center_axis',(0.,0.,-1.));
#25732=DIRECTION('ref_axis',(-1.,0.,0.));
#25733=DIRECTION('center_axis',(0.,0.,-1.));
#25734=DIRECTION('ref_axis',(-1.,0.,0.));
#25735=DIRECTION('center_axis',(0.,0.,-1.));
#25736=DIRECTION('ref_axis',(-1.,0.,0.));
#25737=DIRECTION('center_axis',(0.,0.,1.));
#25738=DIRECTION('ref_axis',(-1.,0.,0.));
#25739=DIRECTION('center_axis',(0.,0.,1.));
#25740=DIRECTION('ref_axis',(-1.,0.,0.));
#25741=DIRECTION('center_axis',(0.,0.,-1.));
#25742=DIRECTION('ref_axis',(-0.707106781186547,-0.707106781186547,0.));
#25743=DIRECTION('',(0.,0.382683432365082,0.92387953251129));
#25744=DIRECTION('',(-0.382683432365082,0.,-0.92387953251129));
#25745=DIRECTION('center_axis',(0.,0.,1.));
#25746=DIRECTION('ref_axis',(-0.707106781186547,-0.707106781186547,0.));
#25747=DIRECTION('center_axis',(0.,-0.923879532511285,0.382683432365094));
#25748=DIRECTION('ref_axis',(0.,-0.382683432365094,-0.923879532511285));
#25749=DIRECTION('',(0.,0.382683432365095,0.923879532511285));
#25750=DIRECTION('',(1.,0.,0.));
#25751=DIRECTION('center_axis',(0.,0.,-1.));
#25752=DIRECTION('ref_axis',(0.707106781186547,-0.707106781186547,0.));
#25753=DIRECTION('',(-0.382683432365082,0.,0.92387953251129));
#25754=DIRECTION('center_axis',(0.,0.,1.));
#25755=DIRECTION('ref_axis',(0.707106781186547,-0.707106781186547,0.));
#25756=DIRECTION('center_axis',(0.923879532511285,0.,0.382683432365094));
#25757=DIRECTION('ref_axis',(0.382683432365094,0.,-0.923879532511285));
#25758=DIRECTION('',(-0.382683432365095,0.,0.923879532511285));
#25759=DIRECTION('',(0.,1.,0.));
#25760=DIRECTION('center_axis',(0.,0.,-1.));
#25761=DIRECTION('ref_axis',(0.707106781186547,0.707106781186547,0.));
#25762=DIRECTION('',(0.,-0.382683432365082,0.92387953251129));
#25763=DIRECTION('center_axis',(0.,0.,-1.));
#25764=DIRECTION('ref_axis',(0.707106781186547,0.707106781186547,0.));
#25765=DIRECTION('center_axis',(0.,0.,1.));
#25766=DIRECTION('ref_axis',(0.707106781186547,0.707106781186547,0.));
#25767=DIRECTION('center_axis',(0.,0.923879532511285,0.382683432365094));
#25768=DIRECTION('ref_axis',(0.,-0.382683432365094,0.923879532511285));
#25769=DIRECTION('',(0.,-0.382683432365095,0.923879532511285));
#25770=DIRECTION('',(1.,0.,0.));
#25771=DIRECTION('',(-1.,0.,0.));
#25772=DIRECTION('center_axis',(0.,0.,-1.));
#25773=DIRECTION('ref_axis',(-0.707106781186547,0.707106781186547,0.));
#25774=DIRECTION('',(0.382683432365082,0.,0.92387953251129));
#25775=DIRECTION('center_axis',(0.,0.,-1.));
#25776=DIRECTION('ref_axis',(-0.707106781186547,0.707106781186547,0.));
#25777=DIRECTION('center_axis',(0.,0.,1.));
#25778=DIRECTION('ref_axis',(-0.707106781186547,0.707106781186547,0.));
#25779=DIRECTION('center_axis',(-0.923879532511285,0.,0.382683432365094));
#25780=DIRECTION('ref_axis',(0.382683432365094,0.,0.923879532511285));
#25781=DIRECTION('',(0.,1.,0.));
#25782=DIRECTION('',(0.,-1.,0.));
#25783=DIRECTION('center_axis',(1.,0.,0.));
#25784=DIRECTION('ref_axis',(0.,1.,0.));
#25785=DIRECTION('',(0.,0.,1.));
#25786=DIRECTION('',(0.,-1.,0.));
#25787=DIRECTION('',(0.,0.,-1.));
#25788=DIRECTION('center_axis',(0.,0.,1.));
#25789=DIRECTION('ref_axis',(0.707106781186547,-0.707106781186547,0.));
#25790=DIRECTION('',(0.,0.,-1.));
#25791=DIRECTION('center_axis',(0.,0.,-1.));
#25792=DIRECTION('ref_axis',(0.707106781186547,-0.707106781186547,0.));
#25793=DIRECTION('center_axis',(0.,-1.,0.));
#25794=DIRECTION('ref_axis',(1.,0.,0.));
#25795=DIRECTION('',(0.,0.,1.));
#25796=DIRECTION('',(-1.,0.,0.));
#25797=DIRECTION('center_axis',(0.,0.,1.));
#25798=DIRECTION('ref_axis',(-0.707106781186547,-0.707106781186547,0.));
#25799=DIRECTION('',(0.,0.,-1.));
#25800=DIRECTION('center_axis',(0.,0.,-1.));
#25801=DIRECTION('ref_axis',(-0.707106781186547,-0.707106781186547,0.));
#25802=DIRECTION('center_axis',(0.,0.707106781186549,0.707106781186546));
#25803=DIRECTION('ref_axis',(1.,0.,0.));
#25804=DIRECTION('',(0.,0.707106781186546,-0.707106781186549));
#25805=DIRECTION('',(0.,0.707106781186546,-0.707106781186549));
#25806=DIRECTION('center_axis',(0.,0.,-1.));
#25807=DIRECTION('ref_axis',(-0.707106781186548,0.707106781186548,0.));
#25808=DIRECTION('',(-0.707106781186546,0.,-0.707106781186549));
#25809=DIRECTION('center_axis',(-0.707106781186549,0.,0.707106781186546));
#25810=DIRECTION('ref_axis',(0.707106781186546,0.,0.707106781186549));
#25811=DIRECTION('center_axis',(0.38268343236509,0.,-0.923879532511287));
#25812=DIRECTION('ref_axis',(-0.923879532511287,0.,-0.38268343236509));
#25813=DIRECTION('',(0.923879532511288,0.,0.382683432365087));
#25814=DIRECTION('',(0.,-1.,0.));
#25815=DIRECTION('',(-0.923879532511288,0.,-0.382683432365087));
#25816=DIRECTION('',(0.,1.,0.));
#25817=DIRECTION('center_axis',(0.,0.,1.));
#25818=DIRECTION('ref_axis',(0.707106781186548,0.707106781186548,0.));
#25819=DIRECTION('',(0.,0.923879532511292,0.382683432365076));
#25820=DIRECTION('center_axis',(0.,0.,-1.));
#25821=DIRECTION('ref_axis',(0.707106781186548,0.707106781186548,0.));
#25822=DIRECTION('center_axis',(0.,0.,1.));
#25823=DIRECTION('ref_axis',(0.707106781186548,0.707106781186548,0.));
#25824=DIRECTION('center_axis',(0.,0.382683432365092,-0.923879532511286));
#25825=DIRECTION('ref_axis',(-1.,0.,0.));
#25826=DIRECTION('',(0.,0.923879532511288,0.382683432365088));
#25827=DIRECTION('',(1.,0.,0.));
#25828=DIRECTION('',(-1.,0.,0.));
#25829=DIRECTION('center_axis',(0.,0.,1.));
#25830=DIRECTION('ref_axis',(-0.707106781186548,0.707106781186548,0.));
#25831=DIRECTION('',(-0.923879532511292,0.,0.382683432365076));
#25832=DIRECTION('center_axis',(0.,0.,-1.));
#25833=DIRECTION('ref_axis',(-0.707106781186548,0.707106781186548,0.));
#25834=DIRECTION('center_axis',(0.,0.,1.));
#25835=DIRECTION('ref_axis',(-0.707106781186548,0.707106781186548,0.));
#25836=DIRECTION('center_axis',(-0.38268343236509,0.,-0.923879532511287));
#25837=DIRECTION('ref_axis',(-0.923879532511287,0.,0.38268343236509));
#25838=DIRECTION('',(-0.923879532511288,0.,0.382683432365087));
#25839=DIRECTION('',(0.,1.,0.));
#25840=DIRECTION('',(0.,-1.,0.));
#25841=DIRECTION('center_axis',(0.,0.,1.));
#25842=DIRECTION('ref_axis',(-0.707106781186548,-0.707106781186548,0.));
#25843=DIRECTION('',(0.,-0.923879532511292,0.382683432365076));
#25844=DIRECTION('center_axis',(0.,0.,-1.));
#25845=DIRECTION('ref_axis',(-0.707106781186548,-0.707106781186548,0.));
#25846=DIRECTION('center_axis',(0.,0.,1.));
#25847=DIRECTION('ref_axis',(-0.707106781186548,-0.707106781186548,0.));
#25848=DIRECTION('center_axis',(0.,-0.382683432365092,-0.923879532511286));
#25849=DIRECTION('ref_axis',(-1.,0.,0.));
#25850=DIRECTION('',(0.,-0.923879532511288,0.382683432365088));
#25851=DIRECTION('',(-1.,0.,0.));
#25852=DIRECTION('',(1.,0.,0.));
#25853=DIRECTION('center_axis',(0.,0.,1.));
#25854=DIRECTION('ref_axis',(0.707106781186548,-0.707106781186548,0.));
#25855=DIRECTION('center_axis',(0.,0.,-1.));
#25856=DIRECTION('ref_axis',(0.707106781186548,-0.707106781186548,0.));
#25857=DIRECTION('center_axis',(0.,0.,1.));
#25858=DIRECTION('ref_axis',(0.707106781186548,-0.707106781186548,0.));
#25859=DIRECTION('center_axis',(0.,0.,1.));
#25860=DIRECTION('ref_axis',(-0.707106781186548,-0.707106781186548,0.));
#25861=DIRECTION('',(0.,-0.70710678118654,0.707106781186555));
#25862=DIRECTION('center_axis',(0.,0.,1.));
#25863=DIRECTION('ref_axis',(-0.707106781186547,-0.707106781186547,0.));
#25864=DIRECTION('',(-0.707106781186546,0.,0.707106781186549));
#25865=DIRECTION('center_axis',(0.,-0.707106781186549,-0.707106781186546));
#25866=DIRECTION('ref_axis',(-1.,0.,0.));
#25867=DIRECTION('',(0.,-0.707106781186546,0.707106781186549));
#25868=DIRECTION('',(1.,0.,0.));
#25869=DIRECTION('center_axis',(0.,0.,1.));
#25870=DIRECTION('ref_axis',(0.707106781186548,-0.707106781186548,0.));
#25871=DIRECTION('',(-0.707106781186546,0.,-0.707106781186549));
#25872=DIRECTION('center_axis',(0.,0.,1.));
#25873=DIRECTION('ref_axis',(0.707106781186547,-0.707106781186547,0.));
#25874=DIRECTION('center_axis',(0.707106781186549,0.,-0.707106781186546));
#25875=DIRECTION('ref_axis',(-0.707106781186546,0.,-0.707106781186549));
#25876=DIRECTION('',(0.707106781186546,0.,0.707106781186549));
#25877=DIRECTION('',(0.,1.,0.));
#25878=DIRECTION('center_axis',(0.,0.,1.));
#25879=DIRECTION('ref_axis',(1.,0.,0.));
#25880=DIRECTION('center_axis',(0.,0.,-1.));
#25881=DIRECTION('ref_axis',(1.,0.,0.));
#25882=DIRECTION('center_axis',(0.,0.,-1.));
#25883=DIRECTION('ref_axis',(1.,0.,0.));
#25884=DIRECTION('center_axis',(0.,0.,1.));
#25885=DIRECTION('ref_axis',(1.,0.,0.));
#25886=DIRECTION('center_axis',(0.,0.,1.));
#25887=DIRECTION('ref_axis',(1.,0.,0.));
#25888=DIRECTION('center_axis',(0.,0.,1.));
#25889=DIRECTION('ref_axis',(1.,0.,0.));
#25890=DIRECTION('center_axis',(0.,0.,1.));
#25891=DIRECTION('ref_axis',(1.,0.,0.));
#25892=DIRECTION('center_axis',(0.,0.,-1.));
#25893=DIRECTION('ref_axis',(1.,0.,0.));
#25894=DIRECTION('center_axis',(0.923879532511292,0.,-0.382683432365078));
#25895=DIRECTION('ref_axis',(-0.382683432365078,0.,-0.923879532511292));
#25896=DIRECTION('',(-0.382683432365076,0.,-0.923879532511293));
#25897=DIRECTION('',(0.382683432365076,0.,0.923879532511293));
#25898=DIRECTION('center_axis',(0.,0.,1.));
#25899=DIRECTION('ref_axis',(0.707106781186547,-0.707106781186547,0.));
#25900=DIRECTION('',(0.,0.382683432365084,-0.923879532511289));
#25901=DIRECTION('center_axis',(0.,-0.923879532511292,-0.382683432365078));
#25902=DIRECTION('ref_axis',(0.,0.382683432365078,-0.923879532511292));
#25903=DIRECTION('',(0.,0.382683432365061,-0.923879532511299));
#25904=DIRECTION('center_axis',(0.,0.,1.));
#25905=DIRECTION('ref_axis',(-0.707106781186547,-0.707106781186547,0.));
#25906=DIRECTION('',(0.382683432365084,0.,-0.923879532511289));
#25907=DIRECTION('center_axis',(-0.923879532511292,0.,-0.382683432365078));
#25908=DIRECTION('ref_axis',(-0.382683432365078,0.,0.923879532511292));
#25909=DIRECTION('',(0.382683432365061,0.,-0.923879532511299));
#25910=DIRECTION('',(0.,-1.,0.));
#25911=DIRECTION('',(0.,1.,0.));
#25912=DIRECTION('center_axis',(0.,0.,1.));
#25913=DIRECTION('ref_axis',(-0.707106781186547,0.707106781186547,0.));
#25914=DIRECTION('',(0.,-0.382683432365084,-0.923879532511289));
#25915=DIRECTION('center_axis',(0.,0.,1.));
#25916=DIRECTION('ref_axis',(-0.707106781186547,0.707106781186547,0.));
#25917=DIRECTION('center_axis',(0.,0.,-1.));
#25918=DIRECTION('ref_axis',(-0.707106781186547,0.707106781186547,0.));
#25919=DIRECTION('center_axis',(0.,0.923879532511292,-0.382683432365078));
#25920=DIRECTION('ref_axis',(0.,0.382683432365078,0.923879532511292));
#25921=DIRECTION('',(0.,-0.382683432365061,-0.923879532511299));
#25922=DIRECTION('',(-1.,0.,0.));
#25923=DIRECTION('',(1.,0.,0.));
#25924=DIRECTION('center_axis',(0.,0.,1.));
#25925=DIRECTION('ref_axis',(0.707106781186547,0.707106781186547,0.));
#25926=DIRECTION('center_axis',(0.,0.,1.));
#25927=DIRECTION('ref_axis',(0.707106781186547,0.707106781186547,0.));
#25928=DIRECTION('center_axis',(0.,0.,-1.));
#25929=DIRECTION('ref_axis',(0.707106781186547,0.707106781186547,0.));
#25930=DIRECTION('center_axis',(0.,0.,1.));
#25931=DIRECTION('ref_axis',(-0.707106781186548,0.707106781186548,0.));
#25932=DIRECTION('',(-0.70710678118654,0.,0.707106781186555));
#25933=DIRECTION('',(0.,0.707106781186546,0.707106781186549));
#25934=DIRECTION('center_axis',(0.,0.707106781186549,-0.707106781186546));
#25935=DIRECTION('ref_axis',(-1.,0.,0.));
#25936=DIRECTION('',(0.,0.70710678118654,0.707106781186555));
#25937=DIRECTION('center_axis',(0.,0.,1.));
#25938=DIRECTION('ref_axis',(0.707106781186548,0.707106781186548,0.));
#25939=DIRECTION('center_axis',(0.,0.,1.));
#25940=DIRECTION('ref_axis',(-1.,0.,0.));
#25941=DIRECTION('',(-0.70710678118655,-8.65956056235496E-17,-0.707106781186545));
#25942=DIRECTION('center_axis',(0.,0.,-1.));
#25943=DIRECTION('ref_axis',(-1.,0.,0.));
#25944=DIRECTION('center_axis',(0.,0.,-1.));
#25945=DIRECTION('ref_axis',(-1.,0.,0.));
#25946=DIRECTION('center_axis',(0.,0.,1.));
#25947=DIRECTION('ref_axis',(1.,0.,0.));
#25948=DIRECTION('center_axis',(0.,0.,1.));
#25949=DIRECTION('ref_axis',(1.,0.,0.));
#25950=DIRECTION('',(0.,0.,1.));
#25951=DIRECTION('center_axis',(0.,0.,1.));
#25952=DIRECTION('ref_axis',(-1.,0.,0.));
#25953=DIRECTION('',(-0.70710678118655,-8.65956056235496E-17,-0.707106781186545));
#25954=DIRECTION('center_axis',(0.,0.,-1.));
#25955=DIRECTION('ref_axis',(-1.,0.,0.));
#25956=DIRECTION('center_axis',(0.,0.,-1.));
#25957=DIRECTION('ref_axis',(-1.,0.,0.));
#25958=DIRECTION('center_axis',(0.,0.,1.));
#25959=DIRECTION('ref_axis',(1.,0.,0.));
#25960=DIRECTION('center_axis',(0.,0.,1.));
#25961=DIRECTION('ref_axis',(1.,0.,0.));
#25962=DIRECTION('',(0.,0.,1.));
#25963=DIRECTION('center_axis',(0.,0.,1.));
#25964=DIRECTION('ref_axis',(-1.,0.,0.));
#25965=DIRECTION('',(-0.70710678118655,-8.65956056235496E-17,-0.707106781186545));
#25966=DIRECTION('center_axis',(0.,0.,-1.));
#25967=DIRECTION('ref_axis',(-1.,0.,0.));
#25968=DIRECTION('center_axis',(0.,0.,-1.));
#25969=DIRECTION('ref_axis',(-1.,0.,0.));
#25970=DIRECTION('center_axis',(0.,0.,1.));
#25971=DIRECTION('ref_axis',(1.,0.,0.));
#25972=DIRECTION('center_axis',(0.,0.,1.));
#25973=DIRECTION('ref_axis',(1.,0.,0.));
#25974=DIRECTION('',(0.,0.,1.));
#25975=DIRECTION('center_axis',(0.,0.,1.));
#25976=DIRECTION('ref_axis',(-1.,0.,0.));
#25977=DIRECTION('',(-0.70710678118655,-8.65956056235496E-17,-0.707106781186545));
#25978=DIRECTION('center_axis',(0.,0.,-1.));
#25979=DIRECTION('ref_axis',(-1.,0.,0.));
#25980=DIRECTION('center_axis',(0.,0.,-1.));
#25981=DIRECTION('ref_axis',(-1.,0.,0.));
#25982=DIRECTION('center_axis',(0.,0.,1.));
#25983=DIRECTION('ref_axis',(1.,0.,0.));
#25984=DIRECTION('center_axis',(0.,0.,1.));
#25985=DIRECTION('ref_axis',(1.,0.,0.));
#25986=DIRECTION('',(0.,0.,1.));
#25987=DIRECTION('center_axis',(0.,0.,-1.));
#25988=DIRECTION('ref_axis',(1.,0.,0.));
#25989=DIRECTION('',(0.707106781186545,-8.6595605623549E-17,0.70710678118655));
#25990=DIRECTION('center_axis',(0.,0.,1.));
#25991=DIRECTION('ref_axis',(1.,0.,0.));
#25992=DIRECTION('center_axis',(0.,0.,1.));
#25993=DIRECTION('ref_axis',(1.,0.,0.));
#25994=DIRECTION('center_axis',(0.,0.,-1.));
#25995=DIRECTION('ref_axis',(-1.,0.,0.));
#25996=DIRECTION('center_axis',(0.,0.,-1.));
#25997=DIRECTION('ref_axis',(1.,0.,0.));
#25998=DIRECTION('',(0.,0.,-1.));
#25999=DIRECTION('center_axis',(0.,0.,-1.));
#26000=DIRECTION('ref_axis',(1.,0.,0.));
#26001=DIRECTION('',(0.707106781186548,-8.65956056235494E-17,0.707106781186547));
#26002=DIRECTION('center_axis',(0.,0.,1.));
#26003=DIRECTION('ref_axis',(1.,0.,0.));
#26004=DIRECTION('center_axis',(0.,0.,1.));
#26005=DIRECTION('ref_axis',(1.,0.,0.));
#26006=DIRECTION('center_axis',(0.,0.,-1.));
#26007=DIRECTION('ref_axis',(-1.,0.,0.));
#26008=DIRECTION('center_axis',(0.,0.,-1.));
#26009=DIRECTION('ref_axis',(1.,0.,0.));
#26010=DIRECTION('',(0.,0.,-1.));
#26011=DIRECTION('center_axis',(0.,0.,-1.));
#26012=DIRECTION('ref_axis',(1.,0.,0.));
#26013=DIRECTION('',(0.70710678118655,-8.65956056235497E-17,0.707106781186545));
#26014=DIRECTION('center_axis',(0.,0.,1.));
#26015=DIRECTION('ref_axis',(1.,0.,0.));
#26016=DIRECTION('center_axis',(0.,0.,1.));
#26017=DIRECTION('ref_axis',(1.,0.,0.));
#26018=DIRECTION('center_axis',(0.,0.,-1.));
#26019=DIRECTION('ref_axis',(-1.,0.,0.));
#26020=DIRECTION('center_axis',(0.,0.,-1.));
#26021=DIRECTION('ref_axis',(1.,0.,0.));
#26022=DIRECTION('',(0.,0.,-1.));
#26023=DIRECTION('center_axis',(0.,0.,1.));
#26024=DIRECTION('ref_axis',(-1.,0.,0.));
#26025=DIRECTION('',(-0.316227766016832,3.87267321454032E-17,-0.948683298050516));
#26026=DIRECTION('center_axis',(0.,0.,-1.));
#26027=DIRECTION('ref_axis',(1.,0.,0.));
#26028=DIRECTION('center_axis',(0.,0.,-1.));
#26029=DIRECTION('ref_axis',(-1.,0.,0.));
#26030=DIRECTION('',(0.,0.,-1.));
#26031=DIRECTION('center_axis',(0.,0.,-1.));
#26032=DIRECTION('ref_axis',(1.,0.,0.));
#26033=DIRECTION('center_axis',(0.,0.,-1.));
#26034=DIRECTION('ref_axis',(-1.,0.,0.));
#26035=DIRECTION('',(0.707106781186541,-8.65956056235486E-17,-0.707106781186554));
#26036=DIRECTION('center_axis',(0.,0.,-1.));
#26037=DIRECTION('ref_axis',(1.,0.,0.));
#26038=DIRECTION('center_axis',(0.,0.,1.));
#26039=DIRECTION('ref_axis',(1.,0.,0.));
#26040=DIRECTION('center_axis',(0.,0.,1.));
#26041=DIRECTION('ref_axis',(-1.,0.,0.));
#26042=DIRECTION('',(-0.316227766016838,3.87267321454038E-17,-0.948683298050514));
#26043=DIRECTION('center_axis',(0.,0.,-1.));
#26044=DIRECTION('ref_axis',(1.,0.,0.));
#26045=DIRECTION('center_axis',(0.,0.,-1.));
#26046=DIRECTION('ref_axis',(-1.,0.,0.));
#26047=DIRECTION('',(0.,0.,-1.));
#26048=DIRECTION('center_axis',(0.,0.,-1.));
#26049=DIRECTION('ref_axis',(1.,0.,0.));
#26050=DIRECTION('center_axis',(0.,0.,-1.));
#26051=DIRECTION('ref_axis',(-1.,0.,0.));
#26052=DIRECTION('',(0.707106781186548,-8.65956056235494E-17,-0.707106781186547));
#26053=DIRECTION('center_axis',(0.,0.,-1.));
#26054=DIRECTION('ref_axis',(1.,0.,0.));
#26055=DIRECTION('center_axis',(0.,0.,1.));
#26056=DIRECTION('ref_axis',(1.,0.,0.));
#26057=DIRECTION('center_axis',(0.,0.,1.));
#26058=DIRECTION('ref_axis',(-1.,0.,0.));
#26059=DIRECTION('',(-0.316227766016832,3.87267321454032E-17,-0.948683298050516));
#26060=DIRECTION('center_axis',(0.,0.,-1.));
#26061=DIRECTION('ref_axis',(1.,0.,0.));
#26062=DIRECTION('center_axis',(0.,0.,-1.));
#26063=DIRECTION('ref_axis',(-1.,0.,0.));
#26064=DIRECTION('',(0.,0.,-1.));
#26065=DIRECTION('center_axis',(0.,0.,-1.));
#26066=DIRECTION('ref_axis',(1.,0.,0.));
#26067=DIRECTION('center_axis',(0.,0.,-1.));
#26068=DIRECTION('ref_axis',(-1.,0.,0.));
#26069=DIRECTION('',(0.707106781186541,-8.65956056235486E-17,-0.707106781186554));
#26070=DIRECTION('center_axis',(0.,0.,-1.));
#26071=DIRECTION('ref_axis',(1.,0.,0.));
#26072=DIRECTION('center_axis',(0.,0.,1.));
#26073=DIRECTION('ref_axis',(1.,0.,0.));
#26074=DIRECTION('center_axis',(0.,0.,-1.));
#26075=DIRECTION('ref_axis',(1.,0.,0.));
#26076=DIRECTION('',(0.316227766016832,3.87267321454031E-17,0.948683298050516));
#26077=DIRECTION('center_axis',(0.,0.,1.));
#26078=DIRECTION('ref_axis',(1.,0.,0.));
#26079=DIRECTION('center_axis',(0.,0.,1.));
#26080=DIRECTION('ref_axis',(1.,0.,0.));
#26081=DIRECTION('',(0.,0.,1.));
#26082=DIRECTION('center_axis',(0.,0.,1.));
#26083=DIRECTION('ref_axis',(1.,0.,0.));
#26084=DIRECTION('center_axis',(0.,0.,1.));
#26085=DIRECTION('ref_axis',(1.,0.,0.));
#26086=DIRECTION('',(-0.70710678118654,-8.65956056235484E-17,0.707106781186555));
#26087=DIRECTION('center_axis',(0.,0.,1.));
#26088=DIRECTION('ref_axis',(1.,0.,0.));
#26089=DIRECTION('center_axis',(0.,0.,-1.));
#26090=DIRECTION('ref_axis',(-1.,0.,0.));
#26091=DIRECTION('center_axis',(0.,0.,-1.));
#26092=DIRECTION('ref_axis',(1.,0.,0.));
#26093=DIRECTION('',(0.316227766016832,3.87267321454031E-17,0.948683298050516));
#26094=DIRECTION('center_axis',(0.,0.,1.));
#26095=DIRECTION('ref_axis',(1.,0.,0.));
#26096=DIRECTION('center_axis',(0.,0.,1.));
#26097=DIRECTION('ref_axis',(1.,0.,0.));
#26098=DIRECTION('',(0.,0.,1.));
#26099=DIRECTION('center_axis',(0.,0.,1.));
#26100=DIRECTION('ref_axis',(1.,0.,0.));
#26101=DIRECTION('center_axis',(0.,0.,1.));
#26102=DIRECTION('ref_axis',(1.,0.,0.));
#26103=DIRECTION('',(-0.70710678118654,-8.65956056235484E-17,0.707106781186555));
#26104=DIRECTION('center_axis',(0.,0.,1.));
#26105=DIRECTION('ref_axis',(1.,0.,0.));
#26106=DIRECTION('center_axis',(0.,0.,-1.));
#26107=DIRECTION('ref_axis',(-1.,0.,0.));
#26108=DIRECTION('center_axis',(0.,0.,-1.));
#26109=DIRECTION('ref_axis',(1.,0.,0.));
#26110=DIRECTION('',(0.316227766016832,3.87267321454031E-17,0.948683298050516));
#26111=DIRECTION('center_axis',(0.,0.,1.));
#26112=DIRECTION('ref_axis',(1.,0.,0.));
#26113=DIRECTION('center_axis',(0.,0.,1.));
#26114=DIRECTION('ref_axis',(1.,0.,0.));
#26115=DIRECTION('',(0.,0.,1.));
#26116=DIRECTION('center_axis',(0.,0.,1.));
#26117=DIRECTION('ref_axis',(1.,0.,0.));
#26118=DIRECTION('center_axis',(0.,0.,1.));
#26119=DIRECTION('ref_axis',(1.,0.,0.));
#26120=DIRECTION('',(-0.70710678118654,-8.65956056235484E-17,0.707106781186555));
#26121=DIRECTION('center_axis',(0.,0.,1.));
#26122=DIRECTION('ref_axis',(1.,0.,0.));
#26123=DIRECTION('center_axis',(0.,0.,-1.));
#26124=DIRECTION('ref_axis',(-1.,0.,0.));
#26125=DIRECTION('center_axis',(0.,0.,-1.));
#26126=DIRECTION('ref_axis',(1.,0.,0.));
#26127=DIRECTION('',(0.316227766016832,3.87267321454031E-17,0.948683298050516));
#26128=DIRECTION('center_axis',(0.,0.,1.));
#26129=DIRECTION('ref_axis',(1.,0.,0.));
#26130=DIRECTION('center_axis',(0.,0.,1.));
#26131=DIRECTION('ref_axis',(1.,0.,0.));
#26132=DIRECTION('',(0.,0.,1.));
#26133=DIRECTION('center_axis',(0.,0.,1.));
#26134=DIRECTION('ref_axis',(1.,0.,0.));
#26135=DIRECTION('center_axis',(0.,0.,1.));
#26136=DIRECTION('ref_axis',(1.,0.,0.));
#26137=DIRECTION('',(-0.70710678118654,-8.65956056235484E-17,0.707106781186555));
#26138=DIRECTION('center_axis',(0.,0.,1.));
#26139=DIRECTION('ref_axis',(1.,0.,0.));
#26140=DIRECTION('center_axis',(0.,0.,-1.));
#26141=DIRECTION('ref_axis',(-1.,0.,0.));
#26142=DIRECTION('center_axis',(-0.707106781186549,0.,-0.707106781186546));
#26143=DIRECTION('ref_axis',(-0.707106781186546,0.,0.707106781186549));
#26144=DIRECTION('center_axis',(0.,0.,-1.));
#26145=DIRECTION('ref_axis',(0.707106781186548,0.707106781186548,0.));
#26146=DIRECTION('center_axis',(-1.,0.,0.));
#26147=DIRECTION('ref_axis',(0.,-1.,0.));
#26148=DIRECTION('',(0.,0.,1.));
#26149=DIRECTION('center_axis',(0.,0.,1.));
#26150=DIRECTION('ref_axis',(0.707106781186547,0.707106781186547,0.));
#26151=DIRECTION('',(0.,0.,1.));
#26152=DIRECTION('center_axis',(0.,0.,1.));
#26153=DIRECTION('ref_axis',(-0.707106781186547,0.707106781186547,0.));
#26154=DIRECTION('',(0.,0.,-1.));
#26155=DIRECTION('center_axis',(0.,1.,0.));
#26156=DIRECTION('ref_axis',(-1.,0.,0.));
#26157=DIRECTION('axis',(0.,0.,1.));
#26158=DIRECTION('refdir',(1.,0.,0.));
#26159=DIRECTION('center_axis',(0.,-0.923879532511281,-0.382683432365103));
#26160=DIRECTION('ref_axis',(0.,0.382683432365103,-0.923879532511281));
#26161=DIRECTION('',(-1.,0.,0.));
#26162=DIRECTION('',(-0.678598344545856,0.281084637714825,-0.678598344545836));
#26163=DIRECTION('',(1.,0.,0.));
#26164=DIRECTION('',(-0.678598344545858,-0.281084637714826,0.678598344545834));
#26165=DIRECTION('center_axis',(-0.382683432365088,-0.923879532511288,0.));
#26166=DIRECTION('ref_axis',(0.,0.,-1.));
#26167=DIRECTION('',(0.,0.,1.));
#26168=DIRECTION('',(-0.923879532511283,0.3826834323651,0.));
#26169=DIRECTION('',(0.,0.,-1.));
#26170=DIRECTION('center_axis',(0.,1.,0.));
#26171=DIRECTION('ref_axis',(-0.707106781186549,0.,0.707106781186546));
#26172=DIRECTION('',(0.,0.382683432365092,0.923879532511286));
#26173=DIRECTION('center_axis',(-8.70318267579337E-16,-1.,-8.70318267579341E-16));
#26174=DIRECTION('ref_axis',(-0.707106781186549,0.,0.707106781186546));
#26175=DIRECTION('center_axis',(0.,1.,0.));
#26176=DIRECTION('ref_axis',(-0.70710678118655,0.,0.707106781186545));
#26177=DIRECTION('center_axis',(0.,-0.923879532511287,0.382683432365089));
#26178=DIRECTION('ref_axis',(0.,-0.382683432365089,-0.923879532511287));
#26179=DIRECTION('',(0.,0.382683432365109,0.923879532511279));
#26180=DIRECTION('',(-1.,0.,0.));
#26181=DIRECTION('',(1.,0.,0.));
#26182=DIRECTION('center_axis',(0.,1.,0.));
#26183=DIRECTION('ref_axis',(0.707106781186548,0.,0.707106781186548));
#26184=DIRECTION('',(0.923879532511298,0.382683432365064,0.));
#26185=DIRECTION('center_axis',(0.,-1.,0.));
#26186=DIRECTION('ref_axis',(0.707106781186548,0.,0.707106781186548));
#26187=DIRECTION('center_axis',(0.,1.,0.));
#26188=DIRECTION('ref_axis',(0.707106781186547,0.,0.707106781186547));
#26189=DIRECTION('center_axis',(0.382683432365088,-0.923879532511288,0.));
#26190=DIRECTION('ref_axis',(0.,0.,-1.));
#26191=DIRECTION('',(0.,0.,1.));
#26192=DIRECTION('',(0.,0.,-1.));
#26193=DIRECTION('center_axis',(0.,1.,0.));
#26194=DIRECTION('ref_axis',(0.707106781186548,0.,0.707106781186548));
#26195=DIRECTION('',(-0.707106781186548,-0.707106781186548,0.));
#26196=DIRECTION('center_axis',(0.,1.,0.));
#26197=DIRECTION('ref_axis',(0.707106781186548,0.,0.707106781186547));
#26198=DIRECTION('',(0.,-0.70710678118654,-0.707106781186555));
#26199=DIRECTION('center_axis',(0.707106781186548,-0.707106781186548,0.));
#26200=DIRECTION('ref_axis',(0.,0.,-1.));
#26201=DIRECTION('',(0.577350269189625,0.577350269189625,-0.577350269189627));
#26202=DIRECTION('',(0.,0.,-1.));
#26203=DIRECTION('center_axis',(0.,-0.707106781186549,-0.707106781186547));
#26204=DIRECTION('ref_axis',(-1.,0.,0.));
#26205=DIRECTION('',(-0.577350269189624,0.577350269189624,-0.57735026918963));
#26206=DIRECTION('',(-1.,0.,0.));
#26207=DIRECTION('center_axis',(0.,1.,0.));
#26208=DIRECTION('ref_axis',(1.,0.,0.));
#26209=DIRECTION('center_axis',(0.,-1.,0.));
#26210=DIRECTION('ref_axis',(-1.,0.,0.));
#26211=DIRECTION('center_axis',(0.,-1.,0.));
#26212=DIRECTION('ref_axis',(-1.,0.,0.));
#26213=DIRECTION('center_axis',(0.,-1.,0.));
#26214=DIRECTION('ref_axis',(-1.,0.,0.));
#26215=DIRECTION('center_axis',(0.,-1.,0.));
#26216=DIRECTION('ref_axis',(-1.,0.,0.));
#26217=DIRECTION('center_axis',(0.,-1.,0.));
#26218=DIRECTION('ref_axis',(-1.,0.,0.));
#26219=DIRECTION('center_axis',(0.,-1.,0.));
#26220=DIRECTION('ref_axis',(-1.,0.,0.));
#26221=DIRECTION('center_axis',(0.,-1.,0.));
#26222=DIRECTION('ref_axis',(-1.,0.,0.));
#26223=DIRECTION('center_axis',(0.,-0.382683432365092,-0.923879532511286));
#26224=DIRECTION('ref_axis',(-1.,0.,0.));
#26225=DIRECTION('',(-0.357406744336597,-0.862856209461015,0.357406744336595));
#26226=DIRECTION('',(-0.357406744336597,0.862856209461015,-0.357406744336595));
#26227=DIRECTION('',(0.357406744336602,0.862856209461013,-0.357406744336594));
#26228=DIRECTION('',(1.,0.,0.));
#26229=DIRECTION('',(0.357406744336593,-0.862856209461016,0.357406744336595));
#26230=DIRECTION('center_axis',(0.,0.,-1.));
#26231=DIRECTION('ref_axis',(-1.,0.,0.));
#26232=DIRECTION('',(0.,-1.,0.));
#26233=DIRECTION('',(-1.,0.,0.));
#26234=DIRECTION('',(0.,1.,0.));
#26235=DIRECTION('center_axis',(0.,0.,1.));
#26236=DIRECTION('ref_axis',(-1.,0.,0.));
#26237=DIRECTION('center_axis',(0.,0.,1.));
#26238=DIRECTION('ref_axis',(-1.,0.,0.));
#26239=DIRECTION('center_axis',(0.,0.,1.));
#26240=DIRECTION('ref_axis',(-1.,0.,0.));
#26241=DIRECTION('center_axis',(-0.70710678118654,0.,-0.707106781186555));
#26242=DIRECTION('ref_axis',(-0.707106781186555,0.,0.70710678118654));
#26243=DIRECTION('',(0.357406744336598,-0.862856209461016,-0.35740674433659));
#26244=DIRECTION('',(0.,1.,0.));
#26245=DIRECTION('',(0.3574067443366,0.862856209461015,-0.357406744336592));
#26246=DIRECTION('',(0.357406744336606,-0.86285620946101,-0.357406744336598));
#26247=DIRECTION('center_axis',(-0.923879532511285,-0.382683432365094,0.));
#26248=DIRECTION('ref_axis',(0.,0.,1.));
#26249=DIRECTION('',(0.,0.,1.));
#26250=DIRECTION('',(0.382683432365092,-0.923879532511286,0.));
#26251=DIRECTION('',(0.,0.,-1.));
#26252=DIRECTION('center_axis',(0.923879532511285,-0.382683432365094,0.));
#26253=DIRECTION('ref_axis',(0.,0.,-1.));
#26254=DIRECTION('',(0.357406744336596,0.862856209461013,0.357406744336599));
#26255=DIRECTION('',(0.,0.,1.));
#26256=DIRECTION('',(-0.382683432365095,-0.923879532511285,0.));
#26257=DIRECTION('center_axis',(0.,1.,0.));
#26258=DIRECTION('ref_axis',(0.707106781186548,0.,0.707106781186547));
#26259=DIRECTION('',(0.,-0.923879532511273,-0.382683432365123));
#26260=DIRECTION('center_axis',(0.,-1.,0.));
#26261=DIRECTION('ref_axis',(0.707106781186548,0.,0.707106781186548));
#26262=DIRECTION('center_axis',(0.,-0.382683432365085,0.923879532511289));
#26263=DIRECTION('ref_axis',(1.,0.,0.));
#26264=DIRECTION('',(0.,-0.92387953251129,-0.382683432365083));
#26265=DIRECTION('',(1.,0.,0.));
#26266=DIRECTION('',(-1.,0.,0.));
#26267=DIRECTION('center_axis',(0.,1.,3.46855248302154E-14));
#26268=DIRECTION('ref_axis',(-0.70710678118655,0.,0.707106781186545));
#26269=DIRECTION('center_axis',(-5.42546052537348E-16,1.,-5.42546052537352E-16));
#26270=DIRECTION('ref_axis',(-0.70710678118655,0.,0.707106781186545));
#26271=DIRECTION('center_axis',(0.,-1.,0.));
#26272=DIRECTION('ref_axis',(-0.70710678118655,0.,0.707106781186545));
#26273=DIRECTION('center_axis',(0.,-0.70710678118654,0.707106781186555));
#26274=DIRECTION('ref_axis',(1.,0.,0.));
#26275=DIRECTION('',(0.,-0.707106781186555,-0.70710678118654));
#26276=DIRECTION('center_axis',(0.,1.,0.));
#26277=DIRECTION('ref_axis',(-0.70710678118655,0.,0.707106781186545));
#26278=DIRECTION('',(0.707106781186551,-0.707106781186544,0.));
#26279=DIRECTION('center_axis',(-0.707106781186548,-0.707106781186548,0.));
#26280=DIRECTION('ref_axis',(0.,0.,1.));
#26281=DIRECTION('center_axis',(0.,0.382683432365097,-0.923879532511284));
#26282=DIRECTION('ref_axis',(-1.,0.,0.));
#26283=DIRECTION('',(0.357406744336598,0.86285620946101,0.357406744336605));
#26284=DIRECTION('',(1.,0.,0.));
#26285=DIRECTION('',(0.357406744336598,-0.862856209461011,-0.357406744336602));
#26286=DIRECTION('',(0.357406744336597,0.862856209461013,0.357406744336599));
#26287=DIRECTION('center_axis',(0.70710678118655,0.,-0.707106781186545));
#26288=DIRECTION('ref_axis',(-0.707106781186545,0.,-0.70710678118655));
#26289=DIRECTION('',(0.357406744336599,-0.862856209461011,0.357406744336601));
#26290=DIRECTION('',(0.,-1.,0.));
#26291=DIRECTION('center_axis',(1.,0.,0.));
#26292=DIRECTION('ref_axis',(0.,0.,-1.));
#26293=DIRECTION('',(0.,0.,-1.));
#26294=DIRECTION('',(0.,1.,0.));
#26295=DIRECTION('center_axis',(0.923879532511284,0.382683432365097,0.));
#26296=DIRECTION('ref_axis',(0.,0.,-1.));
#26297=DIRECTION('',(0.,0.,1.));
#26298=DIRECTION('',(-0.382683432365099,0.923879532511283,0.));
#26299=DIRECTION('center_axis',(-0.923879532511284,0.382683432365097,0.));
#26300=DIRECTION('ref_axis',(0.,0.,1.));
#26301=DIRECTION('',(0.,0.,1.));
#26302=DIRECTION('',(0.382683432365097,0.923879532511284,0.));
#26303=DIRECTION('',(0.,0.,-1.));
#26304=DIRECTION('center_axis',(0.,-1.,3.46855248302153E-14));
#26305=DIRECTION('ref_axis',(-0.70710678118655,0.,0.707106781186545));
#26306=DIRECTION('',(0.,0.923879532511285,-0.382683432365094));
#26307=DIRECTION('center_axis',(0.,-1.,0.));
#26308=DIRECTION('ref_axis',(-0.70710678118655,0.,0.707106781186545));
#26309=DIRECTION('center_axis',(0.,1.,0.));
#26310=DIRECTION('ref_axis',(-0.70710678118655,0.,0.707106781186545));
#26311=DIRECTION('center_axis',(0.,0.382683432365083,0.92387953251129));
#26312=DIRECTION('ref_axis',(1.,0.,0.));
#26313=DIRECTION('',(0.,0.923879532511292,-0.382683432365077));
#26314=DIRECTION('',(-1.,0.,0.));
#26315=DIRECTION('',(1.,0.,0.));
#26316=DIRECTION('center_axis',(0.,-1.,0.));
#26317=DIRECTION('ref_axis',(0.707106781186548,0.,0.707106781186547));
#26318=DIRECTION('center_axis',(0.,-1.,0.));
#26319=DIRECTION('ref_axis',(0.707106781186549,0.,0.707106781186546));
#26320=DIRECTION('center_axis',(0.,1.,0.));
#26321=DIRECTION('ref_axis',(0.707106781186547,0.,0.707106781186547));
#26322=DIRECTION('center_axis',(0.,-1.,0.));
#26323=DIRECTION('ref_axis',(0.707106781186548,0.,0.707106781186548));
#26324=DIRECTION('',(-0.707106781186551,0.707106781186544,0.));
#26325=DIRECTION('center_axis',(0.,1.,0.));
#26326=DIRECTION('ref_axis',(0.707106781186548,0.,0.707106781186548));
#26327=DIRECTION('',(0.,0.707106781186555,-0.70710678118654));
#26328=DIRECTION('center_axis',(0.707106781186548,0.707106781186548,0.));
#26329=DIRECTION('ref_axis',(0.,0.,-1.));
#26330=DIRECTION('',(0.577350269189623,-0.577350269189623,-0.577350269189631));
#26331=DIRECTION('',(0.,0.,-1.));
#26332=DIRECTION('center_axis',(0.,0.707106781186549,-0.707106781186547));
#26333=DIRECTION('ref_axis',(-1.,0.,0.));
#26334=DIRECTION('',(-0.577350269189619,-0.577350269189626,-0.577350269189632));
#26335=DIRECTION('',(-1.,0.,0.));
#26336=DIRECTION('center_axis',(0.,1.,0.));
#26337=DIRECTION('ref_axis',(-0.70710678118655,0.,0.707106781186545));
#26338=DIRECTION('',(0.,1.,0.));
#26339=DIRECTION('',(0.,-1.,0.));
#26340=DIRECTION('center_axis',(-1.,0.,0.));
#26341=DIRECTION('ref_axis',(0.,0.,1.));
#26342=DIRECTION('center_axis',(0.,0.923879532511284,-0.382683432365097));
#26343=DIRECTION('ref_axis',(0.,0.382683432365097,0.923879532511284));
#26344=DIRECTION('',(1.,0.,0.));
#26345=DIRECTION('',(0.678598344545853,-0.281084637714818,-0.678598344545842));
#26346=DIRECTION('',(0.678598344545855,0.281084637714819,0.67859834454584));
#26347=DIRECTION('center_axis',(0.382683432365084,0.923879532511289,0.));
#26348=DIRECTION('ref_axis',(0.,0.,1.));
#26349=DIRECTION('',(0.,0.,1.));
#26350=DIRECTION('',(0.923879532511284,-0.382683432365097,0.));
#26351=DIRECTION('center_axis',(0.,-1.,0.));
#26352=DIRECTION('ref_axis',(0.707106781186547,0.,0.707106781186547));
#26353=DIRECTION('',(0.,-0.382683432365037,0.923879532511308));
#26354=DIRECTION('center_axis',(0.,-1.,0.));
#26355=DIRECTION('ref_axis',(0.707106781186548,0.,0.707106781186548));
#26356=DIRECTION('center_axis',(0.,0.923879532511289,0.382683432365085));
#26357=DIRECTION('ref_axis',(0.,-0.382683432365085,0.923879532511289));
#26358=DIRECTION('',(0.,-0.382683432365106,0.92387953251128));
#26359=DIRECTION('',(1.,0.,0.));
#26360=DIRECTION('',(-1.,0.,0.));
#26361=DIRECTION('center_axis',(0.,-1.,0.));
#26362=DIRECTION('ref_axis',(-0.707106781186549,0.,0.707106781186546));
#26363=DIRECTION('',(-0.923879532511289,-0.382683432365085,0.));
#26364=DIRECTION('center_axis',(5.80212178386225E-16,1.,5.80212178386227E-16));
#26365=DIRECTION('ref_axis',(-0.707106781186549,0.,0.707106781186546));
#26366=DIRECTION('center_axis',(0.,-1.,0.));
#26367=DIRECTION('ref_axis',(-0.70710678118655,0.,0.707106781186545));
#26368=DIRECTION('center_axis',(-0.382683432365084,0.923879532511289,0.));
#26369=DIRECTION('ref_axis',(0.,0.,1.));
#26370=DIRECTION('',(0.,0.,1.));
#26371=DIRECTION('',(0.,0.,-1.));
#26372=DIRECTION('center_axis',(0.,-1.,0.));
#26373=DIRECTION('ref_axis',(-0.70710678118655,0.,0.707106781186545));
#26374=DIRECTION('',(0.,0.70710678118654,-0.707106781186555));
#26375=DIRECTION('',(0.707106781186548,0.707106781186548,0.));
#26376=DIRECTION('center_axis',(-0.707106781186548,0.707106781186548,0.));
#26377=DIRECTION('ref_axis',(0.,0.,1.));
#26378=DIRECTION('center_axis',(0.,1.,0.));
#26379=DIRECTION('ref_axis',(0.,0.,1.));
#26380=DIRECTION('center_axis',(0.,1.,0.));
#26381=DIRECTION('ref_axis',(1.,0.,0.));
#26382=DIRECTION('center_axis',(0.,1.,0.));
#26383=DIRECTION('ref_axis',(1.,0.,0.));
#26384=DIRECTION('center_axis',(0.,-1.,0.));
#26385=DIRECTION('ref_axis',(-1.,0.,0.));
#26386=DIRECTION('center_axis',(0.,-1.,0.));
#26387=DIRECTION('ref_axis',(-1.,0.,0.));
#26388=DIRECTION('center_axis',(0.,-1.,0.));
#26389=DIRECTION('ref_axis',(-1.,0.,0.));
#26390=DIRECTION('center_axis',(0.,-1.,0.));
#26391=DIRECTION('ref_axis',(-1.,0.,0.));
#26392=DIRECTION('center_axis',(0.,-1.,0.));
#26393=DIRECTION('ref_axis',(-1.,0.,0.));
#26394=DIRECTION('center_axis',(0.,-1.,0.));
#26395=DIRECTION('ref_axis',(-1.,0.,0.));
#26396=DIRECTION('center_axis',(0.,1.,0.));
#26397=DIRECTION('ref_axis',(1.,0.,0.));
#26398=DIRECTION('center_axis',(0.,1.,0.));
#26399=DIRECTION('ref_axis',(1.,0.,0.));
#26400=DIRECTION('center_axis',(0.,-1.,0.));
#26401=DIRECTION('ref_axis',(-1.,0.,0.));
#26402=DIRECTION('',(-0.707106781186545,0.70710678118655,-8.6595605623549E-17));
#26403=DIRECTION('center_axis',(0.,1.,0.));
#26404=DIRECTION('ref_axis',(-1.,0.,0.));
#26405=DIRECTION('center_axis',(0.,1.,0.));
#26406=DIRECTION('ref_axis',(-1.,0.,0.));
#26407=DIRECTION('',(0.,1.,0.));
#26408=DIRECTION('center_axis',(0.,-1.,0.));
#26409=DIRECTION('ref_axis',(-1.,0.,0.));
#26410=DIRECTION('center_axis',(0.,1.,0.));
#26411=DIRECTION('ref_axis',(1.,0.,0.));
#26412=DIRECTION('',(0.707106781186548,-0.707106781186548,-8.65956056235493E-17));
#26413=DIRECTION('center_axis',(0.,-1.,0.));
#26414=DIRECTION('ref_axis',(1.,0.,0.));
#26415=DIRECTION('center_axis',(0.,-1.,0.));
#26416=DIRECTION('ref_axis',(1.,0.,0.));
#26417=DIRECTION('center_axis',(0.,1.,0.));
#26418=DIRECTION('ref_axis',(-1.,0.,0.));
#26419=DIRECTION('center_axis',(0.,1.,0.));
#26420=DIRECTION('ref_axis',(1.,0.,0.));
#26421=DIRECTION('',(0.,1.,0.));
#26422=DIRECTION('center_axis',(0.,1.,0.));
#26423=DIRECTION('ref_axis',(-1.,0.,0.));
#26424=DIRECTION('',(0.707106781186545,0.70710678118655,8.6595605623549E-17));
#26425=DIRECTION('center_axis',(0.,1.,0.));
#26426=DIRECTION('ref_axis',(-1.,0.,0.));
#26427=DIRECTION('center_axis',(0.,-1.,0.));
#26428=DIRECTION('ref_axis',(0.,0.,-1.));
#26429=DIRECTION('center_axis',(0.,1.,0.));
#26430=DIRECTION('ref_axis',(1.,0.,0.));
#26431=DIRECTION('',(0.707106781186548,-0.707106781186548,-8.65956056235493E-17));
#26432=DIRECTION('center_axis',(0.,-1.,0.));
#26433=DIRECTION('ref_axis',(1.,0.,0.));
#26434=DIRECTION('center_axis',(0.,-1.,0.));
#26435=DIRECTION('ref_axis',(1.,0.,0.));
#26436=DIRECTION('center_axis',(0.,1.,0.));
#26437=DIRECTION('ref_axis',(-1.,0.,0.));
#26438=DIRECTION('center_axis',(0.,1.,0.));
#26439=DIRECTION('ref_axis',(-1.,0.,0.));
#26440=DIRECTION('',(0.,1.,0.));
#26441=DIRECTION('center_axis',(0.,-1.,0.));
#26442=DIRECTION('ref_axis',(-1.,0.,0.));
#26443=DIRECTION('',(-0.707106781186545,0.70710678118655,-8.6595605623549E-17));
#26444=DIRECTION('center_axis',(0.,1.,0.));
#26445=DIRECTION('ref_axis',(1.,0.,0.));
#26446=DIRECTION('',(0.707106781186553,-0.707106781186542,-8.659560562355E-17));
#26447=DIRECTION('center_axis',(0.,-1.,0.));
#26448=DIRECTION('ref_axis',(1.,0.,0.));
#26449=DIRECTION('center_axis',(0.,-1.,0.));
#26450=DIRECTION('ref_axis',(1.,0.,0.));
#26451=DIRECTION('center_axis',(0.,1.,0.));
#26452=DIRECTION('ref_axis',(-1.,0.,0.));
#26453=DIRECTION('center_axis',(0.,1.,0.));
#26454=DIRECTION('ref_axis',(-1.,0.,0.));
#26455=DIRECTION('',(0.,1.,0.));
#26456=DIRECTION('center_axis',(0.,-1.,0.));
#26457=DIRECTION('ref_axis',(-1.,0.,0.));
#26458=DIRECTION('',(-0.70710678118655,0.707106781186545,-8.65956056235496E-17));
#26459=DIRECTION('center_axis',(0.,1.,0.));
#26460=DIRECTION('ref_axis',(1.,0.,0.));
#26461=DIRECTION('',(0.707106781186548,-0.707106781186548,-8.65956056235493E-17));
#26462=DIRECTION('center_axis',(0.,-1.,0.));
#26463=DIRECTION('ref_axis',(1.,0.,0.));
#26464=DIRECTION('center_axis',(0.,-1.,0.));
#26465=DIRECTION('ref_axis',(1.,0.,0.));
#26466=DIRECTION('center_axis',(0.,1.,0.));
#26467=DIRECTION('ref_axis',(-1.,0.,0.));
#26468=DIRECTION('center_axis',(0.,1.,0.));
#26469=DIRECTION('ref_axis',(-1.,0.,0.));
#26470=DIRECTION('',(0.,1.,0.));
#26471=DIRECTION('center_axis',(0.,-1.,0.));
#26472=DIRECTION('ref_axis',(-1.,0.,0.));
#26473=DIRECTION('',(-0.707106781186545,0.70710678118655,-8.6595605623549E-17));
#26474=DIRECTION('center_axis',(0.,-1.,0.));
#26475=DIRECTION('ref_axis',(-1.,0.,0.));
#26476=DIRECTION('',(-0.70710678118655,0.707106781186545,-8.65956056235497E-17));
#26477=DIRECTION('center_axis',(0.,1.,0.));
#26478=DIRECTION('ref_axis',(-1.,0.,0.));
#26479=DIRECTION('center_axis',(0.,1.,0.));
#26480=DIRECTION('ref_axis',(-1.,0.,0.));
#26481=DIRECTION('',(0.,1.,0.));
#26482=DIRECTION('center_axis',(0.,1.,0.));
#26483=DIRECTION('ref_axis',(1.,0.,0.));
#26484=DIRECTION('center_axis',(0.,-1.,0.));
#26485=DIRECTION('ref_axis',(-1.,0.,0.));
#26486=DIRECTION('',(-0.70710678118655,0.707106781186545,-8.65956056235496E-17));
#26487=DIRECTION('center_axis',(0.,1.,0.));
#26488=DIRECTION('ref_axis',(-1.,0.,0.));
#26489=DIRECTION('center_axis',(0.,1.,0.));
#26490=DIRECTION('ref_axis',(-1.,0.,0.));
#26491=DIRECTION('',(0.,1.,0.));
#26492=DIRECTION('center_axis',(0.,1.,0.));
#26493=DIRECTION('ref_axis',(1.,0.,0.));
#26494=DIRECTION('center_axis',(0.,-1.,0.));
#26495=DIRECTION('ref_axis',(-1.,0.,0.));
#26496=DIRECTION('',(-0.707106781186547,0.707106781186548,-8.65956056235492E-17));
#26497=DIRECTION('center_axis',(0.,1.,0.));
#26498=DIRECTION('ref_axis',(-1.,0.,0.));
#26499=DIRECTION('center_axis',(0.,1.,0.));
#26500=DIRECTION('ref_axis',(-1.,0.,0.));
#26501=DIRECTION('',(0.,1.,0.));
#26502=DIRECTION('center_axis',(0.,1.,0.));
#26503=DIRECTION('ref_axis',(1.,0.,0.));
#26504=DIRECTION('center_axis',(0.,0.,1.));
#26505=DIRECTION('ref_axis',(1.,0.,0.));
#26506=DIRECTION('center_axis',(0.,0.,1.));
#26507=DIRECTION('ref_axis',(1.,0.,0.));
#26508=DIRECTION('',(0.923879532511284,1.1314261122877E-16,-0.382683432365096));
#26509=DIRECTION('center_axis',(0.,0.,-1.));
#26510=DIRECTION('ref_axis',(1.,0.,0.));
#26511=DIRECTION('center_axis',(0.,0.,1.));
#26512=DIRECTION('ref_axis',(1.,0.,0.));
#26513=DIRECTION('center_axis',(0.,0.,1.));
#26514=DIRECTION('ref_axis',(-1.,0.,0.));
#26515=DIRECTION('center_axis',(0.,0.,1.));
#26516=DIRECTION('ref_axis',(-1.,0.,0.));
#26517=DIRECTION('',(-0.707106781186543,-8.65956056235488E-17,0.707106781186552));
#26518=DIRECTION('center_axis',(0.,0.,1.));
#26519=DIRECTION('ref_axis',(1.,0.,0.));
#26520=DIRECTION('',(0.,-1.,0.));
#26521=DIRECTION('center_axis',(0.,0.,1.));
#26522=DIRECTION('ref_axis',(-1.,0.,0.));
#26523=DIRECTION('center_axis',(0.,0.,-1.));
#26524=DIRECTION('ref_axis',(-1.,0.,0.));
#26525=DIRECTION('center_axis',(0.,0.,-1.));
#26526=DIRECTION('ref_axis',(-1.,0.,0.));
#26527=DIRECTION('',(0.382683432365085,-4.68652040532624E-17,0.923879532511289));
#26528=DIRECTION('center_axis',(0.,0.,1.));
#26529=DIRECTION('ref_axis',(1.,0.,0.));
#26530=DIRECTION('center_axis',(0.,0.,1.));
#26531=DIRECTION('ref_axis',(1.,0.,0.));
#26532=DIRECTION('',(0.,0.,1.));
#26533=DIRECTION('center_axis',(0.,0.,1.));
#26534=DIRECTION('ref_axis',(1.,0.,0.));
#26535=DIRECTION('',(-0.857167300702113,-1.04972719113862E-16,0.515038074910052));
#26536=DIRECTION('center_axis',(0.,0.,-1.));
#26537=DIRECTION('ref_axis',(-1.,0.,0.));
#26538=DIRECTION('',(0.857167300702112,-1.04972719113862E-16,-0.515038074910054));
#26539=DIRECTION('center_axis',(0.,0.,-1.));
#26540=DIRECTION('ref_axis',(1.,0.,0.));
#26541=DIRECTION('center_axis',(0.,0.,-1.));
#26542=DIRECTION('ref_axis',(-1.,0.,0.));
#26543=DIRECTION('',(0.,0.,-1.));
#26544=DIRECTION('center_axis',(0.,0.,-1.));
#26545=DIRECTION('ref_axis',(1.,0.,0.));
#26546=DIRECTION('center_axis',(0.,0.,-1.));
#26547=DIRECTION('ref_axis',(-1.,0.,0.));
#26548=DIRECTION('',(0.707106781186546,-8.65956056235491E-17,-0.707106781186549));
#26549=DIRECTION('center_axis',(0.,0.,-1.));
#26550=DIRECTION('ref_axis',(-1.,0.,0.));
#26551=DIRECTION('',(0.857167300702112,-1.04972719113862E-16,-0.515038074910054));
#26552=DIRECTION('center_axis',(0.,0.,-1.));
#26553=DIRECTION('ref_axis',(1.,0.,0.));
#26554=DIRECTION('center_axis',(0.,0.,-1.));
#26555=DIRECTION('ref_axis',(-1.,0.,0.));
#26556=DIRECTION('',(0.,0.,-1.));
#26557=DIRECTION('center_axis',(0.,0.,-1.));
#26558=DIRECTION('ref_axis',(1.,0.,0.));
#26559=DIRECTION('center_axis',(0.,0.,-1.));
#26560=DIRECTION('ref_axis',(-1.,0.,0.));
#26561=DIRECTION('',(0.707106781186547,-8.65956056235493E-17,-0.707106781186548));
#26562=DIRECTION('center_axis',(0.,0.,-1.));
#26563=DIRECTION('ref_axis',(-1.,0.,0.));
#26564=DIRECTION('',(0.857167300702112,-1.04972719113862E-16,-0.515038074910054));
#26565=DIRECTION('center_axis',(0.,0.,-1.));
#26566=DIRECTION('ref_axis',(1.,0.,0.));
#26567=DIRECTION('center_axis',(0.,0.,-1.));
#26568=DIRECTION('ref_axis',(-1.,0.,0.));
#26569=DIRECTION('',(0.,0.,-1.));
#26570=DIRECTION('center_axis',(0.,0.,-1.));
#26571=DIRECTION('ref_axis',(1.,0.,0.));
#26572=DIRECTION('center_axis',(0.,0.,-1.));
#26573=DIRECTION('ref_axis',(-1.,0.,0.));
#26574=DIRECTION('',(0.707106781186546,-8.65956056235491E-17,-0.707106781186549));
#26575=DIRECTION('center_axis',(0.,1.,0.));
#26576=DIRECTION('ref_axis',(-1.,0.,0.));
#26577=DIRECTION('',(0.52999894000318,0.847998304005088,-6.49061505426384E-17));
#26578=DIRECTION('center_axis',(0.,1.,0.));
#26579=DIRECTION('ref_axis',(-1.,0.,0.));
#26580=DIRECTION('',(0.529998940003178,0.847998304005089,-6.49061505426383E-17));
#26581=DIRECTION('center_axis',(0.,1.,0.));
#26582=DIRECTION('ref_axis',(-1.,0.,0.));
#26583=DIRECTION('',(0.529998940003178,0.847998304005089,-6.49061505426382E-17));
#26584=DIRECTION('center_axis',(0.,1.,0.));
#26585=DIRECTION('ref_axis',(-1.,0.,0.));
#26586=DIRECTION('',(0.857167300702112,0.515038074910054,-1.04972719113862E-16));
#26587=DIRECTION('center_axis',(0.,1.,0.));
#26588=DIRECTION('ref_axis',(1.,0.,0.));
#26589=DIRECTION('center_axis',(0.,1.,0.));
#26590=DIRECTION('ref_axis',(-1.,0.,0.));
#26591=DIRECTION('',(0.,1.,0.));
#26592=DIRECTION('center_axis',(0.,1.,0.));
#26593=DIRECTION('ref_axis',(1.,0.,0.));
#26594=DIRECTION('center_axis',(0.,1.,0.));
#26595=DIRECTION('ref_axis',(-1.,0.,0.));
#26596=DIRECTION('',(0.707106781186548,0.707106781186547,-8.65956056235493E-17));
#26597=DIRECTION('center_axis',(0.,1.,0.));
#26598=DIRECTION('ref_axis',(-1.,0.,0.));
#26599=DIRECTION('',(0.857167300702112,0.515038074910054,-1.04972719113862E-16));
#26600=DIRECTION('center_axis',(0.,1.,0.));
#26601=DIRECTION('ref_axis',(1.,0.,0.));
#26602=DIRECTION('center_axis',(0.,1.,0.));
#26603=DIRECTION('ref_axis',(-1.,0.,0.));
#26604=DIRECTION('',(0.,1.,0.));
#26605=DIRECTION('center_axis',(0.,1.,0.));
#26606=DIRECTION('ref_axis',(1.,0.,0.));
#26607=DIRECTION('center_axis',(0.,1.,0.));
#26608=DIRECTION('ref_axis',(-1.,0.,0.));
#26609=DIRECTION('',(0.707106781186548,0.707106781186547,-8.65956056235493E-17));
#26610=DIRECTION('center_axis',(0.,1.,0.));
#26611=DIRECTION('ref_axis',(-1.,0.,0.));
#26612=DIRECTION('',(0.857167300702112,0.515038074910054,-1.04972719113862E-16));
#26613=DIRECTION('center_axis',(0.,1.,0.));
#26614=DIRECTION('ref_axis',(1.,0.,0.));
#26615=DIRECTION('center_axis',(0.,1.,0.));
#26616=DIRECTION('ref_axis',(-1.,0.,0.));
#26617=DIRECTION('',(0.,1.,0.));
#26618=DIRECTION('center_axis',(0.,1.,0.));
#26619=DIRECTION('ref_axis',(1.,0.,0.));
#26620=DIRECTION('center_axis',(0.,1.,0.));
#26621=DIRECTION('ref_axis',(-1.,0.,0.));
#26622=DIRECTION('',(0.707106781186546,0.707106781186549,-8.65956056235491E-17));
#26623=DIRECTION('center_axis',(0.,0.70710678118654,0.707106781186555));
#26624=DIRECTION('ref_axis',(1.,0.,0.));
#26625=DIRECTION('center_axis',(0.,1.,0.));
#26626=DIRECTION('ref_axis',(0.707106781186547,0.,0.707106781186547));
#26627=DIRECTION('axis',(0.,0.,1.));
#26628=DIRECTION('refdir',(1.,0.,0.));
#26629=DIRECTION('center_axis',(0.,1.,0.));
#26630=DIRECTION('ref_axis',(0.707106781186546,0.,0.707106781186549));
#26631=DIRECTION('',(0.923879532511281,0.382683432365105,0.));
#26632=DIRECTION('center_axis',(-1.16042435677245E-15,-1.,1.16042435677245E-15));
#26633=DIRECTION('ref_axis',(0.707106781186546,0.,0.707106781186549));
#26634=DIRECTION('',(1.60226232325242E-14,-0.382683432365069,-0.923879532511295));
#26635=DIRECTION('center_axis',(0.,1.,0.));
#26636=DIRECTION('ref_axis',(0.707106781186546,0.,0.707106781186549));
#26637=DIRECTION('center_axis',(0.382683432365084,-0.923879532511289,0.));
#26638=DIRECTION('ref_axis',(0.,0.,-1.));
#26639=DIRECTION('',(0.923879532511289,0.382683432365084,0.));
#26640=DIRECTION('',(0.,0.,1.));
#26641=DIRECTION('',(0.,0.,-1.));
#26642=DIRECTION('center_axis',(0.,1.,0.));
#26643=DIRECTION('ref_axis',(0.707106781186548,0.,-0.707106781186547));
#26644=DIRECTION('',(0.,0.382683432365101,-0.923879532511282));
#26645=DIRECTION('center_axis',(0.,-1.,0.));
#26646=DIRECTION('ref_axis',(0.707106781186548,0.,-0.707106781186547));
#26647=DIRECTION('center_axis',(0.,1.,0.));
#26648=DIRECTION('ref_axis',(0.707106781186548,0.,-0.707106781186548));
#26649=DIRECTION('center_axis',(0.,-0.923879532511291,-0.38268343236508));
#26650=DIRECTION('ref_axis',(0.,0.38268343236508,-0.923879532511291));
#26651=DIRECTION('',(0.,0.38268343236509,-0.923879532511287));
#26652=DIRECTION('',(1.,0.,0.));
#26653=DIRECTION('',(-1.,0.,0.));
#26654=DIRECTION('center_axis',(0.,1.,0.));
#26655=DIRECTION('ref_axis',(-0.707106781186548,0.,-0.707106781186547));
#26656=DIRECTION('',(-0.923879532511284,0.382683432365097,0.));
#26657=DIRECTION('center_axis',(0.,-1.,0.));
#26658=DIRECTION('ref_axis',(-0.707106781186548,0.,-0.707106781186547));
#26659=DIRECTION('center_axis',(0.,1.,0.));
#26660=DIRECTION('ref_axis',(-0.707106781186548,0.,-0.707106781186548));
#26661=DIRECTION('center_axis',(-0.382683432365084,-0.923879532511289,0.));
#26662=DIRECTION('ref_axis',(0.,0.,-1.));
#26663=DIRECTION('',(-0.923879532511289,0.382683432365084,0.));
#26664=DIRECTION('',(0.,0.,-1.));
#26665=DIRECTION('',(0.,0.,1.));
#26666=DIRECTION('center_axis',(0.,1.,0.));
#26667=DIRECTION('ref_axis',(-0.707106781186549,0.,0.707106781186547));
#26668=DIRECTION('',(0.,0.382683432365085,0.923879532511289));
#26669=DIRECTION('center_axis',(0.,-1.,0.));
#26670=DIRECTION('ref_axis',(-0.707106781186548,0.,0.707106781186547));
#26671=DIRECTION('center_axis',(0.,1.,0.));
#26672=DIRECTION('ref_axis',(-0.707106781186548,0.,0.707106781186547));
#26673=DIRECTION('center_axis',(0.,-0.92387953251129,0.382683432365083));
#26674=DIRECTION('ref_axis',(0.,-0.382683432365083,-0.92387953251129));
#26675=DIRECTION('',(-1.,0.,0.));
#26676=DIRECTION('',(1.,0.,0.));
#26677=DIRECTION('center_axis',(-0.707106781186548,-0.707106781186548,0.));
#26678=DIRECTION('ref_axis',(0.,0.,1.));
#26679=DIRECTION('',(-0.707106781186548,0.707106781186548,0.));
#26680=DIRECTION('',(0.,0.,1.));
#26681=DIRECTION('',(-0.707106781186548,0.707106781186548,0.));
#26682=DIRECTION('center_axis',(0.,1.,0.));
#26683=DIRECTION('ref_axis',(-0.707106781186548,0.,0.707106781186546));
#26684=DIRECTION('',(0.,0.707106781186548,0.707106781186548));
#26685=DIRECTION('center_axis',(0.,1.,0.));
#26686=DIRECTION('ref_axis',(-0.707106781186547,0.,0.707106781186547));
#26687=DIRECTION('center_axis',(0.,-0.707106781186548,0.707106781186548));
#26688=DIRECTION('ref_axis',(1.,0.,0.));
#26689=DIRECTION('',(0.,-0.707106781186548,-0.707106781186548));
#26690=DIRECTION('',(1.,0.,0.));
#26691=DIRECTION('center_axis',(0.,1.,0.));
#26692=DIRECTION('ref_axis',(0.707106781186546,0.,0.707106781186549));
#26693=DIRECTION('',(0.707106781186548,0.707106781186548,0.));
#26694=DIRECTION('center_axis',(-1.62763815761205E-15,1.,1.62763815761205E-15));
#26695=DIRECTION('ref_axis',(0.707106781186547,0.,0.707106781186548));
#26696=DIRECTION('center_axis',(0.,1.,0.));
#26697=DIRECTION('ref_axis',(1.,0.,0.));
#26698=DIRECTION('center_axis',(0.,-1.,0.));
#26699=DIRECTION('ref_axis',(-1.,0.,0.));
#26700=DIRECTION('center_axis',(0.,1.,0.));
#26701=DIRECTION('ref_axis',(1.,0.,0.));
#26702=DIRECTION('center_axis',(0.,1.,0.));
#26703=DIRECTION('ref_axis',(1.,0.,0.));
#26704=DIRECTION('center_axis',(0.,1.,0.));
#26705=DIRECTION('ref_axis',(1.,0.,0.));
#26706=DIRECTION('center_axis',(0.,-0.382683432365099,-0.923879532511283));
#26707=DIRECTION('ref_axis',(-1.,0.,0.));
#26708=DIRECTION('',(0.,-0.923879532511286,0.382683432365093));
#26709=DIRECTION('',(-1.,0.,0.));
#26710=DIRECTION('',(0.,0.923879532511286,-0.382683432365093));
#26711=DIRECTION('',(1.,0.,0.));
#26712=DIRECTION('center_axis',(0.,1.,0.));
#26713=DIRECTION('ref_axis',(0.707106781186547,0.,-0.707106781186548));
#26714=DIRECTION('',(-0.382683432365089,-0.923879532511287,0.));
#26715=DIRECTION('center_axis',(0.,1.,0.));
#26716=DIRECTION('ref_axis',(0.707106781186547,0.,-0.707106781186548));
#26717=DIRECTION('center_axis',(0.,-1.,0.));
#26718=DIRECTION('ref_axis',(0.707106781186547,0.,-0.707106781186547));
#26719=DIRECTION('center_axis',(0.923879532511284,-0.382683432365097,0.));
#26720=DIRECTION('ref_axis',(0.,0.,-1.));
#26721=DIRECTION('',(-0.382683432365097,-0.923879532511284,0.));
#26722=DIRECTION('',(0.,0.,-1.));
#26723=DIRECTION('',(0.,0.,1.));
#26724=DIRECTION('center_axis',(0.,1.,0.));
#26725=DIRECTION('ref_axis',(0.707106781186547,0.,0.707106781186549));
#26726=DIRECTION('',(-1.60226232325235E-14,-0.923879532511276,-0.382683432365116));
#26727=DIRECTION('center_axis',(0.,-1.,0.));
#26728=DIRECTION('ref_axis',(0.707106781186546,0.,0.707106781186549));
#26729=DIRECTION('center_axis',(0.,-0.382683432365088,0.923879532511288));
#26730=DIRECTION('ref_axis',(1.,0.,0.));
#26731=DIRECTION('',(0.,-0.923879532511285,-0.382683432365094));
#26732=DIRECTION('',(-1.,0.,0.));
#26733=DIRECTION('center_axis',(0.,1.,0.));
#26734=DIRECTION('ref_axis',(-0.707106781186548,0.,0.707106781186547));
#26735=DIRECTION('',(0.382683432365083,-0.92387953251129,0.));
#26736=DIRECTION('center_axis',(0.,-1.,0.));
#26737=DIRECTION('ref_axis',(-0.707106781186548,0.,0.707106781186546));
#26738=DIRECTION('center_axis',(-0.923879532511284,-0.382683432365097,0.));
#26739=DIRECTION('ref_axis',(0.,0.,1.));
#26740=DIRECTION('',(0.382683432365097,-0.923879532511284,0.));
#26741=DIRECTION('',(0.,0.,-1.));
#26742=DIRECTION('center_axis',(0.,1.,0.));
#26743=DIRECTION('ref_axis',(-0.707106781186547,0.,-0.707106781186548));
#26744=DIRECTION('center_axis',(0.,1.,0.));
#26745=DIRECTION('ref_axis',(-0.707106781186547,0.,-0.707106781186548));
#26746=DIRECTION('center_axis',(0.,-1.,0.));
#26747=DIRECTION('ref_axis',(-0.707106781186547,0.,-0.707106781186547));
#26748=DIRECTION('center_axis',(0.,1.,0.));
#26749=DIRECTION('ref_axis',(0.707106781186546,0.,0.707106781186549));
#26750=DIRECTION('',(0.,1.,0.));
#26751=DIRECTION('center_axis',(0.,1.,0.));
#26752=DIRECTION('ref_axis',(0.707106781186546,0.,0.707106781186549));
#26753=DIRECTION('',(0.,-1.,0.));
#26754=DIRECTION('center_axis',(1.,0.,0.));
#26755=DIRECTION('ref_axis',(0.,0.,-1.));
#26756=DIRECTION('',(0.,-1.,0.));
#26757=DIRECTION('',(0.,0.,-1.));
#26758=DIRECTION('center_axis',(0.,1.,0.));
#26759=DIRECTION('ref_axis',(0.707106781186547,0.,-0.707106781186547));
#26760=DIRECTION('',(0.,1.,0.));
#26761=DIRECTION('center_axis',(0.,1.,0.));
#26762=DIRECTION('ref_axis',(0.707106781186547,0.,-0.707106781186547));
#26763=DIRECTION('center_axis',(0.,0.,-1.));
#26764=DIRECTION('ref_axis',(-1.,0.,0.));
#26765=DIRECTION('',(0.,-1.,0.));
#26766=DIRECTION('',(-1.,0.,0.));
#26767=DIRECTION('center_axis',(0.,1.,0.));
#26768=DIRECTION('ref_axis',(-0.707106781186548,0.,-0.707106781186548));
#26769=DIRECTION('',(0.,0.707106781186548,-0.707106781186548));
#26770=DIRECTION('center_axis',(0.,-0.707106781186548,-0.707106781186548));
#26771=DIRECTION('ref_axis',(-1.,0.,0.));
#26772=DIRECTION('',(0.,0.707106781186548,-0.707106781186548));
#26773=DIRECTION('center_axis',(0.,-1.,0.));
#26774=DIRECTION('ref_axis',(0.707106781186547,0.,0.707106781186549));
#26775=DIRECTION('',(-0.382683432365089,0.923879532511287,0.));
#26776=DIRECTION('center_axis',(1.0850921050747E-15,-1.,-1.0850921050747E-15));
#26777=DIRECTION('ref_axis',(0.707106781186547,0.,0.707106781186548));
#26778=DIRECTION('',(1.60226232325234E-14,-0.923879532511277,0.382683432365113));
#26779=DIRECTION('center_axis',(0.923879532511286,0.382683432365092,0.));
#26780=DIRECTION('ref_axis',(0.,0.,-1.));
#26781=DIRECTION('',(-0.382683432365092,0.923879532511286,0.));
#26782=DIRECTION('',(0.,0.,1.));
#26783=DIRECTION('center_axis',(0.,-1.,0.));
#26784=DIRECTION('ref_axis',(0.707106781186547,0.,-0.707106781186547));
#26785=DIRECTION('',(0.,0.92387953251129,0.382683432365082));
#26786=DIRECTION('center_axis',(0.,-1.,0.));
#26787=DIRECTION('ref_axis',(0.707106781186547,0.,-0.707106781186547));
#26788=DIRECTION('center_axis',(0.,0.382683432365088,-0.923879532511287));
#26789=DIRECTION('ref_axis',(-1.,0.,0.));
#26790=DIRECTION('',(0.,0.923879532511287,0.382683432365088));
#26791=DIRECTION('',(1.,0.,0.));
#26792=DIRECTION('center_axis',(0.,-1.,0.));
#26793=DIRECTION('ref_axis',(-0.707106781186547,0.,-0.707106781186547));
#26794=DIRECTION('',(0.382683432365086,0.923879532511288,0.));
#26795=DIRECTION('center_axis',(0.,-1.,0.));
#26796=DIRECTION('ref_axis',(-0.707106781186547,0.,-0.707106781186547));
#26797=DIRECTION('center_axis',(0.,1.,0.));
#26798=DIRECTION('ref_axis',(-0.707106781186547,0.,-0.707106781186547));
#26799=DIRECTION('center_axis',(-0.923879532511286,0.382683432365092,0.));
#26800=DIRECTION('ref_axis',(0.,0.,1.));
#26801=DIRECTION('',(0.382683432365092,0.923879532511286,0.));
#26802=DIRECTION('',(0.,0.,-1.));
#26803=DIRECTION('',(0.,0.,1.));
#26804=DIRECTION('center_axis',(0.,-1.,0.));
#26805=DIRECTION('ref_axis',(-0.707106781186548,0.,0.707106781186547));
#26806=DIRECTION('',(0.,0.923879532511294,-0.382683432365072));
#26807=DIRECTION('center_axis',(0.,-1.,0.));
#26808=DIRECTION('ref_axis',(-0.707106781186547,0.,0.707106781186547));
#26809=DIRECTION('center_axis',(0.,1.,0.));
#26810=DIRECTION('ref_axis',(-0.707106781186548,0.,0.707106781186546));
#26811=DIRECTION('center_axis',(0.,0.382683432365087,0.923879532511288));
#26812=DIRECTION('ref_axis',(1.,0.,0.));
#26813=DIRECTION('',(-1.,0.,0.));
#26814=DIRECTION('',(1.,0.,0.));
#26815=DIRECTION('center_axis',(-0.707106781186549,0.707106781186547,0.));
#26816=DIRECTION('ref_axis',(0.,0.,1.));
#26817=DIRECTION('',(-0.707106781186548,-0.707106781186548,0.));
#26818=DIRECTION('',(0.,0.,1.));
#26819=DIRECTION('',(-0.707106781186547,-0.707106781186549,0.));
#26820=DIRECTION('center_axis',(0.,-1.,0.));
#26821=DIRECTION('ref_axis',(-0.707106781186548,0.,0.707106781186546));
#26822=DIRECTION('',(0.,-0.707106781186549,0.707106781186547));
#26823=DIRECTION('center_axis',(0.,1.,0.));
#26824=DIRECTION('ref_axis',(-0.707106781186548,0.,0.707106781186547));
#26825=DIRECTION('center_axis',(0.,0.707106781186547,0.707106781186549));
#26826=DIRECTION('ref_axis',(1.,0.,0.));
#26827=DIRECTION('',(0.,-0.707106781186548,0.707106781186548));
#26828=DIRECTION('',(1.,0.,0.));
#26829=DIRECTION('center_axis',(0.,-1.,0.));
#26830=DIRECTION('ref_axis',(0.707106781186546,0.,0.707106781186549));
#26831=DIRECTION('',(-0.707106781186548,0.707106781186548,0.));
#26832=DIRECTION('center_axis',(0.,1.,0.));
#26833=DIRECTION('ref_axis',(0.707106781186546,0.,0.707106781186549));
#26834=DIRECTION('center_axis',(0.,-1.,0.));
#26835=DIRECTION('ref_axis',(-1.,0.,0.));
#26836=DIRECTION('',(-0.707106781186548,0.707106781186548,-8.65956056235493E-17));
#26837=DIRECTION('center_axis',(0.,1.,0.));
#26838=DIRECTION('ref_axis',(-1.,0.,0.));
#26839=DIRECTION('center_axis',(0.,1.,0.));
#26840=DIRECTION('ref_axis',(-1.,0.,0.));
#26841=DIRECTION('center_axis',(0.,-1.,0.));
#26842=DIRECTION('ref_axis',(1.,0.,0.));
#26843=DIRECTION('center_axis',(0.,-1.,0.));
#26844=DIRECTION('ref_axis',(1.,0.,0.));
#26845=DIRECTION('',(0.,-1.,0.));
#26846=DIRECTION('center_axis',(0.,-1.,0.));
#26847=DIRECTION('ref_axis',(0.707106781186546,0.,0.707106781186549));
#26848=DIRECTION('',(0.,-0.382683432365069,0.923879532511295));
#26849=DIRECTION('',(-0.923879532511281,0.382683432365105,-3.20452464650474E-14));
#26850=DIRECTION('center_axis',(0.,-1.,0.));
#26851=DIRECTION('ref_axis',(0.707106781186546,0.,0.707106781186549));
#26852=DIRECTION('center_axis',(0.,0.923879532511288,0.382683432365086));
#26853=DIRECTION('ref_axis',(0.,-0.382683432365086,0.923879532511288));
#26854=DIRECTION('',(0.,-0.382683432365093,0.923879532511285));
#26855=DIRECTION('',(-1.,0.,0.));
#26856=DIRECTION('center_axis',(0.,-1.,0.));
#26857=DIRECTION('ref_axis',(-0.707106781186548,0.,0.707106781186547));
#26858=DIRECTION('',(-0.923879532511289,-0.382683432365085,0.));
#26859=DIRECTION('center_axis',(0.,-1.,0.));
#26860=DIRECTION('ref_axis',(-0.707106781186549,0.,0.707106781186547));
#26861=DIRECTION('center_axis',(-0.382683432365107,0.92387953251128,0.));
#26862=DIRECTION('ref_axis',(0.,0.,1.));
#26863=DIRECTION('',(-0.923879532511281,-0.382683432365103,0.));
#26864=DIRECTION('',(0.,0.,-1.));
#26865=DIRECTION('center_axis',(0.,-1.,0.));
#26866=DIRECTION('ref_axis',(-0.707106781186548,-2.15323663608327E-16,-0.707106781186547));
#26867=DIRECTION('',(0.,-0.382683432365098,-0.923879532511283));
#26868=DIRECTION('center_axis',(0.,1.,-5.80212178386226E-16));
#26869=DIRECTION('ref_axis',(-0.707106781186548,-4.10271965863919E-16,-0.707106781186547));
#26870=DIRECTION('center_axis',(0.,-1.,0.));
#26871=DIRECTION('ref_axis',(-0.707106781186548,0.,-0.707106781186548));
#26872=DIRECTION('center_axis',(0.,0.923879532511284,-0.382683432365097));
#26873=DIRECTION('ref_axis',(0.,0.382683432365097,0.923879532511284));
#26874=DIRECTION('',(0.,-0.382683432365097,-0.923879532511284));
#26875=DIRECTION('',(-1.,0.,0.));
#26876=DIRECTION('',(1.,0.,0.));
#26877=DIRECTION('center_axis',(0.,-1.,0.));
#26878=DIRECTION('ref_axis',(0.707106781186548,0.,-0.707106781186547));
#26879=DIRECTION('',(0.923879532511284,-0.382683432365097,8.01131161626203E-15));
#26880=DIRECTION('center_axis',(-2.90106089193113E-16,1.,-2.90106089193113E-16));
#26881=DIRECTION('ref_axis',(0.707106781186548,0.,-0.707106781186547));
#26882=DIRECTION('center_axis',(0.,-1.,0.));
#26883=DIRECTION('ref_axis',(0.707106781186548,0.,-0.707106781186548));
#26884=DIRECTION('center_axis',(0.382683432365107,0.92387953251128,0.));
#26885=DIRECTION('ref_axis',(0.,0.,1.));
#26886=DIRECTION('',(0.,0.,-1.));
#26887=DIRECTION('',(0.,0.,1.));
#26888=DIRECTION('center_axis',(0.,0.707106781186547,-0.707106781186549));
#26889=DIRECTION('ref_axis',(-1.,0.,0.));
#26890=DIRECTION('',(0.,-0.707106781186548,-0.707106781186548));
#26891=DIRECTION('',(0.,-0.707106781186549,-0.707106781186547));
#26892=DIRECTION('center_axis',(0.,-1.,0.));
#26893=DIRECTION('ref_axis',(0.707106781186548,0.,-0.707106781186548));
#26894=DIRECTION('',(0.707106781186548,-0.707106781186548,0.));
#26895=DIRECTION('center_axis',(0.707106781186549,0.707106781186547,0.));
#26896=DIRECTION('ref_axis',(0.,0.,-1.));
#26897=DIRECTION('center_axis',(0.,1.,0.));
#26898=DIRECTION('ref_axis',(0.,0.,1.));
#26899=DIRECTION('center_axis',(0.,1.,0.));
#26900=DIRECTION('ref_axis',(1.,0.,0.));
#26901=DIRECTION('center_axis',(0.,-1.,0.));
#26902=DIRECTION('ref_axis',(1.,0.,0.));
#26903=DIRECTION('center_axis',(0.,1.,0.));
#26904=DIRECTION('ref_axis',(1.,0.,0.));
#26905=DIRECTION('',(-0.707106781186547,-0.707106781186547,8.65956056235493E-17));
#26906=DIRECTION('center_axis',(0.,-1.,0.));
#26907=DIRECTION('ref_axis',(1.,0.,0.));
#26908=DIRECTION('center_axis',(0.,-1.,0.));
#26909=DIRECTION('ref_axis',(1.,0.,0.));
#26910=DIRECTION('center_axis',(0.,-1.,0.));
#26911=DIRECTION('ref_axis',(1.,0.,0.));
#26912=DIRECTION('',(0.,-1.,0.));
#26913=DIRECTION('center_axis',(0.,1.,0.));
#26914=DIRECTION('ref_axis',(0.,0.,1.));
#26915=DIRECTION('center_axis',(0.,1.,0.));
#26916=DIRECTION('ref_axis',(1.,0.,0.));
#26917=DIRECTION('center_axis',(0.,-1.,0.));
#26918=DIRECTION('ref_axis',(1.,0.,0.));
#26919=DIRECTION('',(-0.923879532511285,0.382683432365093,-1.1314261122877E-16));
#26920=DIRECTION('center_axis',(0.,1.,0.));
#26921=DIRECTION('ref_axis',(1.,0.,0.));
#26922=DIRECTION('',(0.707106781186546,-0.707106781186549,-8.65956056235491E-17));
#26923=DIRECTION('center_axis',(0.,1.,6.68564742231361E-17));
#26924=DIRECTION('ref_axis',(1.,0.,0.));
#26925=DIRECTION('center_axis',(0.,1.,0.));
#26926=DIRECTION('ref_axis',(1.,0.,0.));
#26927=DIRECTION('',(0.382683432365088,-0.923879532511287,-4.68652040532628E-17));
#26928=DIRECTION('center_axis',(0.,-1.,0.));
#26929=DIRECTION('ref_axis',(1.,0.,0.));
#26930=DIRECTION('',(-0.857167300702113,-0.515038074910053,-1.04972719113862E-16));
#26931=DIRECTION('center_axis',(0.,-1.,0.));
#26932=DIRECTION('ref_axis',(1.,0.,0.));
#26933=DIRECTION('center_axis',(0.,-1.,0.));
#26934=DIRECTION('ref_axis',(1.,0.,0.));
#26935=DIRECTION('',(0.,-1.,0.));
#26936=DIRECTION('center_axis',(0.,-1.,0.));
#26937=DIRECTION('ref_axis',(1.,0.,0.));
#26938=DIRECTION('center_axis',(0.,-1.,0.));
#26939=DIRECTION('ref_axis',(1.,0.,0.));
#26940=DIRECTION('',(-0.707106781186547,-0.707106781186548,-8.65956056235493E-17));
#26941=DIRECTION('center_axis',(0.,-1.,0.));
#26942=DIRECTION('ref_axis',(1.,0.,0.));
#26943=DIRECTION('',(-0.857167300702113,-0.515038074910053,-1.04972719113862E-16));
#26944=DIRECTION('center_axis',(0.,-1.,0.));
#26945=DIRECTION('ref_axis',(1.,0.,0.));
#26946=DIRECTION('center_axis',(0.,-1.,0.));
#26947=DIRECTION('ref_axis',(1.,0.,0.));
#26948=DIRECTION('',(0.,-1.,0.));
#26949=DIRECTION('center_axis',(0.,-1.,0.));
#26950=DIRECTION('ref_axis',(1.,0.,0.));
#26951=DIRECTION('center_axis',(0.,-1.,0.));
#26952=DIRECTION('ref_axis',(1.,0.,0.));
#26953=DIRECTION('',(-0.707106781186546,-0.707106781186549,-8.65956056235491E-17));
#26954=DIRECTION('center_axis',(0.,-1.,0.));
#26955=DIRECTION('ref_axis',(1.,0.,0.));
#26956=DIRECTION('',(-0.857167300702113,-0.515038074910053,-1.04972719113862E-16));
#26957=DIRECTION('center_axis',(0.,-1.,0.));
#26958=DIRECTION('ref_axis',(1.,0.,0.));
#26959=DIRECTION('center_axis',(0.,-1.,0.));
#26960=DIRECTION('ref_axis',(1.,0.,0.));
#26961=DIRECTION('',(0.,-1.,0.));
#26962=DIRECTION('center_axis',(0.,-1.,0.));
#26963=DIRECTION('ref_axis',(1.,0.,0.));
#26964=DIRECTION('center_axis',(0.,-1.,0.));
#26965=DIRECTION('ref_axis',(1.,0.,0.));
#26966=DIRECTION('',(-0.707106781186546,-0.707106781186549,-8.65956056235491E-17));
#26967=DIRECTION('center_axis',(0.,-1.,0.));
#26968=DIRECTION('ref_axis',(-0.707106781186548,0.,-0.707106781186548));
#26969=DIRECTION('center_axis',(0.707106781186548,-0.707106781186548,0.));
#26970=DIRECTION('ref_axis',(0.,0.,-1.));
#26971=DIRECTION('',(0.707106781186548,0.707106781186548,0.));
#26972=DIRECTION('center_axis',(0.,1.,0.));
#26973=DIRECTION('ref_axis',(0.707106781186548,0.,-0.707106781186548));
#26974=DIRECTION('center_axis',(-1.,0.,0.));
#26975=DIRECTION('ref_axis',(0.,0.,1.));
#26976=DIRECTION('',(0.,-1.,0.));
#26977=DIRECTION('',(0.,1.,0.));
#26978=DIRECTION('center_axis',(0.,1.,0.));
#26979=DIRECTION('ref_axis',(-0.707106781186548,0.,0.707106781186546));
#26980=DIRECTION('',(0.,1.,0.));
#26981=DIRECTION('center_axis',(0.,0.,1.));
#26982=DIRECTION('ref_axis',(1.,0.,0.));
#26983=DIRECTION('center_axis',(0.,1.,0.));
#26984=DIRECTION('ref_axis',(-0.707106781186547,0.,-0.707106781186547));
#26985=DIRECTION('axis',(0.,0.,1.));
#26986=DIRECTION('refdir',(1.,0.,0.));
#26987=DIRECTION('center_axis',(0.,-4.80790650449101E-15,1.));
#26988=DIRECTION('ref_axis',(-1.,3.06971386583218E-17,0.));
#26989=DIRECTION('center_axis',(0.,0.,1.));
#26990=DIRECTION('ref_axis',(-1.,6.12323399573677E-17,0.));
#26991=DIRECTION('',(-0.38268343236511,4.40680849605938E-15,-0.923879532511278));
#26992=DIRECTION('center_axis',(0.,0.,-1.));
#26993=DIRECTION('ref_axis',(-1.,0.,0.));
#26994=DIRECTION('center_axis',(0.,0.,-1.));
#26995=DIRECTION('ref_axis',(-1.,0.,0.));
#26996=DIRECTION('center_axis',(0.,0.,1.));
#26997=DIRECTION('ref_axis',(1.,0.,0.));
#26998=DIRECTION('',(0.,0.,-1.));
#26999=DIRECTION('center_axis',(0.,0.,1.));
#27000=DIRECTION('ref_axis',(-1.,0.,0.));
#27001=DIRECTION('center_axis',(0.,0.,1.));
#27002=DIRECTION('ref_axis',(-1.,0.,0.));
#27003=DIRECTION('center_axis',(0.,0.,1.));
#27004=DIRECTION('ref_axis',(-1.,0.,0.));
#27005=DIRECTION('',(0.707106781186546,-8.65956056235492E-17,0.707106781186549));
#27006=DIRECTION('center_axis',(0.,0.,-1.));
#27007=DIRECTION('ref_axis',(-1.,6.12323399573677E-17,0.));
#27008=DIRECTION('center_axis',(0.,-4.80790650449097E-15,-1.));
#27009=DIRECTION('ref_axis',(-1.,3.06971386583218E-17,0.));
#27010=DIRECTION('center_axis',(0.,0.,-1.));
#27011=DIRECTION('ref_axis',(-1.,6.12323399573677E-17,0.));
#27012=DIRECTION('',(-0.382683432365094,4.5005389041659E-15,0.923879532511285));
#27013=DIRECTION('center_axis',(0.,0.,-1.));
#27014=DIRECTION('ref_axis',(-1.,0.,0.));
#27015=DIRECTION('center_axis',(0.,0.,1.));
#27016=DIRECTION('ref_axis',(-1.,6.12323399573677E-17,0.));
#27017=DIRECTION('',(-0.707106781186546,8.65956056235492E-17,0.707106781186549));
#27018=DIRECTION('center_axis',(0.,1.16291744192215E-14,-1.));
#27019=DIRECTION('ref_axis',(-1.,3.04228054001255E-17,0.));
#27020=DIRECTION('',(0.923879532511283,4.53532798631812E-15,-0.382683432365099));
#27021=DIRECTION('center_axis',(0.,0.,-1.));
#27022=DIRECTION('ref_axis',(-1.,0.,0.));
#27023=DIRECTION('center_axis',(0.,0.,-1.));
#27024=DIRECTION('ref_axis',(-1.,0.,0.));
#27025=DIRECTION('center_axis',(0.,0.,1.));
#27026=DIRECTION('ref_axis',(-1.,0.,0.));
#27027=DIRECTION('center_axis',(0.,0.,1.));
#27028=DIRECTION('ref_axis',(-1.,0.,0.));
#27029=DIRECTION('center_axis',(0.,0.,1.));
#27030=DIRECTION('ref_axis',(-1.,0.,0.));
#27031=DIRECTION('center_axis',(0.,0.,1.));
#27032=DIRECTION('ref_axis',(-1.,0.,0.));
#27033=DIRECTION('center_axis',(0.,1.37722032303527E-14,1.));
#27034=DIRECTION('ref_axis',(-1.,-3.078137037066E-17,0.));
#27035=DIRECTION('center_axis',(0.,0.,-1.));
#27036=DIRECTION('ref_axis',(-1.,-6.12323399573677E-17,0.));
#27037=DIRECTION('',(-0.923879532511289,-5.41197489271776E-15,-0.382683432365086));
#27038=DIRECTION('center_axis',(0.,0.,1.));
#27039=DIRECTION('ref_axis',(-1.,0.,0.));
#27040=DIRECTION('center_axis',(0.,0.,1.));
#27041=DIRECTION('ref_axis',(-1.,-6.12323399573676E-17,0.));
#27042=DIRECTION('',(-0.707106781186546,-8.65956056235491E-17,-0.707106781186549));
#27043=DIRECTION('center_axis',(0.,1.16291744192216E-14,1.));
#27044=DIRECTION('ref_axis',(-1.,3.04228054001255E-17,0.));
#27045=DIRECTION('',(0.923879532511284,4.30904276386059E-15,0.382683432365097));
#27046=DIRECTION('center_axis',(0.,0.,1.));
#27047=DIRECTION('ref_axis',(-1.,0.,0.));
#27048=DIRECTION('center_axis',(0.,0.,1.));
#27049=DIRECTION('ref_axis',(1.,0.,0.));
#27050=DIRECTION('center_axis',(0.,0.,-1.));
#27051=DIRECTION('ref_axis',(-1.,0.,0.));
#27052=DIRECTION('center_axis',(0.,-5.71368862092357E-15,1.));
#27053=DIRECTION('ref_axis',(-1.,-3.05483673377054E-17,0.));
#27054=DIRECTION('',(0.382683432365081,-5.31393482200127E-15,0.923879532511291));
#27055=DIRECTION('center_axis',(0.,0.,-1.));
#27056=DIRECTION('ref_axis',(-1.,0.,0.));
#27057=DIRECTION('center_axis',(0.,0.,-1.));
#27058=DIRECTION('ref_axis',(-1.,0.,0.));
#27059=DIRECTION('center_axis',(0.,0.,1.));
#27060=DIRECTION('ref_axis',(1.,0.,0.));
#27061=DIRECTION('center_axis',(0.,0.,1.));
#27062=DIRECTION('ref_axis',(-1.,0.,0.));
#27063=DIRECTION('center_axis',(0.,0.,1.));
#27064=DIRECTION('ref_axis',(-1.,0.,0.));
#27065=DIRECTION('',(0.,0.,-1.));
#27066=DIRECTION('center_axis',(0.,1.37722032303528E-14,-1.));
#27067=DIRECTION('ref_axis',(-1.,-3.078137037066E-17,0.));
#27068=DIRECTION('center_axis',(0.,0.,1.));
#27069=DIRECTION('ref_axis',(-1.,-6.12323399573677E-17,0.));
#27070=DIRECTION('',(-0.923879532511289,-5.18568967026023E-15,0.382683432365084));
#27071=DIRECTION('center_axis',(0.,0.,-1.));
#27072=DIRECTION('ref_axis',(-1.,0.,0.));
#27073=DIRECTION('',(0.707106781186546,8.65956056235491E-17,-0.707106781186549));
#27074=DIRECTION('center_axis',(0.,0.,-1.));
#27075=DIRECTION('ref_axis',(-1.,-6.12323399573677E-17,0.));
#27076=DIRECTION('center_axis',(0.,-5.71368862092356E-15,-1.));
#27077=DIRECTION('ref_axis',(-1.,-3.05483673377054E-17,0.));
#27078=DIRECTION('',(0.38268343236508,-5.22020441389474E-15,-0.923879532511291));
#27079=DIRECTION('center_axis',(0.,0.,-1.));
#27080=DIRECTION('ref_axis',(-1.,0.,0.));
#27081=DIRECTION('',(0.857167300702112,-1.04972719113862E-16,-0.515038074910055));
#27082=DIRECTION('center_axis',(0.,0.,-1.));
#27083=DIRECTION('ref_axis',(1.,0.,0.));
#27084=DIRECTION('center_axis',(0.,0.,-1.));
#27085=DIRECTION('ref_axis',(-1.,0.,0.));
#27086=DIRECTION('',(0.,0.,-1.));
#27087=DIRECTION('center_axis',(0.,0.,-1.));
#27088=DIRECTION('ref_axis',(1.,0.,0.));
#27089=DIRECTION('center_axis',(0.,0.,-1.));
#27090=DIRECTION('ref_axis',(-1.,0.,0.));
#27091=DIRECTION('',(0.707106781186548,-8.65956056235494E-17,-0.707106781186547));
#27092=DIRECTION('center_axis',(0.,0.,-1.));
#27093=DIRECTION('ref_axis',(-1.,0.,0.));
#27094=DIRECTION('',(0.857167300702111,-1.04972719113862E-16,-0.515038074910056));
#27095=DIRECTION('center_axis',(0.,0.,-1.));
#27096=DIRECTION('ref_axis',(1.,0.,0.));
#27097=DIRECTION('center_axis',(0.,0.,-1.));
#27098=DIRECTION('ref_axis',(-1.,0.,0.));
#27099=DIRECTION('',(0.,0.,-1.));
#27100=DIRECTION('center_axis',(0.,0.,-1.));
#27101=DIRECTION('ref_axis',(1.,0.,0.));
#27102=DIRECTION('center_axis',(0.,0.,-1.));
#27103=DIRECTION('ref_axis',(-1.,0.,0.));
#27104=DIRECTION('',(0.707106781186546,-8.65956056235492E-17,-0.707106781186549));
#27105=DIRECTION('center_axis',(0.,0.,-1.));
#27106=DIRECTION('ref_axis',(-1.,0.,0.));
#27107=DIRECTION('',(0.857167300702112,-1.04972719113862E-16,-0.515038074910055));
#27108=DIRECTION('center_axis',(0.,0.,-1.));
#27109=DIRECTION('ref_axis',(1.,0.,0.));
#27110=DIRECTION('center_axis',(0.,0.,-1.));
#27111=DIRECTION('ref_axis',(-1.,0.,0.));
#27112=DIRECTION('',(0.,0.,-1.));
#27113=DIRECTION('center_axis',(0.,0.,-1.));
#27114=DIRECTION('ref_axis',(1.,0.,0.));
#27115=DIRECTION('center_axis',(0.,0.,-1.));
#27116=DIRECTION('ref_axis',(-1.,0.,0.));
#27117=DIRECTION('',(0.707106781186548,-8.65956056235494E-17,-0.707106781186547));
#27118=DIRECTION('axis',(0.,0.,1.));
#27119=DIRECTION('refdir',(1.,0.,0.));
#27120=DIRECTION('center_axis',(0.,0.,1.));
#27121=DIRECTION('ref_axis',(-1.,0.,0.));
#27122=DIRECTION('center_axis',(0.,0.,1.));
#27123=DIRECTION('ref_axis',(-1.,0.,0.));
#27124=DIRECTION('',(-0.70710678118655,-8.65956056235496E-17,-0.707106781186545));
#27125=DIRECTION('center_axis',(0.,0.,-1.));
#27126=DIRECTION('ref_axis',(-1.,0.,0.));
#27127=DIRECTION('center_axis',(0.,0.,-1.));
#27128=DIRECTION('ref_axis',(-1.,0.,0.));
#27129=DIRECTION('center_axis',(0.,0.,1.));
#27130=DIRECTION('ref_axis',(1.,0.,0.));
#27131=DIRECTION('center_axis',(0.,0.,1.));
#27132=DIRECTION('ref_axis',(1.,0.,0.));
#27133=DIRECTION('',(0.,0.,1.));
#27134=DIRECTION('center_axis',(0.,0.,1.));
#27135=DIRECTION('ref_axis',(1.,0.,0.));
#27136=DIRECTION('center_axis',(0.,0.,-1.));
#27137=DIRECTION('ref_axis',(-1.,0.,0.));
#27138=DIRECTION('center_axis',(0.,0.,1.));
#27139=DIRECTION('ref_axis',(-1.,0.,0.));
#27140=DIRECTION('center_axis',(0.,0.,1.));
#27141=DIRECTION('ref_axis',(-1.,0.,0.));
#27142=DIRECTION('center_axis',(0.,0.,1.));
#27143=DIRECTION('ref_axis',(-1.,0.,0.));
#27144=DIRECTION('center_axis',(0.,0.,1.));
#27145=DIRECTION('ref_axis',(-1.,0.,0.));
#27146=DIRECTION('center_axis',(0.,0.,1.));
#27147=DIRECTION('ref_axis',(-1.,0.,0.));
#27148=DIRECTION('center_axis',(0.,0.,1.));
#27149=DIRECTION('ref_axis',(-1.,0.,0.));
#27150=DIRECTION('center_axis',(0.,0.,-1.));
#27151=DIRECTION('ref_axis',(1.,0.,0.));
#27152=DIRECTION('center_axis',(0.,0.,-1.));
#27153=DIRECTION('ref_axis',(1.,0.,0.));
#27154=DIRECTION('',(0.707106781186551,-8.65956056235497E-17,0.707106781186544));
#27155=DIRECTION('center_axis',(0.,0.,-1.));
#27156=DIRECTION('ref_axis',(-1.,0.,0.));
#27157=DIRECTION('center_axis',(0.,0.,1.));
#27158=DIRECTION('ref_axis',(-1.,0.,0.));
#27159=DIRECTION('center_axis',(0.,0.,-1.));
#27160=DIRECTION('ref_axis',(1.,0.,0.));
#27161=DIRECTION('center_axis',(0.,0.,-1.));
#27162=DIRECTION('ref_axis',(1.,0.,0.));
#27163=DIRECTION('center_axis',(0.,0.,-1.));
#27164=DIRECTION('ref_axis',(1.,0.,0.));
#27165=DIRECTION('center_axis',(0.,0.,-1.));
#27166=DIRECTION('ref_axis',(-1.,0.,0.));
#27167=DIRECTION('center_axis',(0.,0.,-1.));
#27168=DIRECTION('ref_axis',(1.,0.,0.));
#27169=DIRECTION('center_axis',(0.,0.,-1.));
#27170=DIRECTION('ref_axis',(1.,0.,0.));
#27171=DIRECTION('center_axis',(0.,0.,1.));
#27172=DIRECTION('ref_axis',(-1.,0.,0.));
#27173=DIRECTION('',(-0.707106781186545,-8.6595605623549E-17,-0.70710678118655));
#27174=DIRECTION('center_axis',(0.,0.,-1.));
#27175=DIRECTION('ref_axis',(-1.,0.,0.));
#27176=DIRECTION('center_axis',(0.,0.,-1.));
#27177=DIRECTION('ref_axis',(-1.,0.,0.));
#27178=DIRECTION('center_axis',(0.,0.,1.));
#27179=DIRECTION('ref_axis',(1.,0.,0.));
#27180=DIRECTION('center_axis',(0.,0.,1.));
#27181=DIRECTION('ref_axis',(1.,0.,0.));
#27182=DIRECTION('',(0.,0.,1.));
#27183=DIRECTION('center_axis',(0.,0.,-1.));
#27184=DIRECTION('ref_axis',(1.,0.,0.));
#27185=DIRECTION('',(0.707106781186545,-8.65956056235491E-17,0.70710678118655));
#27186=DIRECTION('center_axis',(0.,0.,1.));
#27187=DIRECTION('ref_axis',(-1.,0.,0.));
#27188=DIRECTION('',(-0.707106781186545,-8.6595605623549E-17,-0.70710678118655));
#27189=DIRECTION('center_axis',(0.,0.,-1.));
#27190=DIRECTION('ref_axis',(-1.,0.,0.));
#27191=DIRECTION('center_axis',(0.,0.,-1.));
#27192=DIRECTION('ref_axis',(-1.,0.,0.));
#27193=DIRECTION('center_axis',(0.,0.,1.));
#27194=DIRECTION('ref_axis',(1.,0.,0.));
#27195=DIRECTION('center_axis',(0.,0.,1.));
#27196=DIRECTION('ref_axis',(1.,0.,0.));
#27197=DIRECTION('',(0.,0.,1.));
#27198=DIRECTION('center_axis',(0.,0.,-1.));
#27199=DIRECTION('ref_axis',(1.,0.,0.));
#27200=DIRECTION('',(0.707106781186548,-8.65956056235494E-17,0.707106781186547));
#27201=DIRECTION('center_axis',(0.,0.,1.));
#27202=DIRECTION('ref_axis',(-1.,0.,0.));
#27203=DIRECTION('',(-0.70710678118655,-8.65956056235496E-17,-0.707106781186545));
#27204=DIRECTION('center_axis',(0.,0.,-1.));
#27205=DIRECTION('ref_axis',(-1.,0.,0.));
#27206=DIRECTION('center_axis',(0.,0.,-1.));
#27207=DIRECTION('ref_axis',(-1.,0.,0.));
#27208=DIRECTION('center_axis',(0.,0.,1.));
#27209=DIRECTION('ref_axis',(1.,0.,0.));
#27210=DIRECTION('center_axis',(0.,0.,1.));
#27211=DIRECTION('ref_axis',(1.,0.,0.));
#27212=DIRECTION('',(0.,0.,1.));
#27213=DIRECTION('center_axis',(0.,0.,-1.));
#27214=DIRECTION('ref_axis',(1.,0.,0.));
#27215=DIRECTION('',(0.70710678118655,-8.65956056235497E-17,0.707106781186545));
#27216=DIRECTION('center_axis',(0.,0.,1.));
#27217=DIRECTION('ref_axis',(-1.,0.,0.));
#27218=DIRECTION('',(-0.707106781186545,-8.6595605623549E-17,-0.70710678118655));
#27219=DIRECTION('center_axis',(0.,0.,-1.));
#27220=DIRECTION('ref_axis',(-1.,0.,0.));
#27221=DIRECTION('center_axis',(0.,0.,-1.));
#27222=DIRECTION('ref_axis',(-1.,0.,0.));
#27223=DIRECTION('center_axis',(0.,0.,1.));
#27224=DIRECTION('ref_axis',(1.,0.,0.));
#27225=DIRECTION('center_axis',(0.,0.,1.));
#27226=DIRECTION('ref_axis',(1.,0.,0.));
#27227=DIRECTION('',(0.,0.,1.));
#27228=DIRECTION('center_axis',(0.,0.,-1.));
#27229=DIRECTION('ref_axis',(1.,0.,0.));
#27230=DIRECTION('',(0.707106781186545,-8.65956056235491E-17,0.70710678118655));
#27231=DIRECTION('center_axis',(0.,0.,1.));
#27232=DIRECTION('ref_axis',(-1.,0.,0.));
#27233=DIRECTION('',(-0.707106781186545,-8.6595605623549E-17,-0.70710678118655));
#27234=DIRECTION('center_axis',(0.,0.,-1.));
#27235=DIRECTION('ref_axis',(-1.,0.,0.));
#27236=DIRECTION('center_axis',(0.,0.,-1.));
#27237=DIRECTION('ref_axis',(-1.,0.,0.));
#27238=DIRECTION('center_axis',(0.,0.,1.));
#27239=DIRECTION('ref_axis',(1.,0.,0.));
#27240=DIRECTION('center_axis',(0.,0.,1.));
#27241=DIRECTION('ref_axis',(1.,0.,0.));
#27242=DIRECTION('',(0.,0.,1.));
#27243=DIRECTION('center_axis',(0.,0.,-1.));
#27244=DIRECTION('ref_axis',(1.,0.,0.));
#27245=DIRECTION('',(0.707106781186545,-8.65956056235491E-17,0.70710678118655));
#27246=DIRECTION('center_axis',(0.,0.,-1.));
#27247=DIRECTION('ref_axis',(-1.,0.,0.));
#27248=DIRECTION('',(0.707106781186548,8.65956056235493E-17,-0.707106781186548));
#27249=DIRECTION('center_axis',(0.,0.,1.));
#27250=DIRECTION('ref_axis',(-1.,0.,0.));
#27251=DIRECTION('center_axis',(0.,0.,1.));
#27252=DIRECTION('ref_axis',(-1.,0.,0.));
#27253=DIRECTION('center_axis',(0.,0.,1.));
#27254=DIRECTION('ref_axis',(1.,0.,0.));
#27255=DIRECTION('',(0.,0.,-1.));
#27256=DIRECTION('center_axis',(0.,0.,-1.));
#27257=DIRECTION('ref_axis',(-1.,0.,0.));
#27258=DIRECTION('center_axis',(0.,0.,-1.));
#27259=DIRECTION('ref_axis',(-1.,0.,0.));
#27260=DIRECTION('center_axis',(0.,0.,1.));
#27261=DIRECTION('ref_axis',(-1.,0.,0.));
#27262=DIRECTION('',(-0.707106781186548,-8.65956056235494E-17,-0.707106781186547));
#27263=DIRECTION('center_axis',(0.,0.,-1.));
#27264=DIRECTION('ref_axis',(-1.,0.,0.));
#27265=DIRECTION('',(-0.707106781186548,8.65956056235494E-17,0.707106781186547));
#27266=DIRECTION('center_axis',(0.,0.,1.));
#27267=DIRECTION('ref_axis',(-1.,0.,0.));
#27268=DIRECTION('center_axis',(0.,0.,1.));
#27269=DIRECTION('ref_axis',(-1.,0.,0.));
#27270=DIRECTION('center_axis',(0.,0.,1.));
#27271=DIRECTION('ref_axis',(1.,0.,0.));
#27272=DIRECTION('center_axis',(0.,0.,-1.));
#27273=DIRECTION('ref_axis',(-1.,0.,0.));
#27274=DIRECTION('center_axis',(0.,0.,-1.));
#27275=DIRECTION('ref_axis',(-1.,0.,0.));
#27276=DIRECTION('',(0.,0.,-1.));
#27277=DIRECTION('center_axis',(0.,0.,1.));
#27278=DIRECTION('ref_axis',(-1.,0.,0.));
#27279=DIRECTION('',(0.707106781186548,-8.65956056235493E-17,0.707106781186548));
#27280=DIRECTION('axis',(0.,0.,1.));
#27281=DIRECTION('refdir',(1.,0.,0.));
#27282=DIRECTION('center_axis',(0.,0.,1.));
#27283=DIRECTION('ref_axis',(1.,0.,0.));
#27284=DIRECTION('',(0.,0.,-1.));
#27285=DIRECTION('',(0.,0.,-1.));
#27286=DIRECTION('center_axis',(0.,0.,1.));
#27287=DIRECTION('ref_axis',(1.,0.,0.));
#27288=DIRECTION('center_axis',(0.,0.,-1.));
#27289=DIRECTION('ref_axis',(1.,0.,0.));
#27290=DIRECTION('center_axis',(0.,0.,1.));
#27291=DIRECTION('ref_axis',(1.,0.,0.));
#27292=DIRECTION('',(0.,0.,-1.));
#27293=DIRECTION('center_axis',(0.,0.,1.));
#27294=DIRECTION('ref_axis',(1.,0.,0.));
#27295=DIRECTION('',(0.,0.,-1.));
#27296=DIRECTION('center_axis',(0.,0.,1.));
#27297=DIRECTION('ref_axis',(1.,0.,0.));
#27298=DIRECTION('',(0.,0.,-1.));
#27299=DIRECTION('center_axis',(0.,0.,1.));
#27300=DIRECTION('ref_axis',(1.,0.,0.));
#27301=DIRECTION('',(0.,0.,-1.));
#27302=DIRECTION('center_axis',(0.,0.,1.));
#27303=DIRECTION('ref_axis',(1.,0.,0.));
#27304=DIRECTION('',(0.,0.,-1.));
#27305=DIRECTION('center_axis',(0.,0.,1.));
#27306=DIRECTION('ref_axis',(1.,0.,0.));
#27307=DIRECTION('',(0.,0.,-1.));
#27308=DIRECTION('center_axis',(0.,0.,1.));
#27309=DIRECTION('ref_axis',(1.,0.,0.));
#27310=DIRECTION('',(0.,0.,-1.));
#27311=DIRECTION('center_axis',(0.,0.,1.));
#27312=DIRECTION('ref_axis',(1.,0.,0.));
#27313=DIRECTION('',(0.,0.,-1.));
#27314=DIRECTION('center_axis',(0.,0.,1.));
#27315=DIRECTION('ref_axis',(1.,0.,0.));
#27316=DIRECTION('',(0.,0.,-1.));
#27317=DIRECTION('center_axis',(0.,0.,1.));
#27318=DIRECTION('ref_axis',(1.,5.20993371284765E-14,0.));
#27319=DIRECTION('',(0.,0.,1.));
#27320=DIRECTION('center_axis',(0.,0.,1.));
#27321=DIRECTION('ref_axis',(1.,5.20993371284765E-14,0.));
#27322=DIRECTION('center_axis',(0.,0.,1.));
#27323=DIRECTION('ref_axis',(1.,5.20993371284765E-14,0.));
#27324=DIRECTION('',(0.,0.,1.));
#27325=DIRECTION('center_axis',(0.,0.,1.));
#27326=DIRECTION('ref_axis',(1.,5.20993371284765E-14,0.));
#27327=DIRECTION('',(0.,0.,1.));
#27328=DIRECTION('center_axis',(0.,0.,1.));
#27329=DIRECTION('ref_axis',(1.,5.20993371284765E-14,0.));
#27330=DIRECTION('',(0.,0.,1.));
#27331=DIRECTION('center_axis',(0.,0.,1.));
#27332=DIRECTION('ref_axis',(1.,5.20993371284765E-14,0.));
#27333=DIRECTION('',(0.,0.,1.));
#27334=DIRECTION('center_axis',(0.,0.,1.));
#27335=DIRECTION('ref_axis',(1.,5.20993371284765E-14,0.));
#27336=DIRECTION('',(0.,0.,1.));
#27337=DIRECTION('center_axis',(0.,0.,1.));
#27338=DIRECTION('ref_axis',(1.,5.20993371284765E-14,0.));
#27339=DIRECTION('',(0.,0.,1.));
#27340=DIRECTION('center_axis',(0.,0.,1.));
#27341=DIRECTION('ref_axis',(1.,5.20993371284765E-14,0.));
#27342=DIRECTION('',(0.,0.,1.));
#27343=DIRECTION('center_axis',(0.,0.,1.));
#27344=DIRECTION('ref_axis',(1.,5.20993371284765E-14,0.));
#27345=DIRECTION('',(0.,0.,1.));
#27346=DIRECTION('center_axis',(0.,0.,1.));
#27347=DIRECTION('ref_axis',(1.,5.20993371284765E-14,0.));
#27348=DIRECTION('',(0.,0.,1.));
#27349=DIRECTION('center_axis',(0.,0.,1.));
#27350=DIRECTION('ref_axis',(1.,5.20993371284765E-14,0.));
#27351=DIRECTION('',(0.,0.,1.));
#27352=DIRECTION('center_axis',(0.,0.,1.));
#27353=DIRECTION('ref_axis',(1.,0.,0.));
#27354=DIRECTION('center_axis',(0.,0.,-1.));
#27355=DIRECTION('ref_axis',(1.,5.20993371284765E-14,0.));
#27356=DIRECTION('center_axis',(0.,0.,1.));
#27357=DIRECTION('ref_axis',(0.464898683733536,0.885363887823998,0.));
#27358=DIRECTION('center_axis',(0.,0.,1.));
#27359=DIRECTION('ref_axis',(1.,0.,0.));
#27360=DIRECTION('center_axis',(0.,0.,1.));
#27361=DIRECTION('ref_axis',(1.,0.,0.));
#27362=DIRECTION('',(0.,0.,1.));
#27363=DIRECTION('center_axis',(0.,0.,-1.));
#27364=DIRECTION('ref_axis',(1.,0.,0.));
#27365=DIRECTION('center_axis',(0.,0.,1.));
#27366=DIRECTION('ref_axis',(1.,0.,0.));
#27367=DIRECTION('center_axis',(0.,0.,1.));
#27368=DIRECTION('ref_axis',(1.,0.,0.));
#27369=DIRECTION('',(0.,0.,1.));
#27370=DIRECTION('center_axis',(0.,0.,-1.));
#27371=DIRECTION('ref_axis',(1.,0.,0.));
#27372=DIRECTION('center_axis',(0.,0.,1.));
#27373=DIRECTION('ref_axis',(1.,0.,0.));
#27374=DIRECTION('center_axis',(0.,0.,1.));
#27375=DIRECTION('ref_axis',(1.,0.,0.));
#27376=DIRECTION('',(0.,0.,1.));
#27377=DIRECTION('center_axis',(0.,0.,-1.));
#27378=DIRECTION('ref_axis',(1.,0.,0.));
#27379=DIRECTION('center_axis',(0.,0.,1.));
#27380=DIRECTION('ref_axis',(1.,0.,0.));
#27381=DIRECTION('center_axis',(0.,0.,1.));
#27382=DIRECTION('ref_axis',(1.,0.,0.));
#27383=DIRECTION('',(0.,0.,1.));
#27384=DIRECTION('center_axis',(0.,0.,-1.));
#27385=DIRECTION('ref_axis',(1.,0.,0.));
#27386=DIRECTION('center_axis',(-0.718878223686824,-0.695136029499893,0.));
#27387=DIRECTION('ref_axis',(0.695136029499893,-0.718878223686824,0.));
#27388=DIRECTION('',(0.,0.,1.));
#27389=DIRECTION('',(0.695136029499893,-0.718878223686824,0.));
#27390=DIRECTION('',(0.,0.,1.));
#27391=DIRECTION('',(0.695136029499893,-0.718878223686824,0.));
#27392=DIRECTION('center_axis',(0.,0.,1.));
#27393=DIRECTION('ref_axis',(0.965925826289068,-0.258819045102522,0.));
#27394=DIRECTION('center_axis',(0.,0.,1.));
#27395=DIRECTION('ref_axis',(1.,0.,0.));
#27396=DIRECTION('',(-0.961444572476169,-0.274998789190274,0.));
#27397=DIRECTION('center_axis',(-0.274998789190274,0.961444572476169,0.));
#27398=DIRECTION('ref_axis',(-0.961444572476169,-0.274998789190274,0.));
#27399=DIRECTION('',(0.,0.,-1.));
#27400=DIRECTION('',(-0.961444572476169,-0.274998789190274,0.));
#27401=DIRECTION('center_axis',(0.,0.,1.));
#27402=DIRECTION('ref_axis',(0.965925826289068,-0.258819045102522,0.));
#27403=DIRECTION('center_axis',(0.,0.,-1.));
#27404=DIRECTION('ref_axis',(1.,0.,0.));
#27405=DIRECTION('center_axis',(-0.874297485587433,-0.485390468278367,0.));
#27406=DIRECTION('ref_axis',(0.485390468278367,-0.874297485587433,0.));
#27407=DIRECTION('',(0.,0.,1.));
#27408=DIRECTION('',(0.485390468278367,-0.874297485587433,0.));
#27409=DIRECTION('',(0.,0.,1.));
#27410=DIRECTION('',(0.485390468278367,-0.874297485587433,0.));
#27411=DIRECTION('center_axis',(0.,0.,1.));
#27412=DIRECTION('ref_axis',(0.866025403784438,-0.500000000000001,0.));
#27413=DIRECTION('center_axis',(0.,0.,1.));
#27414=DIRECTION('ref_axis',(1.,0.,0.));
#27415=DIRECTION('',(-0.99985906712276,-0.0167882665098254,0.));
#27416=DIRECTION('center_axis',(-0.0167882665098254,0.99985906712276,0.));
#27417=DIRECTION('ref_axis',(-0.99985906712276,-0.0167882665098254,0.));
#27418=DIRECTION('',(0.,0.,-1.));
#27419=DIRECTION('',(-0.99985906712276,-0.0167882665098254,0.));
#27420=DIRECTION('center_axis',(0.,0.,1.));
#27421=DIRECTION('ref_axis',(0.866025403784438,-0.500000000000001,0.));
#27422=DIRECTION('center_axis',(0.,0.,-1.));
#27423=DIRECTION('ref_axis',(1.,0.,0.));
#27424=DIRECTION('center_axis',(-0.970134818690168,-0.242566348789345,0.));
#27425=DIRECTION('ref_axis',(0.242566348789345,-0.970134818690168,0.));
#27426=DIRECTION('',(0.,0.,1.));
#27427=DIRECTION('',(0.242566348789345,-0.970134818690168,0.));
#27428=DIRECTION('',(0.,0.,1.));
#27429=DIRECTION('',(0.242566348789345,-0.970134818690168,0.));
#27430=DIRECTION('center_axis',(0.,0.,1.));
#27431=DIRECTION('ref_axis',(0.707106781186547,-0.707106781186548,0.));
#27432=DIRECTION('center_axis',(0.,0.,1.));
#27433=DIRECTION('ref_axis',(1.,0.,0.));
#27434=DIRECTION('',(-0.970134818690168,0.242566348789345,0.));
#27435=DIRECTION('center_axis',(0.242566348789345,0.970134818690168,0.));
#27436=DIRECTION('ref_axis',(-0.970134818690168,0.242566348789345,0.));
#27437=DIRECTION('',(0.,0.,-1.));
#27438=DIRECTION('',(-0.970134818690168,0.242566348789345,0.));
#27439=DIRECTION('center_axis',(0.,0.,1.));
#27440=DIRECTION('ref_axis',(0.707106781186547,-0.707106781186548,0.));
#27441=DIRECTION('center_axis',(0.,0.,-1.));
#27442=DIRECTION('ref_axis',(1.,0.,0.));
#27443=DIRECTION('center_axis',(-0.99985906712276,0.0167882665098268,0.));
#27444=DIRECTION('ref_axis',(-0.0167882665098268,-0.99985906712276,0.));
#27445=DIRECTION('',(0.,0.,1.));
#27446=DIRECTION('',(-0.0167882665098268,-0.99985906712276,0.));
#27447=DIRECTION('',(0.,0.,1.));
#27448=DIRECTION('',(-0.0167882665098268,-0.99985906712276,0.));
#27449=DIRECTION('center_axis',(0.,0.,1.));
#27450=DIRECTION('ref_axis',(0.499999999999999,-0.866025403784439,0.));
#27451=DIRECTION('center_axis',(0.,0.,1.));
#27452=DIRECTION('ref_axis',(1.,0.,0.));
#27453=DIRECTION('',(-0.874297485587433,0.485390468278368,0.));
#27454=DIRECTION('center_axis',(0.485390468278368,0.874297485587433,0.));
#27455=DIRECTION('ref_axis',(-0.874297485587433,0.485390468278368,0.));
#27456=DIRECTION('',(0.,0.,-1.));
#27457=DIRECTION('',(-0.874297485587433,0.485390468278368,0.));
#27458=DIRECTION('center_axis',(0.,0.,1.));
#27459=DIRECTION('ref_axis',(0.499999999999999,-0.866025403784439,0.));
#27460=DIRECTION('center_axis',(0.,0.,-1.));
#27461=DIRECTION('ref_axis',(1.,0.,0.));
#27462=DIRECTION('center_axis',(-0.961444572476169,0.274998789190275,0.));
#27463=DIRECTION('ref_axis',(-0.274998789190275,-0.961444572476169,0.));
#27464=DIRECTION('',(0.,0.,1.));
#27465=DIRECTION('',(-0.274998789190275,-0.961444572476169,0.));
#27466=DIRECTION('',(0.,0.,1.));
#27467=DIRECTION('',(-0.274998789190275,-0.961444572476169,0.));
#27468=DIRECTION('center_axis',(0.,0.,1.));
#27469=DIRECTION('ref_axis',(0.25881904510252,-0.965925826289068,0.));
#27470=DIRECTION('center_axis',(0.,0.,1.));
#27471=DIRECTION('ref_axis',(1.,0.,0.));
#27472=DIRECTION('',(-0.718878223686823,0.695136029499894,0.));
#27473=DIRECTION('center_axis',(0.695136029499894,0.718878223686823,0.));
#27474=DIRECTION('ref_axis',(-0.718878223686823,0.695136029499894,0.));
#27475=DIRECTION('',(0.,0.,-1.));
#27476=DIRECTION('',(-0.718878223686823,0.695136029499894,0.));
#27477=DIRECTION('center_axis',(0.,0.,1.));
#27478=DIRECTION('ref_axis',(0.25881904510252,-0.965925826289068,0.));
#27479=DIRECTION('center_axis',(0.,0.,-1.));
#27480=DIRECTION('ref_axis',(1.,0.,0.));
#27481=DIRECTION('center_axis',(-0.857509219077607,0.514468598844393,0.));
#27482=DIRECTION('ref_axis',(-0.514468598844393,-0.857509219077607,0.));
#27483=DIRECTION('',(0.,0.,1.));
#27484=DIRECTION('',(-0.514468598844393,-0.857509219077607,0.));
#27485=DIRECTION('',(0.,0.,1.));
#27486=DIRECTION('',(-0.514468598844393,-0.857509219077607,0.));
#27487=DIRECTION('center_axis',(0.,0.,1.));
#27488=DIRECTION('ref_axis',(-1.94289029309402E-16,-1.,0.));
#27489=DIRECTION('center_axis',(0.,0.,1.));
#27490=DIRECTION('ref_axis',(1.,0.,0.));
#27491=DIRECTION('',(-0.514468598844392,0.857509219077607,0.));
#27492=DIRECTION('center_axis',(0.857509219077607,0.514468598844392,0.));
#27493=DIRECTION('ref_axis',(-0.514468598844392,0.857509219077607,0.));
#27494=DIRECTION('',(0.,0.,-1.));
#27495=DIRECTION('',(-0.514468598844392,0.857509219077607,0.));
#27496=DIRECTION('center_axis',(0.,0.,1.));
#27497=DIRECTION('ref_axis',(-1.94289029309402E-16,-1.,0.));
#27498=DIRECTION('center_axis',(0.,0.,-1.));
#27499=DIRECTION('ref_axis',(1.,0.,0.));
#27500=DIRECTION('center_axis',(-0.695136029499893,0.718878223686824,0.));
#27501=DIRECTION('ref_axis',(-0.718878223686824,-0.695136029499893,0.));
#27502=DIRECTION('',(0.,0.,1.));
#27503=DIRECTION('',(-0.718878223686824,-0.695136029499893,0.));
#27504=DIRECTION('',(0.,0.,1.));
#27505=DIRECTION('',(-0.718878223686824,-0.695136029499893,0.));
#27506=DIRECTION('center_axis',(0.,0.,1.));
#27507=DIRECTION('ref_axis',(-0.258819045102522,-0.965925826289068,0.));
#27508=DIRECTION('center_axis',(0.,0.,1.));
#27509=DIRECTION('ref_axis',(1.,0.,0.));
#27510=DIRECTION('',(-0.274998789190274,0.961444572476169,0.));
#27511=DIRECTION('center_axis',(0.961444572476169,0.274998789190274,0.));
#27512=DIRECTION('ref_axis',(-0.274998789190274,0.961444572476169,0.));
#27513=DIRECTION('',(0.,0.,-1.));
#27514=DIRECTION('',(-0.274998789190274,0.961444572476169,0.));
#27515=DIRECTION('center_axis',(0.,0.,1.));
#27516=DIRECTION('ref_axis',(-0.258819045102522,-0.965925826289068,0.));
#27517=DIRECTION('center_axis',(0.,0.,-1.));
#27518=DIRECTION('ref_axis',(1.,0.,0.));
#27519=DIRECTION('center_axis',(-0.485390468278367,0.874297485587433,0.));
#27520=DIRECTION('ref_axis',(-0.874297485587433,-0.485390468278367,0.));
#27521=DIRECTION('',(0.,0.,1.));
#27522=DIRECTION('',(-0.874297485587433,-0.485390468278367,0.));
#27523=DIRECTION('',(0.,0.,1.));
#27524=DIRECTION('',(-0.874297485587433,-0.485390468278367,0.));
#27525=DIRECTION('center_axis',(0.,0.,1.));
#27526=DIRECTION('ref_axis',(-0.500000000000001,-0.866025403784438,0.));
#27527=DIRECTION('center_axis',(0.,0.,1.));
#27528=DIRECTION('ref_axis',(1.,0.,0.));
#27529=DIRECTION('',(-0.0167882665098254,0.99985906712276,0.));
#27530=DIRECTION('center_axis',(0.99985906712276,0.0167882665098254,0.));
#27531=DIRECTION('ref_axis',(-0.0167882665098254,0.99985906712276,0.));
#27532=DIRECTION('',(0.,0.,-1.));
#27533=DIRECTION('',(-0.0167882665098254,0.99985906712276,0.));
#27534=DIRECTION('center_axis',(0.,0.,1.));
#27535=DIRECTION('ref_axis',(-0.500000000000001,-0.866025403784438,0.));
#27536=DIRECTION('center_axis',(0.,0.,-1.));
#27537=DIRECTION('ref_axis',(1.,0.,0.));
#27538=DIRECTION('center_axis',(-0.242566348789345,0.970134818690168,0.));
#27539=DIRECTION('ref_axis',(-0.970134818690168,-0.242566348789345,0.));
#27540=DIRECTION('',(0.,0.,1.));
#27541=DIRECTION('',(-0.970134818690168,-0.242566348789345,0.));
#27542=DIRECTION('',(0.,0.,1.));
#27543=DIRECTION('',(-0.970134818690168,-0.242566348789345,0.));
#27544=DIRECTION('center_axis',(0.,0.,1.));
#27545=DIRECTION('ref_axis',(-0.707106781186548,-0.707106781186547,0.));
#27546=DIRECTION('center_axis',(0.,0.,1.));
#27547=DIRECTION('ref_axis',(1.,0.,0.));
#27548=DIRECTION('',(0.242566348789346,0.970134818690168,0.));
#27549=DIRECTION('center_axis',(0.970134818690168,-0.242566348789346,0.));
#27550=DIRECTION('ref_axis',(0.242566348789346,0.970134818690168,0.));
#27551=DIRECTION('',(0.,0.,-1.));
#27552=DIRECTION('',(0.242566348789346,0.970134818690168,0.));
#27553=DIRECTION('center_axis',(0.,0.,1.));
#27554=DIRECTION('ref_axis',(-0.707106781186548,-0.707106781186547,0.));
#27555=DIRECTION('center_axis',(0.,0.,-1.));
#27556=DIRECTION('ref_axis',(1.,0.,0.));
#27557=DIRECTION('center_axis',(0.0167882665098262,0.99985906712276,0.));
#27558=DIRECTION('ref_axis',(-0.99985906712276,0.0167882665098262,0.));
#27559=DIRECTION('',(0.,0.,1.));
#27560=DIRECTION('',(-0.99985906712276,0.0167882665098262,0.));
#27561=DIRECTION('',(0.,0.,1.));
#27562=DIRECTION('',(-0.99985906712276,0.0167882665098262,0.));
#27563=DIRECTION('center_axis',(0.,0.,1.));
#27564=DIRECTION('ref_axis',(-0.866025403784439,-0.5,0.));
#27565=DIRECTION('center_axis',(0.,0.,1.));
#27566=DIRECTION('ref_axis',(1.,0.,0.));
#27567=DIRECTION('',(0.485390468278367,0.874297485587433,0.));
#27568=DIRECTION('center_axis',(0.874297485587433,-0.485390468278367,0.));
#27569=DIRECTION('ref_axis',(0.485390468278367,0.874297485587433,0.));
#27570=DIRECTION('',(0.,0.,-1.));
#27571=DIRECTION('',(0.485390468278367,0.874297485587433,0.));
#27572=DIRECTION('center_axis',(0.,0.,1.));
#27573=DIRECTION('ref_axis',(-0.866025403784439,-0.5,0.));
#27574=DIRECTION('center_axis',(0.,0.,-1.));
#27575=DIRECTION('ref_axis',(1.,0.,0.));
#27576=DIRECTION('center_axis',(0.274998789190275,0.961444572476169,0.));
#27577=DIRECTION('ref_axis',(-0.961444572476169,0.274998789190275,0.));
#27578=DIRECTION('',(0.,0.,1.));
#27579=DIRECTION('',(-0.961444572476169,0.274998789190275,0.));
#27580=DIRECTION('',(0.,0.,1.));
#27581=DIRECTION('',(-0.961444572476169,0.274998789190275,0.));
#27582=DIRECTION('center_axis',(0.,0.,1.));
#27583=DIRECTION('ref_axis',(-0.965925826289068,-0.25881904510252,0.));
#27584=DIRECTION('center_axis',(0.,0.,1.));
#27585=DIRECTION('ref_axis',(1.,0.,0.));
#27586=DIRECTION('',(0.695136029499894,0.718878223686823,0.));
#27587=DIRECTION('center_axis',(0.718878223686823,-0.695136029499894,0.));
#27588=DIRECTION('ref_axis',(0.695136029499894,0.718878223686823,0.));
#27589=DIRECTION('',(0.,0.,-1.));
#27590=DIRECTION('',(0.695136029499894,0.718878223686823,0.));
#27591=DIRECTION('center_axis',(0.,0.,1.));
#27592=DIRECTION('ref_axis',(-0.965925826289068,-0.25881904510252,0.));
#27593=DIRECTION('center_axis',(0.,0.,-1.));
#27594=DIRECTION('ref_axis',(1.,0.,0.));
#27595=DIRECTION('center_axis',(0.514468598844393,0.857509219077607,0.));
#27596=DIRECTION('ref_axis',(-0.857509219077607,0.514468598844393,0.));
#27597=DIRECTION('',(0.,0.,1.));
#27598=DIRECTION('',(-0.857509219077607,0.514468598844393,0.));
#27599=DIRECTION('',(0.,0.,1.));
#27600=DIRECTION('',(-0.857509219077607,0.514468598844393,0.));
#27601=DIRECTION('center_axis',(0.,0.,1.));
#27602=DIRECTION('ref_axis',(-1.,1.38777878078145E-16,0.));
#27603=DIRECTION('center_axis',(0.,0.,1.));
#27604=DIRECTION('ref_axis',(1.,0.,0.));
#27605=DIRECTION('',(0.857509219077607,0.514468598844393,0.));
#27606=DIRECTION('center_axis',(0.,0.,1.));
#27607=DIRECTION('ref_axis',(1.,0.,0.));
#27608=DIRECTION('center_axis',(0.514468598844393,-0.857509219077607,0.));
#27609=DIRECTION('ref_axis',(0.857509219077607,0.514468598844393,0.));
#27610=DIRECTION('',(0.,0.,-1.));
#27611=DIRECTION('',(0.857509219077607,0.514468598844393,0.));
#27612=DIRECTION('center_axis',(0.,0.,1.));
#27613=DIRECTION('ref_axis',(-1.,1.38777878078145E-16,0.));
#27614=DIRECTION('center_axis',(0.,0.,-1.));
#27615=DIRECTION('ref_axis',(1.,0.,0.));
#27616=DIRECTION('center_axis',(0.,0.,-1.));
#27617=DIRECTION('ref_axis',(1.,0.,0.));
#27618=DIRECTION('center_axis',(0.718878223686824,0.695136029499894,0.));
#27619=DIRECTION('ref_axis',(-0.695136029499894,0.718878223686824,0.));
#27620=DIRECTION('',(0.,0.,1.));
#27621=DIRECTION('',(-0.695136029499894,0.718878223686824,0.));
#27622=DIRECTION('',(0.,0.,1.));
#27623=DIRECTION('',(-0.695136029499894,0.718878223686824,0.));
#27624=DIRECTION('center_axis',(0.,0.,1.));
#27625=DIRECTION('ref_axis',(-0.965925826289068,0.258819045102521,0.));
#27626=DIRECTION('center_axis',(0.,0.,1.));
#27627=DIRECTION('ref_axis',(1.,0.,0.));
#27628=DIRECTION('',(0.961444572476169,0.274998789190274,0.));
#27629=DIRECTION('center_axis',(0.274998789190274,-0.961444572476169,0.));
#27630=DIRECTION('ref_axis',(0.961444572476169,0.274998789190274,0.));
#27631=DIRECTION('',(0.,0.,-1.));
#27632=DIRECTION('',(0.961444572476169,0.274998789190274,0.));
#27633=DIRECTION('center_axis',(0.,0.,1.));
#27634=DIRECTION('ref_axis',(-0.965925826289068,0.258819045102521,0.));
#27635=DIRECTION('center_axis',(0.,0.,-1.));
#27636=DIRECTION('ref_axis',(1.,0.,0.));
#27637=DIRECTION('center_axis',(0.874297485587433,0.485390468278367,0.));
#27638=DIRECTION('ref_axis',(-0.485390468278367,0.874297485587433,0.));
#27639=DIRECTION('',(0.,0.,1.));
#27640=DIRECTION('',(-0.485390468278367,0.874297485587433,0.));
#27641=DIRECTION('',(0.,0.,1.));
#27642=DIRECTION('',(-0.485390468278367,0.874297485587433,0.));
#27643=DIRECTION('center_axis',(0.,0.,1.));
#27644=DIRECTION('ref_axis',(-0.866025403784438,0.5,0.));
#27645=DIRECTION('center_axis',(0.,0.,1.));
#27646=DIRECTION('ref_axis',(1.,0.,0.));
#27647=DIRECTION('',(0.99985906712276,0.0167882665098256,0.));
#27648=DIRECTION('center_axis',(0.0167882665098256,-0.99985906712276,0.));
#27649=DIRECTION('ref_axis',(0.99985906712276,0.0167882665098256,0.));
#27650=DIRECTION('',(0.,0.,-1.));
#27651=DIRECTION('',(0.99985906712276,0.0167882665098256,0.));
#27652=DIRECTION('center_axis',(0.,0.,1.));
#27653=DIRECTION('ref_axis',(-0.866025403784438,0.5,0.));
#27654=DIRECTION('center_axis',(0.,0.,-1.));
#27655=DIRECTION('ref_axis',(1.,0.,0.));
#27656=DIRECTION('center_axis',(0.970134818690168,0.242566348789345,0.));
#27657=DIRECTION('ref_axis',(-0.242566348789345,0.970134818690168,0.));
#27658=DIRECTION('',(0.,0.,1.));
#27659=DIRECTION('',(-0.242566348789345,0.970134818690168,0.));
#27660=DIRECTION('',(0.,0.,1.));
#27661=DIRECTION('',(-0.242566348789345,0.970134818690168,0.));
#27662=DIRECTION('center_axis',(0.,0.,1.));
#27663=DIRECTION('ref_axis',(-0.707106781186548,0.707106781186548,0.));
#27664=DIRECTION('center_axis',(0.,0.,1.));
#27665=DIRECTION('ref_axis',(1.,0.,0.));
#27666=DIRECTION('',(0.970134818690168,-0.242566348789345,0.));
#27667=DIRECTION('center_axis',(-0.242566348789345,-0.970134818690168,0.));
#27668=DIRECTION('ref_axis',(0.970134818690168,-0.242566348789345,0.));
#27669=DIRECTION('',(0.,0.,-1.));
#27670=DIRECTION('',(0.970134818690168,-0.242566348789345,0.));
#27671=DIRECTION('center_axis',(0.,0.,1.));
#27672=DIRECTION('ref_axis',(-0.707106781186548,0.707106781186548,0.));
#27673=DIRECTION('center_axis',(0.,0.,-1.));
#27674=DIRECTION('ref_axis',(1.,0.,0.));
#27675=DIRECTION('center_axis',(0.99985906712276,-0.0167882665098261,0.));
#27676=DIRECTION('ref_axis',(0.0167882665098261,0.99985906712276,0.));
#27677=DIRECTION('',(0.,0.,1.));
#27678=DIRECTION('',(0.0167882665098261,0.99985906712276,0.));
#27679=DIRECTION('',(0.,0.,1.));
#27680=DIRECTION('',(0.0167882665098261,0.99985906712276,0.));
#27681=DIRECTION('center_axis',(0.,0.,1.));
#27682=DIRECTION('ref_axis',(-0.5,0.866025403784439,0.));
#27683=DIRECTION('center_axis',(0.,0.,1.));
#27684=DIRECTION('ref_axis',(1.,0.,0.));
#27685=DIRECTION('',(0.874297485587433,-0.485390468278367,0.));
#27686=DIRECTION('center_axis',(-0.485390468278367,-0.874297485587433,0.));
#27687=DIRECTION('ref_axis',(0.874297485587433,-0.485390468278367,0.));
#27688=DIRECTION('',(0.,0.,-1.));
#27689=DIRECTION('',(0.874297485587433,-0.485390468278367,0.));
#27690=DIRECTION('center_axis',(0.,0.,1.));
#27691=DIRECTION('ref_axis',(-0.5,0.866025403784439,0.));
#27692=DIRECTION('center_axis',(0.,0.,-1.));
#27693=DIRECTION('ref_axis',(1.,0.,0.));
#27694=DIRECTION('center_axis',(0.961444572476169,-0.274998789190275,0.));
#27695=DIRECTION('ref_axis',(0.274998789190275,0.961444572476169,0.));
#27696=DIRECTION('',(0.,0.,1.));
#27697=DIRECTION('',(0.274998789190275,0.961444572476169,0.));
#27698=DIRECTION('',(0.,0.,1.));
#27699=DIRECTION('',(0.274998789190275,0.961444572476169,0.));
#27700=DIRECTION('center_axis',(0.,0.,1.));
#27701=DIRECTION('ref_axis',(-0.258819045102521,0.965925826289068,0.));
#27702=DIRECTION('center_axis',(0.,0.,1.));
#27703=DIRECTION('ref_axis',(1.,0.,0.));
#27704=DIRECTION('',(0.718878223686824,-0.695136029499894,0.));
#27705=DIRECTION('center_axis',(-0.695136029499894,-0.718878223686824,0.));
#27706=DIRECTION('ref_axis',(0.718878223686824,-0.695136029499894,0.));
#27707=DIRECTION('',(0.,0.,-1.));
#27708=DIRECTION('',(0.718878223686824,-0.695136029499894,0.));
#27709=DIRECTION('center_axis',(0.,0.,1.));
#27710=DIRECTION('ref_axis',(-0.258819045102521,0.965925826289068,0.));
#27711=DIRECTION('center_axis',(0.,0.,-1.));
#27712=DIRECTION('ref_axis',(1.,0.,0.));
#27713=DIRECTION('center_axis',(0.857509219077607,-0.514468598844393,0.));
#27714=DIRECTION('ref_axis',(0.514468598844393,0.857509219077607,0.));
#27715=DIRECTION('',(0.,0.,1.));
#27716=DIRECTION('',(0.514468598844393,0.857509219077607,0.));
#27717=DIRECTION('',(0.,0.,1.));
#27718=DIRECTION('',(0.514468598844393,0.857509219077607,0.));
#27719=DIRECTION('center_axis',(0.,0.,1.));
#27720=DIRECTION('ref_axis',(8.32667268468867E-17,1.,0.));
#27721=DIRECTION('center_axis',(0.,0.,1.));
#27722=DIRECTION('ref_axis',(1.,0.,0.));
#27723=DIRECTION('',(0.514468598844393,-0.857509219077607,0.));
#27724=DIRECTION('center_axis',(-0.857509219077607,-0.514468598844393,0.));
#27725=DIRECTION('ref_axis',(0.514468598844393,-0.857509219077607,0.));
#27726=DIRECTION('',(0.,0.,-1.));
#27727=DIRECTION('',(0.514468598844393,-0.857509219077607,0.));
#27728=DIRECTION('center_axis',(0.,0.,1.));
#27729=DIRECTION('ref_axis',(8.32667268468867E-17,1.,0.));
#27730=DIRECTION('center_axis',(0.,0.,-1.));
#27731=DIRECTION('ref_axis',(1.,0.,0.));
#27732=DIRECTION('center_axis',(0.695136029499894,-0.718878223686824,0.));
#27733=DIRECTION('ref_axis',(0.718878223686824,0.695136029499894,0.));
#27734=DIRECTION('',(0.,0.,1.));
#27735=DIRECTION('',(0.718878223686824,0.695136029499894,0.));
#27736=DIRECTION('',(0.,0.,1.));
#27737=DIRECTION('',(0.718878223686824,0.695136029499894,0.));
#27738=DIRECTION('center_axis',(0.,0.,1.));
#27739=DIRECTION('ref_axis',(0.258819045102521,0.965925826289068,0.));
#27740=DIRECTION('center_axis',(0.,0.,1.));
#27741=DIRECTION('ref_axis',(1.,0.,0.));
#27742=DIRECTION('',(0.274998789190274,-0.961444572476169,0.));
#27743=DIRECTION('center_axis',(-0.961444572476169,-0.274998789190274,0.));
#27744=DIRECTION('ref_axis',(0.274998789190274,-0.961444572476169,0.));
#27745=DIRECTION('',(0.,0.,-1.));
#27746=DIRECTION('',(0.274998789190274,-0.961444572476169,0.));
#27747=DIRECTION('center_axis',(0.,0.,1.));
#27748=DIRECTION('ref_axis',(0.258819045102521,0.965925826289068,0.));
#27749=DIRECTION('center_axis',(0.,0.,-1.));
#27750=DIRECTION('ref_axis',(1.,0.,0.));
#27751=DIRECTION('center_axis',(0.485390468278367,-0.874297485587433,0.));
#27752=DIRECTION('ref_axis',(0.874297485587433,0.485390468278367,0.));
#27753=DIRECTION('',(0.,0.,1.));
#27754=DIRECTION('',(0.874297485587433,0.485390468278367,0.));
#27755=DIRECTION('',(0.,0.,1.));
#27756=DIRECTION('',(0.874297485587433,0.485390468278367,0.));
#27757=DIRECTION('center_axis',(0.,0.,1.));
#27758=DIRECTION('ref_axis',(0.5,0.866025403784439,0.));
#27759=DIRECTION('center_axis',(0.,0.,1.));
#27760=DIRECTION('ref_axis',(1.,0.,0.));
#27761=DIRECTION('',(0.0167882665098258,-0.99985906712276,0.));
#27762=DIRECTION('center_axis',(-0.99985906712276,-0.0167882665098258,0.));
#27763=DIRECTION('ref_axis',(0.0167882665098258,-0.99985906712276,0.));
#27764=DIRECTION('',(0.,0.,-1.));
#27765=DIRECTION('',(0.0167882665098258,-0.99985906712276,0.));
#27766=DIRECTION('center_axis',(0.,0.,1.));
#27767=DIRECTION('ref_axis',(0.5,0.866025403784439,0.));
#27768=DIRECTION('center_axis',(0.,0.,-1.));
#27769=DIRECTION('ref_axis',(1.,0.,0.));
#27770=DIRECTION('center_axis',(0.242566348789345,-0.970134818690168,0.));
#27771=DIRECTION('ref_axis',(0.970134818690168,0.242566348789345,0.));
#27772=DIRECTION('',(0.,0.,1.));
#27773=DIRECTION('',(0.970134818690168,0.242566348789345,0.));
#27774=DIRECTION('',(0.,0.,1.));
#27775=DIRECTION('',(0.970134818690168,0.242566348789345,0.));
#27776=DIRECTION('center_axis',(0.,0.,1.));
#27777=DIRECTION('ref_axis',(0.707106781186547,0.707106781186548,0.));
#27778=DIRECTION('center_axis',(0.,0.,1.));
#27779=DIRECTION('ref_axis',(1.,0.,0.));
#27780=DIRECTION('',(-0.242566348789345,-0.970134818690168,0.));
#27781=DIRECTION('center_axis',(-0.970134818690168,0.242566348789345,0.));
#27782=DIRECTION('ref_axis',(-0.242566348789345,-0.970134818690168,0.));
#27783=DIRECTION('',(0.,0.,-1.));
#27784=DIRECTION('',(-0.242566348789345,-0.970134818690168,0.));
#27785=DIRECTION('center_axis',(0.,0.,1.));
#27786=DIRECTION('ref_axis',(0.707106781186547,0.707106781186548,0.));
#27787=DIRECTION('center_axis',(0.,0.,-1.));
#27788=DIRECTION('ref_axis',(1.,0.,0.));
#27789=DIRECTION('center_axis',(-0.0167882665098259,-0.99985906712276,0.));
#27790=DIRECTION('ref_axis',(0.99985906712276,-0.0167882665098259,0.));
#27791=DIRECTION('',(0.,0.,1.));
#27792=DIRECTION('',(0.99985906712276,-0.0167882665098259,0.));
#27793=DIRECTION('',(0.,0.,1.));
#27794=DIRECTION('',(0.99985906712276,-0.0167882665098259,0.));
#27795=DIRECTION('center_axis',(0.,0.,1.));
#27796=DIRECTION('ref_axis',(0.866025403784439,0.5,0.));
#27797=DIRECTION('center_axis',(0.,0.,1.));
#27798=DIRECTION('ref_axis',(1.,0.,0.));
#27799=DIRECTION('',(-0.485390468278367,-0.874297485587433,0.));
#27800=DIRECTION('center_axis',(-0.874297485587433,0.485390468278367,0.));
#27801=DIRECTION('ref_axis',(-0.485390468278367,-0.874297485587433,0.));
#27802=DIRECTION('',(0.,0.,-1.));
#27803=DIRECTION('',(-0.485390468278367,-0.874297485587433,0.));
#27804=DIRECTION('center_axis',(0.,0.,1.));
#27805=DIRECTION('ref_axis',(0.866025403784439,0.5,0.));
#27806=DIRECTION('center_axis',(0.,0.,-1.));
#27807=DIRECTION('ref_axis',(1.,0.,0.));
#27808=DIRECTION('center_axis',(-0.274998789190275,-0.961444572476169,0.));
#27809=DIRECTION('ref_axis',(0.961444572476169,-0.274998789190275,0.));
#27810=DIRECTION('',(0.,0.,1.));
#27811=DIRECTION('',(0.961444572476169,-0.274998789190275,0.));
#27812=DIRECTION('',(0.,0.,1.));
#27813=DIRECTION('',(0.961444572476169,-0.274998789190275,0.));
#27814=DIRECTION('center_axis',(0.,0.,1.));
#27815=DIRECTION('ref_axis',(0.965925826289068,0.258819045102521,0.));
#27816=DIRECTION('center_axis',(0.,0.,1.));
#27817=DIRECTION('ref_axis',(1.,0.,0.));
#27818=DIRECTION('',(-0.695136029499894,-0.718878223686824,0.));
#27819=DIRECTION('center_axis',(-0.718878223686824,0.695136029499894,0.));
#27820=DIRECTION('ref_axis',(-0.695136029499894,-0.718878223686824,0.));
#27821=DIRECTION('',(0.,0.,-1.));
#27822=DIRECTION('',(-0.695136029499894,-0.718878223686824,0.));
#27823=DIRECTION('center_axis',(0.,0.,1.));
#27824=DIRECTION('ref_axis',(0.965925826289068,0.258819045102521,0.));
#27825=DIRECTION('center_axis',(0.,0.,-1.));
#27826=DIRECTION('ref_axis',(1.,0.,0.));
#27827=DIRECTION('center_axis',(-0.514468598844393,-0.857509219077607,0.));
#27828=DIRECTION('ref_axis',(0.857509219077607,-0.514468598844393,0.));
#27829=DIRECTION('',(0.,0.,1.));
#27830=DIRECTION('',(0.857509219077607,-0.514468598844393,0.));
#27831=DIRECTION('',(0.,0.,1.));
#27832=DIRECTION('',(0.857509219077607,-0.514468598844393,0.));
#27833=DIRECTION('center_axis',(0.,0.,1.));
#27834=DIRECTION('ref_axis',(1.,0.,0.));
#27835=DIRECTION('center_axis',(0.,0.,1.));
#27836=DIRECTION('ref_axis',(1.,0.,0.));
#27837=DIRECTION('',(-0.857509219077607,-0.514468598844393,0.));
#27838=DIRECTION('center_axis',(-0.514468598844393,0.857509219077607,0.));
#27839=DIRECTION('ref_axis',(-0.857509219077607,-0.514468598844393,0.));
#27840=DIRECTION('',(0.,0.,-1.));
#27841=DIRECTION('',(-0.857509219077607,-0.514468598844393,0.));
#27842=DIRECTION('center_axis',(0.,0.,1.));
#27843=DIRECTION('ref_axis',(1.,0.,0.));
#27844=DIRECTION('center_axis',(0.,0.,-1.));
#27845=DIRECTION('ref_axis',(1.,0.,0.));
#27846=DIRECTION('center_axis',(0.,0.,1.));
#27847=DIRECTION('ref_axis',(1.,0.,0.));
#27848=DIRECTION('center_axis',(0.,0.,1.));
#27849=DIRECTION('ref_axis',(1.,0.,0.));
#27850=DIRECTION('',(0.,0.,-1.));
#27851=DIRECTION('center_axis',(0.,0.,-1.));
#27852=DIRECTION('ref_axis',(1.,0.,0.));
#27853=DIRECTION('center_axis',(0.,0.,-1.));
#27854=DIRECTION('ref_axis',(1.,0.,0.));
#27855=DIRECTION('center_axis',(0.,0.,1.));
#27856=DIRECTION('ref_axis',(1.,0.,0.));
#27857=DIRECTION('',(-0.600000000000002,-7.34788079488414E-17,-0.799999999999999));
#27858=DIRECTION('center_axis',(0.,0.,1.));
#27859=DIRECTION('ref_axis',(1.,0.,0.));
#27860=DIRECTION('center_axis',(0.,0.,-1.));
#27861=DIRECTION('ref_axis',(-1.,0.,0.));
#27862=DIRECTION('center_axis',(0.,0.,1.));
#27863=DIRECTION('ref_axis',(1.,0.,0.));
#27864=DIRECTION('center_axis',(0.,0.,1.));
#27865=DIRECTION('ref_axis',(1.,0.,0.));
#27866=DIRECTION('',(0.,0.,1.));
#27867=DIRECTION('center_axis',(0.,0.,-1.));
#27868=DIRECTION('ref_axis',(1.,0.,0.));
#27869=DIRECTION('center_axis',(0.,0.,1.));
#27870=DIRECTION('ref_axis',(1.,0.,0.));
#27871=DIRECTION('center_axis',(0.,0.,1.));
#27872=DIRECTION('ref_axis',(1.,0.,0.));
#27873=DIRECTION('',(0.,0.,-1.));
#27874=DIRECTION('',(0.,0.,-1.));
#27875=DIRECTION('center_axis',(0.,0.,-1.));
#27876=DIRECTION('ref_axis',(1.,0.,0.));
#27877=DIRECTION('center_axis',(0.,0.,-1.));
#27878=DIRECTION('ref_axis',(-1.,0.,0.));
#27879=DIRECTION('center_axis',(0.,0.,1.));
#27880=DIRECTION('ref_axis',(1.,0.,0.));
#27881=DIRECTION('center_axis',(0.,0.,1.));
#27882=DIRECTION('ref_axis',(1.,0.,0.));
#27883=DIRECTION('center_axis',(0.,0.,1.));
#27884=DIRECTION('ref_axis',(1.,0.,0.));
#27885=DIRECTION('',(0.,0.,-1.));
#27886=DIRECTION('center_axis',(0.,0.,-1.));
#27887=DIRECTION('ref_axis',(1.,0.,0.));
#27888=DIRECTION('center_axis',(0.,0.,1.));
#27889=DIRECTION('ref_axis',(1.,0.,0.));
#27890=DIRECTION('',(-0.70710678118655,-8.65956056235496E-17,-0.707106781186545));
#27891=DIRECTION('center_axis',(0.,0.,1.));
#27892=DIRECTION('ref_axis',(1.,0.,0.));
#27893=DIRECTION('center_axis',(-3.49629579342466E-16,-1.,0.));
#27894=DIRECTION('ref_axis',(1.,-3.49629579342466E-16,0.));
#27895=DIRECTION('',(-1.,3.49629579342466E-16,0.));
#27896=DIRECTION('',(0.,0.,1.));
#27897=DIRECTION('',(1.,-3.49629579342466E-16,0.));
#27898=DIRECTION('',(0.,0.,1.));
#27899=DIRECTION('center_axis',(-0.866025403784439,-0.5,0.));
#27900=DIRECTION('ref_axis',(0.5,-0.866025403784439,0.));
#27901=DIRECTION('',(-0.5,0.866025403784439,0.));
#27902=DIRECTION('',(0.5,-0.866025403784439,0.));
#27903=DIRECTION('',(0.,0.,1.));
#27904=DIRECTION('center_axis',(-0.866025403784439,0.5,0.));
#27905=DIRECTION('ref_axis',(-0.5,-0.866025403784439,0.));
#27906=DIRECTION('',(0.5,0.866025403784439,0.));
#27907=DIRECTION('',(-0.5,-0.866025403784439,0.));
#27908=DIRECTION('',(0.,0.,1.));
#27909=DIRECTION('center_axis',(1.74814789671233E-16,1.,0.));
#27910=DIRECTION('ref_axis',(-1.,1.74814789671233E-16,0.));
#27911=DIRECTION('',(1.,-1.74814789671233E-16,0.));
#27912=DIRECTION('',(-1.,1.74814789671233E-16,0.));
#27913=DIRECTION('',(0.,0.,1.));
#27914=DIRECTION('center_axis',(0.866025403784439,0.5,0.));
#27915=DIRECTION('ref_axis',(-0.5,0.866025403784439,0.));
#27916=DIRECTION('',(0.5,-0.866025403784439,0.));
#27917=DIRECTION('',(-0.5,0.866025403784439,0.));
#27918=DIRECTION('',(0.,0.,1.));
#27919=DIRECTION('center_axis',(0.866025403784439,-0.5,0.));
#27920=DIRECTION('ref_axis',(0.5,0.866025403784439,0.));
#27921=DIRECTION('',(-0.5,-0.866025403784439,0.));
#27922=DIRECTION('',(0.5,0.866025403784439,0.));
#27923=DIRECTION('center_axis',(0.,0.,1.));
#27924=DIRECTION('ref_axis',(1.,0.,0.));
#27925=DIRECTION('center_axis',(0.,0.,1.));
#27926=DIRECTION('ref_axis',(1.,0.,0.));
#27927=DIRECTION('',(0.,-1.,0.));
#27928=DIRECTION('',(-1.,0.,0.));
#27929=DIRECTION('',(0.,1.,0.));
#27930=DIRECTION('',(1.,0.,0.));
#27931=DIRECTION('center_axis',(0.,0.,-1.));
#27932=DIRECTION('ref_axis',(1.,0.,0.));
#27933=DIRECTION('center_axis',(0.,1.,0.));
#27934=DIRECTION('ref_axis',(-1.,0.,0.));
#27935=DIRECTION('',(0.,0.,1.));
#27936=DIRECTION('',(-1.,0.,0.));
#27937=DIRECTION('',(0.,0.,1.));
#27938=DIRECTION('center_axis',(1.,0.,0.));
#27939=DIRECTION('ref_axis',(0.,1.,0.));
#27940=DIRECTION('',(0.,1.,0.));
#27941=DIRECTION('',(0.,0.,1.));
#27942=DIRECTION('center_axis',(0.,-1.,0.));
#27943=DIRECTION('ref_axis',(1.,0.,0.));
#27944=DIRECTION('',(1.,0.,0.));
#27945=DIRECTION('',(0.,0.,1.));
#27946=DIRECTION('center_axis',(-1.,0.,0.));
#27947=DIRECTION('ref_axis',(0.,-1.,0.));
#27948=DIRECTION('',(0.,-1.,0.));
#27949=DIRECTION('center_axis',(0.,0.,1.));
#27950=DIRECTION('ref_axis',(1.,0.,0.));
#27951=DIRECTION('center_axis',(0.,0.,-1.));
#27952=DIRECTION('ref_axis',(-1.,0.,0.));
#27953=DIRECTION('center_axis',(0.,0.,1.));
#27954=DIRECTION('ref_axis',(1.,0.,0.));
#27955=DIRECTION('center_axis',(0.,0.,1.));
#27956=DIRECTION('ref_axis',(1.,0.,0.));
#27957=DIRECTION('',(0.707106781186548,8.65956056235493E-17,-0.707106781186548));
#27958=DIRECTION('center_axis',(0.,0.,1.));
#27959=DIRECTION('ref_axis',(1.,0.,0.));
#27960=DIRECTION('axis',(0.,0.,1.));
#27961=DIRECTION('refdir',(1.,0.,0.));
#27962=DIRECTION('center_axis',(0.,0.,-1.));
#27963=DIRECTION('ref_axis',(-1.,0.,0.));
#27964=DIRECTION('center_axis',(0.,0.,-1.));
#27965=DIRECTION('ref_axis',(-1.,0.,0.));
#27966=DIRECTION('',(0.707106781186546,8.65956056235491E-17,-0.707106781186549));
#27967=DIRECTION('center_axis',(0.,0.,1.));
#27968=DIRECTION('ref_axis',(-1.,0.,0.));
#27969=DIRECTION('center_axis',(0.,0.,1.));
#27970=DIRECTION('ref_axis',(-1.,0.,0.));
#27971=DIRECTION('center_axis',(0.,0.,1.));
#27972=DIRECTION('ref_axis',(1.,0.,0.));
#27973=DIRECTION('',(0.,0.,-1.));
#27974=DIRECTION('center_axis',(0.,0.,-1.));
#27975=DIRECTION('ref_axis',(-1.,0.,0.));
#27976=DIRECTION('center_axis',(0.,0.,-1.));
#27977=DIRECTION('ref_axis',(-1.,0.,0.));
#27978=DIRECTION('center_axis',(0.,0.,1.));
#27979=DIRECTION('ref_axis',(1.,0.,0.));
#27980=DIRECTION('center_axis',(0.,0.,1.));
#27981=DIRECTION('ref_axis',(-1.,0.,0.));
#27982=DIRECTION('',(-0.707106781186546,-8.65956056235491E-17,-0.707106781186549));
#27983=DIRECTION('center_axis',(0.,0.,1.));
#27984=DIRECTION('ref_axis',(-1.,0.,0.));
#27985=DIRECTION('center_axis',(0.,0.,-1.));
#27986=DIRECTION('ref_axis',(-1.,0.,0.));
#27987=DIRECTION('axis',(0.,0.,1.));
#27988=DIRECTION('refdir',(1.,0.,0.));
#27989=DIRECTION('center_axis',(0.,0.,1.));
#27990=DIRECTION('ref_axis',(1.,0.,0.));
#27991=DIRECTION('center_axis',(0.,0.,1.));
#27992=DIRECTION('ref_axis',(1.,0.,0.));
#27993=DIRECTION('',(0.,0.,1.));
#27994=DIRECTION('center_axis',(0.,0.,1.));
#27995=DIRECTION('ref_axis',(1.,0.,0.));
#27996=DIRECTION('center_axis',(0.,0.,-1.));
#27997=DIRECTION('ref_axis',(-1.,0.,0.));
#27998=DIRECTION('center_axis',(0.,0.,-1.));
#27999=DIRECTION('ref_axis',(1.,0.,0.));
#28000=DIRECTION('center_axis',(0.,0.,1.));
#28001=DIRECTION('ref_axis',(1.,0.,0.));
#28002=DIRECTION('center_axis',(0.,0.,1.));
#28003=DIRECTION('ref_axis',(1.,0.,0.));
#28004=DIRECTION('center_axis',(0.,0.,1.));
#28005=DIRECTION('ref_axis',(1.,0.,0.));
#28006=DIRECTION('center_axis',(0.,0.,1.));
#28007=DIRECTION('ref_axis',(-1.,0.,0.));
#28008=DIRECTION('center_axis',(0.,0.,1.));
#28009=DIRECTION('ref_axis',(-1.,0.,0.));
#28010=DIRECTION('',(0.,0.,-1.));
#28011=DIRECTION('center_axis',(0.,0.,1.));
#28012=DIRECTION('ref_axis',(1.,0.,0.));
#28013=DIRECTION('center_axis',(0.,0.,1.));
#28014=DIRECTION('ref_axis',(1.,0.,0.));
#28015=DIRECTION('',(0.,0.,1.));
#28016=DIRECTION('center_axis',(0.,0.,1.));
#28017=DIRECTION('ref_axis',(1.,0.,0.));
#28018=DIRECTION('center_axis',(0.,0.,-1.));
#28019=DIRECTION('ref_axis',(-1.,0.,0.));
#28020=DIRECTION('center_axis',(0.,0.,-1.));
#28021=DIRECTION('ref_axis',(1.,0.,0.));
#28022=DIRECTION('center_axis',(0.,0.,1.));
#28023=DIRECTION('ref_axis',(1.,0.,0.));
#28024=DIRECTION('center_axis',(0.,0.,1.));
#28025=DIRECTION('ref_axis',(1.,0.,0.));
#28026=DIRECTION('center_axis',(0.,0.,1.));
#28027=DIRECTION('ref_axis',(1.,0.,0.));
#28028=DIRECTION('',(0.,0.,-1.));
#28029=DIRECTION('center_axis',(0.,0.,-1.));
#28030=DIRECTION('ref_axis',(-1.,0.,0.));
#28031=DIRECTION('center_axis',(0.,0.,-1.));
#28032=DIRECTION('ref_axis',(-1.,0.,0.));
#28033=DIRECTION('',(0.707106781186548,8.65956056235493E-17,-0.707106781186548));
#28034=DIRECTION('center_axis',(0.,0.,1.));
#28035=DIRECTION('ref_axis',(1.,0.,0.));
#28036=DIRECTION('',(0.,0.,-1.));
#28037=DIRECTION('center_axis',(0.,0.,-1.));
#28038=DIRECTION('ref_axis',(-1.,0.,0.));
#28039=DIRECTION('center_axis',(0.,0.,-1.));
#28040=DIRECTION('ref_axis',(-1.,0.,0.));
#28041=DIRECTION('center_axis',(0.,0.,1.));
#28042=DIRECTION('ref_axis',(1.,0.,0.));
#28043=DIRECTION('center_axis',(0.,0.,1.));
#28044=DIRECTION('ref_axis',(1.,0.,0.));
#28045=DIRECTION('center_axis',(0.,0.,1.));
#28046=DIRECTION('ref_axis',(-1.,0.,0.));
#28047=DIRECTION('',(-0.707106781186548,-8.65956056235493E-17,-0.707106781186548));
#28048=DIRECTION('center_axis',(0.,0.,1.));
#28049=DIRECTION('ref_axis',(-1.,0.,0.));
#28050=DIRECTION('center_axis',(0.,0.,-1.));
#28051=DIRECTION('ref_axis',(-1.,0.,0.));
#28052=DIRECTION('center_axis',(0.,0.,1.));
#28053=DIRECTION('ref_axis',(1.,0.,0.));
#28054=DIRECTION('center_axis',(0.,0.,1.));
#28055=DIRECTION('ref_axis',(1.,0.,0.));
#28056=DIRECTION('',(0.,0.,-1.));
#28057=DIRECTION('axis',(0.,0.,1.));
#28058=DIRECTION('refdir',(1.,0.,0.));
#28059=DIRECTION('center_axis',(0.,6.92018220157531E-16,-1.));
#28060=DIRECTION('ref_axis',(-1.,-3.00652077147108E-17,0.));
#28061=DIRECTION('center_axis',(0.,0.,-1.));
#28062=DIRECTION('ref_axis',(-1.,-6.12323399573677E-17,0.));
#28063=DIRECTION('center_axis',(0.,0.,-1.));
#28064=DIRECTION('ref_axis',(-1.,-6.12323399573677E-17,0.));
#28065=DIRECTION('',(0.382683432365084,6.97712130664731E-16,-0.923879532511289));
#28066=DIRECTION('center_axis',(0.,0.,1.));
#28067=DIRECTION('ref_axis',(-1.,0.,0.));
#28068=DIRECTION('center_axis',(0.,0.,1.));
#28069=DIRECTION('ref_axis',(-1.,0.,0.));
#28070=DIRECTION('center_axis',(0.,0.,1.));
#28071=DIRECTION('ref_axis',(1.,0.,0.));
#28072=DIRECTION('',(0.,0.,-1.));
#28073=DIRECTION('center_axis',(0.,0.,-1.));
#28074=DIRECTION('ref_axis',(-1.,0.,0.));
#28075=DIRECTION('center_axis',(0.,0.,-1.));
#28076=DIRECTION('ref_axis',(-1.,0.,0.));
#28077=DIRECTION('center_axis',(0.,0.,-1.));
#28078=DIRECTION('ref_axis',(1.,0.,0.));
#28079=DIRECTION('center_axis',(0.,0.,1.));
#28080=DIRECTION('ref_axis',(1.,0.,0.));
#28081=DIRECTION('',(-0.707106781186548,-8.65956056235493E-17,-0.707106781186548));
#28082=DIRECTION('center_axis',(0.,0.,1.));
#28083=DIRECTION('ref_axis',(-1.,0.,0.));
#28084=DIRECTION('',(-0.707106781186545,-8.6595605623549E-17,-0.70710678118655));
#28085=DIRECTION('center_axis',(0.,0.,1.));
#28086=DIRECTION('ref_axis',(-1.,0.,0.));
#28087=DIRECTION('center_axis',(0.,0.,-1.));
#28088=DIRECTION('ref_axis',(-1.,0.,0.));
#28089=DIRECTION('center_axis',(0.,0.,1.));
#28090=DIRECTION('ref_axis',(1.,0.,0.));
#28091=DIRECTION('center_axis',(-0.714953656968427,-0.69917184467588,0.));
#28092=DIRECTION('ref_axis',(0.69917184467588,-0.714953656968427,0.));
#28093=DIRECTION('',(0.,0.,1.));
#28094=DIRECTION('',(0.69917184467588,-0.714953656968427,0.));
#28095=DIRECTION('',(0.,0.,1.));
#28096=DIRECTION('',(0.69917184467588,-0.714953656968427,0.));
#28097=DIRECTION('center_axis',(0.,0.,1.));
#28098=DIRECTION('ref_axis',(0.939692620785908,-0.342020143325669,0.));
#28099=DIRECTION('center_axis',(0.,0.,1.));
#28100=DIRECTION('ref_axis',(1.,0.,0.));
#28101=DIRECTION('',(-0.995160058598588,-0.0982672772089165,0.));
#28102=DIRECTION('center_axis',(-0.0982672772089165,0.995160058598588,0.));
#28103=DIRECTION('ref_axis',(-0.995160058598588,-0.0982672772089165,0.));
#28104=DIRECTION('',(0.,0.,-1.));
#28105=DIRECTION('',(-0.995160058598588,-0.0982672772089165,0.));
#28106=DIRECTION('center_axis',(0.,0.,1.));
#28107=DIRECTION('ref_axis',(0.939692620785908,-0.342020143325669,0.));
#28108=DIRECTION('center_axis',(0.,0.,-1.));
#28109=DIRECTION('ref_axis',(1.,0.,0.));
#28110=DIRECTION('center_axis',(-0.910967530182447,-0.412478070875644,0.));
#28111=DIRECTION('ref_axis',(0.412478070875644,-0.910967530182447,0.));
#28112=DIRECTION('',(0.,0.,1.));
#28113=DIRECTION('',(0.412478070875644,-0.910967530182447,0.));
#28114=DIRECTION('',(0.,0.,1.));
#28115=DIRECTION('',(0.412478070875644,-0.910967530182447,0.));
#28116=DIRECTION('center_axis',(0.,0.,1.));
#28117=DIRECTION('ref_axis',(0.766044443118978,-0.64278760968654,0.));
#28118=DIRECTION('center_axis',(0.,0.,1.));
#28119=DIRECTION('ref_axis',(1.,0.,0.));
#28120=DIRECTION('',(-0.968753951801183,0.248023750615928,0.));
#28121=DIRECTION('center_axis',(0.248023750615928,0.968753951801183,0.));
#28122=DIRECTION('ref_axis',(-0.968753951801183,0.248023750615928,0.));
#28123=DIRECTION('',(0.,0.,-1.));
#28124=DIRECTION('',(-0.968753951801183,0.248023750615928,0.));
#28125=DIRECTION('center_axis',(0.,0.,1.));
#28126=DIRECTION('ref_axis',(0.766044443118978,-0.64278760968654,0.));
#28127=DIRECTION('center_axis',(0.,0.,-1.));
#28128=DIRECTION('ref_axis',(1.,0.,0.));
#28129=DIRECTION('center_axis',(-0.997105274807593,-0.076033354199819,0.));
#28130=DIRECTION('ref_axis',(0.076033354199819,-0.997105274807593,0.));
#28131=DIRECTION('',(0.,0.,1.));
#28132=DIRECTION('',(0.076033354199819,-0.997105274807593,0.));
#28133=DIRECTION('',(0.,0.,1.));
#28134=DIRECTION('',(0.076033354199819,-0.997105274807593,0.));
#28135=DIRECTION('center_axis',(0.,0.,1.));
#28136=DIRECTION('ref_axis',(0.5,-0.866025403784439,0.));
#28137=DIRECTION('center_axis',(0.,0.,1.));
#28138=DIRECTION('ref_axis',(1.,0.,0.));
#28139=DIRECTION('',(-0.82550182113093,0.56439945367578,0.));
#28140=DIRECTION('center_axis',(0.56439945367578,0.82550182113093,0.));
#28141=DIRECTION('ref_axis',(-0.82550182113093,0.56439945367578,0.));
#28142=DIRECTION('',(0.,0.,-1.));
#28143=DIRECTION('',(-0.82550182113093,0.56439945367578,0.));
#28144=DIRECTION('center_axis',(0.,0.,1.));
#28145=DIRECTION('ref_axis',(0.5,-0.866025403784439,0.));
#28146=DIRECTION('center_axis',(0.,0.,-1.));
#28147=DIRECTION('ref_axis',(1.,0.,0.));
#28148=DIRECTION('center_axis',(-0.962977407584354,0.269582107125302,0.));
#28149=DIRECTION('ref_axis',(-0.269582107125302,-0.962977407584354,0.));
#28150=DIRECTION('',(0.,0.,1.));
#28151=DIRECTION('',(-0.269582107125302,-0.962977407584354,0.));
#28152=DIRECTION('',(0.,0.,1.));
#28153=DIRECTION('',(-0.269582107125302,-0.962977407584354,0.));
#28154=DIRECTION('center_axis',(0.,0.,1.));
#28155=DIRECTION('ref_axis',(0.17364817766693,-0.984807753012208,0.));
#28156=DIRECTION('center_axis',(0.,0.,1.));
#28157=DIRECTION('ref_axis',(1.,0.,0.));
#28158=DIRECTION('',(-0.582681987722944,0.81270025297353,0.));
#28159=DIRECTION('center_axis',(0.81270025297353,0.582681987722944,0.));
#28160=DIRECTION('ref_axis',(-0.582681987722944,0.81270025297353,0.));
#28161=DIRECTION('',(0.,0.,-1.));
#28162=DIRECTION('',(-0.582681987722944,0.81270025297353,0.));
#28163=DIRECTION('center_axis',(0.,0.,1.));
#28164=DIRECTION('ref_axis',(0.17364817766693,-0.984807753012208,0.));
#28165=DIRECTION('center_axis',(0.,0.,-1.));
#28166=DIRECTION('ref_axis',(1.,0.,0.));
#28167=DIRECTION('center_axis',(-0.81270025297353,0.582681987722944,0.));
#28168=DIRECTION('ref_axis',(-0.582681987722944,-0.81270025297353,0.));
#28169=DIRECTION('',(0.,0.,1.));
#28170=DIRECTION('',(-0.582681987722944,-0.81270025297353,0.));
#28171=DIRECTION('',(0.,0.,1.));
#28172=DIRECTION('',(-0.582681987722944,-0.81270025297353,0.));
#28173=DIRECTION('center_axis',(0.,0.,1.));
#28174=DIRECTION('ref_axis',(-0.17364817766693,-0.984807753012208,0.));
#28175=DIRECTION('center_axis',(0.,0.,1.));
#28176=DIRECTION('ref_axis',(1.,0.,0.));
#28177=DIRECTION('',(-0.269582107125302,0.962977407584353,0.));
#28178=DIRECTION('center_axis',(0.962977407584354,0.269582107125302,0.));
#28179=DIRECTION('ref_axis',(-0.269582107125302,0.962977407584353,0.));
#28180=DIRECTION('',(0.,0.,-1.));
#28181=DIRECTION('',(-0.269582107125302,0.962977407584353,0.));
#28182=DIRECTION('center_axis',(0.,0.,1.));
#28183=DIRECTION('ref_axis',(-0.17364817766693,-0.984807753012208,0.));
#28184=DIRECTION('center_axis',(0.,0.,-1.));
#28185=DIRECTION('ref_axis',(1.,0.,0.));
#28186=DIRECTION('center_axis',(-0.564399453675779,0.82550182113093,0.));
#28187=DIRECTION('ref_axis',(-0.82550182113093,-0.564399453675779,0.));
#28188=DIRECTION('',(0.,0.,1.));
#28189=DIRECTION('',(-0.82550182113093,-0.564399453675779,0.));
#28190=DIRECTION('',(0.,0.,1.));
#28191=DIRECTION('',(-0.82550182113093,-0.564399453675779,0.));
#28192=DIRECTION('center_axis',(0.,0.,1.));
#28193=DIRECTION('ref_axis',(-0.5,-0.866025403784438,0.));
#28194=DIRECTION('center_axis',(0.,0.,1.));
#28195=DIRECTION('ref_axis',(1.,0.,0.));
#28196=DIRECTION('',(0.0760333541998194,0.997105274807593,0.));
#28197=DIRECTION('center_axis',(0.997105274807593,-0.0760333541998194,0.));
#28198=DIRECTION('ref_axis',(0.0760333541998194,0.997105274807593,0.));
#28199=DIRECTION('',(0.,0.,-1.));
#28200=DIRECTION('',(0.0760333541998194,0.997105274807593,0.));
#28201=DIRECTION('center_axis',(0.,0.,1.));
#28202=DIRECTION('ref_axis',(-0.5,-0.866025403784438,0.));
#28203=DIRECTION('center_axis',(0.,0.,-1.));
#28204=DIRECTION('ref_axis',(1.,0.,0.));
#28205=DIRECTION('center_axis',(-0.248023750615927,0.968753951801183,0.));
#28206=DIRECTION('ref_axis',(-0.968753951801183,-0.248023750615927,0.));
#28207=DIRECTION('',(0.,0.,1.));
#28208=DIRECTION('',(-0.968753951801183,-0.248023750615927,0.));
#28209=DIRECTION('',(0.,0.,1.));
#28210=DIRECTION('',(-0.968753951801183,-0.248023750615927,0.));
#28211=DIRECTION('center_axis',(0.,0.,1.));
#28212=DIRECTION('ref_axis',(-0.766044443118978,-0.642787609686539,0.));
#28213=DIRECTION('center_axis',(0.,0.,1.));
#28214=DIRECTION('ref_axis',(1.,0.,0.));
#28215=DIRECTION('',(0.412478070875644,0.910967530182447,0.));
#28216=DIRECTION('center_axis',(0.910967530182447,-0.412478070875644,0.));
#28217=DIRECTION('ref_axis',(0.412478070875644,0.910967530182447,0.));
#28218=DIRECTION('',(0.,0.,-1.));
#28219=DIRECTION('',(0.412478070875644,0.910967530182447,0.));
#28220=DIRECTION('center_axis',(0.,0.,1.));
#28221=DIRECTION('ref_axis',(-0.766044443118978,-0.642787609686539,0.));
#28222=DIRECTION('center_axis',(0.,0.,-1.));
#28223=DIRECTION('ref_axis',(1.,0.,0.));
#28224=DIRECTION('center_axis',(0.0982672772089174,0.995160058598588,0.));
#28225=DIRECTION('ref_axis',(-0.995160058598588,0.0982672772089174,0.));
#28226=DIRECTION('',(0.,0.,1.));
#28227=DIRECTION('',(-0.995160058598588,0.0982672772089174,0.));
#28228=DIRECTION('',(0.,0.,1.));
#28229=DIRECTION('',(-0.995160058598588,0.0982672772089174,0.));
#28230=DIRECTION('center_axis',(0.,0.,1.));
#28231=DIRECTION('ref_axis',(-0.939692620785908,-0.342020143325669,0.));
#28232=DIRECTION('center_axis',(0.,0.,1.));
#28233=DIRECTION('ref_axis',(1.,0.,0.));
#28234=DIRECTION('',(0.699171844675881,0.714953656968426,0.));
#28235=DIRECTION('center_axis',(0.714953656968426,-0.699171844675881,0.));
#28236=DIRECTION('ref_axis',(0.699171844675881,0.714953656968426,0.));
#28237=DIRECTION('',(0.,0.,-1.));
#28238=DIRECTION('',(0.699171844675881,0.714953656968426,0.));
#28239=DIRECTION('center_axis',(0.,0.,1.));
#28240=DIRECTION('ref_axis',(-0.939692620785908,-0.342020143325669,0.));
#28241=DIRECTION('center_axis',(0.,0.,-1.));
#28242=DIRECTION('ref_axis',(1.,0.,0.));
#28243=DIRECTION('center_axis',(0.432705821131813,0.901535175330749,0.));
#28244=DIRECTION('ref_axis',(-0.901535175330748,0.432705821131813,0.));
#28245=DIRECTION('',(0.,0.,1.));
#28246=DIRECTION('',(-0.901535175330748,0.432705821131813,0.));
#28247=DIRECTION('',(0.,0.,1.));
#28248=DIRECTION('',(-0.901535175330748,0.432705821131813,0.));
#28249=DIRECTION('center_axis',(0.,0.,1.));
#28250=DIRECTION('ref_axis',(-1.,5.55111512312578E-17,0.));
#28251=DIRECTION('center_axis',(0.,0.,1.));
#28252=DIRECTION('ref_axis',(1.,0.,0.));
#28253=DIRECTION('',(0.901535175330749,0.432705821131813,0.));
#28254=DIRECTION('center_axis',(0.,0.,1.));
#28255=DIRECTION('ref_axis',(1.,0.,0.));
#28256=DIRECTION('center_axis',(0.432705821131813,-0.901535175330749,0.));
#28257=DIRECTION('ref_axis',(0.901535175330749,0.432705821131813,0.));
#28258=DIRECTION('',(0.,0.,-1.));
#28259=DIRECTION('',(0.901535175330749,0.432705821131813,0.));
#28260=DIRECTION('center_axis',(0.,0.,1.));
#28261=DIRECTION('ref_axis',(-1.,5.55111512312578E-17,0.));
#28262=DIRECTION('center_axis',(0.,0.,-1.));
#28263=DIRECTION('ref_axis',(1.,0.,0.));
#28264=DIRECTION('center_axis',(0.,0.,-1.));
#28265=DIRECTION('ref_axis',(1.,0.,0.));
#28266=DIRECTION('center_axis',(0.714953656968426,0.699171844675881,0.));
#28267=DIRECTION('ref_axis',(-0.699171844675881,0.714953656968426,0.));
#28268=DIRECTION('',(0.,0.,1.));
#28269=DIRECTION('',(-0.699171844675881,0.714953656968426,0.));
#28270=DIRECTION('',(0.,0.,1.));
#28271=DIRECTION('',(-0.699171844675881,0.714953656968426,0.));
#28272=DIRECTION('center_axis',(0.,0.,1.));
#28273=DIRECTION('ref_axis',(-0.939692620785908,0.342020143325669,0.));
#28274=DIRECTION('center_axis',(0.,0.,1.));
#28275=DIRECTION('ref_axis',(1.,0.,0.));
#28276=DIRECTION('',(0.995160058598588,0.0982672772089171,0.));
#28277=DIRECTION('center_axis',(0.0982672772089171,-0.995160058598588,0.));
#28278=DIRECTION('ref_axis',(0.995160058598588,0.0982672772089171,0.));
#28279=DIRECTION('',(0.,0.,-1.));
#28280=DIRECTION('',(0.995160058598588,0.0982672772089171,0.));
#28281=DIRECTION('center_axis',(0.,0.,1.));
#28282=DIRECTION('ref_axis',(-0.939692620785908,0.342020143325669,0.));
#28283=DIRECTION('center_axis',(0.,0.,-1.));
#28284=DIRECTION('ref_axis',(1.,0.,0.));
#28285=DIRECTION('center_axis',(0.910967530182447,0.412478070875644,0.));
#28286=DIRECTION('ref_axis',(-0.412478070875644,0.910967530182447,0.));
#28287=DIRECTION('',(0.,0.,1.));
#28288=DIRECTION('',(-0.412478070875644,0.910967530182447,0.));
#28289=DIRECTION('',(0.,0.,1.));
#28290=DIRECTION('',(-0.412478070875644,0.910967530182447,0.));
#28291=DIRECTION('center_axis',(0.,0.,1.));
#28292=DIRECTION('ref_axis',(-0.766044443118978,0.642787609686539,0.));
#28293=DIRECTION('center_axis',(0.,0.,1.));
#28294=DIRECTION('ref_axis',(1.,0.,0.));
#28295=DIRECTION('',(0.968753951801183,-0.248023750615928,0.));
#28296=DIRECTION('center_axis',(-0.248023750615928,-0.968753951801183,0.));
#28297=DIRECTION('ref_axis',(0.968753951801183,-0.248023750615928,0.));
#28298=DIRECTION('',(0.,0.,-1.));
#28299=DIRECTION('',(0.968753951801183,-0.248023750615928,0.));
#28300=DIRECTION('center_axis',(0.,0.,1.));
#28301=DIRECTION('ref_axis',(-0.766044443118978,0.642787609686539,0.));
#28302=DIRECTION('center_axis',(0.,0.,-1.));
#28303=DIRECTION('ref_axis',(1.,0.,0.));
#28304=DIRECTION('center_axis',(0.997105274807593,0.0760333541998187,0.));
#28305=DIRECTION('ref_axis',(-0.0760333541998187,0.997105274807593,0.));
#28306=DIRECTION('',(0.,0.,1.));
#28307=DIRECTION('',(-0.0760333541998187,0.997105274807593,0.));
#28308=DIRECTION('',(0.,0.,1.));
#28309=DIRECTION('',(-0.0760333541998187,0.997105274807593,0.));
#28310=DIRECTION('center_axis',(0.,0.,1.));
#28311=DIRECTION('ref_axis',(-0.5,0.866025403784439,0.));
#28312=DIRECTION('center_axis',(0.,0.,1.));
#28313=DIRECTION('ref_axis',(1.,0.,0.));
#28314=DIRECTION('',(0.82550182113093,-0.56439945367578,0.));
#28315=DIRECTION('center_axis',(-0.56439945367578,-0.82550182113093,0.));
#28316=DIRECTION('ref_axis',(0.82550182113093,-0.56439945367578,0.));
#28317=DIRECTION('',(0.,0.,-1.));
#28318=DIRECTION('',(0.82550182113093,-0.56439945367578,0.));
#28319=DIRECTION('center_axis',(0.,0.,1.));
#28320=DIRECTION('ref_axis',(-0.5,0.866025403784439,0.));
#28321=DIRECTION('center_axis',(0.,0.,-1.));
#28322=DIRECTION('ref_axis',(1.,0.,0.));
#28323=DIRECTION('center_axis',(0.962977407584354,-0.269582107125302,0.));
#28324=DIRECTION('ref_axis',(0.269582107125302,0.962977407584354,0.));
#28325=DIRECTION('',(0.,0.,1.));
#28326=DIRECTION('',(0.269582107125302,0.962977407584354,0.));
#28327=DIRECTION('',(0.,0.,1.));
#28328=DIRECTION('',(0.269582107125302,0.962977407584354,0.));
#28329=DIRECTION('center_axis',(0.,0.,1.));
#28330=DIRECTION('ref_axis',(-0.17364817766693,0.984807753012208,0.));
#28331=DIRECTION('center_axis',(0.,0.,1.));
#28332=DIRECTION('ref_axis',(1.,0.,0.));
#28333=DIRECTION('',(0.582681987722944,-0.81270025297353,0.));
#28334=DIRECTION('center_axis',(-0.81270025297353,-0.582681987722944,0.));
#28335=DIRECTION('ref_axis',(0.582681987722944,-0.81270025297353,0.));
#28336=DIRECTION('',(0.,0.,-1.));
#28337=DIRECTION('',(0.582681987722944,-0.81270025297353,0.));
#28338=DIRECTION('center_axis',(0.,0.,1.));
#28339=DIRECTION('ref_axis',(-0.17364817766693,0.984807753012208,0.));
#28340=DIRECTION('center_axis',(0.,0.,-1.));
#28341=DIRECTION('ref_axis',(1.,0.,0.));
#28342=DIRECTION('center_axis',(0.812700252973529,-0.582681987722944,0.));
#28343=DIRECTION('ref_axis',(0.582681987722944,0.812700252973529,0.));
#28344=DIRECTION('',(0.,0.,1.));
#28345=DIRECTION('',(0.582681987722944,0.812700252973529,0.));
#28346=DIRECTION('',(0.,0.,1.));
#28347=DIRECTION('',(0.582681987722944,0.812700252973529,0.));
#28348=DIRECTION('center_axis',(0.,0.,1.));
#28349=DIRECTION('ref_axis',(0.17364817766693,0.984807753012208,0.));
#28350=DIRECTION('center_axis',(0.,0.,1.));
#28351=DIRECTION('ref_axis',(1.,0.,0.));
#28352=DIRECTION('',(0.269582107125302,-0.962977407584354,0.));
#28353=DIRECTION('center_axis',(-0.962977407584354,-0.269582107125302,0.));
#28354=DIRECTION('ref_axis',(0.269582107125302,-0.962977407584354,0.));
#28355=DIRECTION('',(0.,0.,-1.));
#28356=DIRECTION('',(0.269582107125302,-0.962977407584354,0.));
#28357=DIRECTION('center_axis',(0.,0.,1.));
#28358=DIRECTION('ref_axis',(0.17364817766693,0.984807753012208,0.));
#28359=DIRECTION('center_axis',(0.,0.,-1.));
#28360=DIRECTION('ref_axis',(1.,0.,0.));
#28361=DIRECTION('center_axis',(0.56439945367578,-0.82550182113093,0.));
#28362=DIRECTION('ref_axis',(0.82550182113093,0.56439945367578,0.));
#28363=DIRECTION('',(0.,0.,1.));
#28364=DIRECTION('',(0.82550182113093,0.56439945367578,0.));
#28365=DIRECTION('',(0.,0.,1.));
#28366=DIRECTION('',(0.82550182113093,0.56439945367578,0.));
#28367=DIRECTION('center_axis',(0.,0.,1.));
#28368=DIRECTION('ref_axis',(0.5,0.866025403784439,0.));
#28369=DIRECTION('center_axis',(0.,0.,1.));
#28370=DIRECTION('ref_axis',(1.,0.,0.));
#28371=DIRECTION('',(-0.076033354199819,-0.997105274807593,0.));
#28372=DIRECTION('center_axis',(-0.997105274807593,0.076033354199819,0.));
#28373=DIRECTION('ref_axis',(-0.076033354199819,-0.997105274807593,0.));
#28374=DIRECTION('',(0.,0.,-1.));
#28375=DIRECTION('',(-0.076033354199819,-0.997105274807593,0.));
#28376=DIRECTION('center_axis',(0.,0.,1.));
#28377=DIRECTION('ref_axis',(0.5,0.866025403784439,0.));
#28378=DIRECTION('center_axis',(0.,0.,-1.));
#28379=DIRECTION('ref_axis',(1.,0.,0.));
#28380=DIRECTION('center_axis',(0.248023750615927,-0.968753951801183,0.));
#28381=DIRECTION('ref_axis',(0.968753951801183,0.248023750615927,0.));
#28382=DIRECTION('',(0.,0.,1.));
#28383=DIRECTION('',(0.968753951801183,0.248023750615927,0.));
#28384=DIRECTION('',(0.,0.,1.));
#28385=DIRECTION('',(0.968753951801183,0.248023750615927,0.));
#28386=DIRECTION('center_axis',(0.,0.,1.));
#28387=DIRECTION('ref_axis',(0.766044443118978,0.642787609686539,0.));
#28388=DIRECTION('center_axis',(0.,0.,1.));
#28389=DIRECTION('ref_axis',(1.,0.,0.));
#28390=DIRECTION('',(-0.412478070875644,-0.910967530182447,0.));
#28391=DIRECTION('center_axis',(-0.910967530182447,0.412478070875644,0.));
#28392=DIRECTION('ref_axis',(-0.412478070875644,-0.910967530182447,0.));
#28393=DIRECTION('',(0.,0.,-1.));
#28394=DIRECTION('',(-0.412478070875644,-0.910967530182447,0.));
#28395=DIRECTION('center_axis',(0.,0.,1.));
#28396=DIRECTION('ref_axis',(0.766044443118978,0.642787609686539,0.));
#28397=DIRECTION('center_axis',(0.,0.,-1.));
#28398=DIRECTION('ref_axis',(1.,0.,0.));
#28399=DIRECTION('center_axis',(-0.0982672772089173,-0.995160058598588,
0.));
#28400=DIRECTION('ref_axis',(0.995160058598588,-0.0982672772089173,0.));
#28401=DIRECTION('',(0.,0.,1.));
#28402=DIRECTION('',(0.995160058598588,-0.0982672772089173,0.));
#28403=DIRECTION('',(0.,0.,1.));
#28404=DIRECTION('',(0.995160058598588,-0.0982672772089173,0.));
#28405=DIRECTION('center_axis',(0.,0.,1.));
#28406=DIRECTION('ref_axis',(0.939692620785908,0.342020143325669,0.));
#28407=DIRECTION('center_axis',(0.,0.,1.));
#28408=DIRECTION('ref_axis',(1.,0.,0.));
#28409=DIRECTION('',(-0.699171844675881,-0.714953656968426,0.));
#28410=DIRECTION('center_axis',(-0.714953656968426,0.699171844675881,0.));
#28411=DIRECTION('ref_axis',(-0.699171844675881,-0.714953656968426,0.));
#28412=DIRECTION('',(0.,0.,-1.));
#28413=DIRECTION('',(-0.699171844675881,-0.714953656968426,0.));
#28414=DIRECTION('center_axis',(0.,0.,1.));
#28415=DIRECTION('ref_axis',(0.939692620785908,0.342020143325669,0.));
#28416=DIRECTION('center_axis',(0.,0.,-1.));
#28417=DIRECTION('ref_axis',(1.,0.,0.));
#28418=DIRECTION('center_axis',(-0.432705821131813,-0.901535175330749,0.));
#28419=DIRECTION('ref_axis',(0.901535175330749,-0.432705821131813,0.));
#28420=DIRECTION('',(0.,0.,1.));
#28421=DIRECTION('',(0.901535175330749,-0.432705821131813,0.));
#28422=DIRECTION('',(0.,0.,1.));
#28423=DIRECTION('',(0.901535175330749,-0.432705821131813,0.));
#28424=DIRECTION('center_axis',(0.,0.,1.));
#28425=DIRECTION('ref_axis',(1.,0.,0.));
#28426=DIRECTION('center_axis',(0.,0.,1.));
#28427=DIRECTION('ref_axis',(1.,0.,0.));
#28428=DIRECTION('',(-0.901535175330749,-0.432705821131813,0.));
#28429=DIRECTION('center_axis',(-0.432705821131813,0.901535175330749,0.));
#28430=DIRECTION('ref_axis',(-0.901535175330749,-0.432705821131813,0.));
#28431=DIRECTION('',(0.,0.,-1.));
#28432=DIRECTION('',(-0.901535175330749,-0.432705821131813,0.));
#28433=DIRECTION('center_axis',(0.,0.,1.));
#28434=DIRECTION('ref_axis',(1.,0.,0.));
#28435=DIRECTION('center_axis',(0.,0.,-1.));
#28436=DIRECTION('ref_axis',(1.,0.,0.));
#28437=DIRECTION('center_axis',(0.,0.,1.));
#28438=DIRECTION('ref_axis',(1.,0.,0.));
#28439=DIRECTION('center_axis',(0.,0.,-1.));
#28440=DIRECTION('ref_axis',(1.,0.,0.));
#28441=DIRECTION('',(0.,0.,1.));
#28442=DIRECTION('center_axis',(0.,0.,1.));
#28443=DIRECTION('ref_axis',(1.,0.,0.));
#28444=DIRECTION('center_axis',(0.,0.,1.));
#28445=DIRECTION('ref_axis',(1.,0.,0.));
#28446=DIRECTION('center_axis',(0.,0.,1.));
#28447=DIRECTION('ref_axis',(1.,0.,0.));
#28448=DIRECTION('',(0.,0.,1.));
#28449=DIRECTION('center_axis',(0.,0.,1.));
#28450=DIRECTION('ref_axis',(1.,0.,0.));
#28451=DIRECTION('center_axis',(0.,0.,1.));
#28452=DIRECTION('ref_axis',(1.,0.,0.));
#28453=DIRECTION('center_axis',(0.,0.,-1.));
#28454=DIRECTION('ref_axis',(-1.,0.,0.));
#28455=DIRECTION('center_axis',(0.,0.,1.));
#28456=DIRECTION('ref_axis',(1.,0.,0.));
#28457=DIRECTION('center_axis',(0.,0.,-1.));
#28458=DIRECTION('ref_axis',(-1.,0.,0.));
#28459=DIRECTION('center_axis',(0.,0.,1.));
#28460=DIRECTION('ref_axis',(1.,0.,0.));
#28461=DIRECTION('center_axis',(0.,0.,1.));
#28462=DIRECTION('ref_axis',(1.,0.,0.));
#28463=DIRECTION('',(0.707106781186548,8.65956056235494E-17,-0.707106781186547));
#28464=DIRECTION('center_axis',(0.,0.,1.));
#28465=DIRECTION('ref_axis',(1.,0.,0.));
#28466=DIRECTION('',(0.,0.,-1.));
#28467=DIRECTION('center_axis',(0.,0.,1.));
#28468=DIRECTION('ref_axis',(1.,0.,0.));
#28469=DIRECTION('center_axis',(0.,0.,1.));
#28470=DIRECTION('ref_axis',(1.,0.,0.));
#28471=DIRECTION('center_axis',(0.,0.,1.));
#28472=DIRECTION('ref_axis',(1.,0.,0.));
#28473=DIRECTION('center_axis',(0.,0.,1.));
#28474=DIRECTION('ref_axis',(1.,0.,0.));
#28475=DIRECTION('',(0.,0.,-1.));
#28476=DIRECTION('',(0.,0.,-1.));
#28477=DIRECTION('center_axis',(0.,0.,1.));
#28478=DIRECTION('ref_axis',(1.,0.,0.));
#28479=DIRECTION('center_axis',(0.,0.,1.));
#28480=DIRECTION('ref_axis',(1.,0.,0.));
#28481=DIRECTION('center_axis',(0.,0.,1.));
#28482=DIRECTION('ref_axis',(1.,0.,0.));
#28483=DIRECTION('center_axis',(0.,0.,1.));
#28484=DIRECTION('ref_axis',(1.,0.,0.));
#28485=DIRECTION('',(0.,0.,-1.));
#28486=DIRECTION('center_axis',(0.,0.,1.));
#28487=DIRECTION('ref_axis',(1.,0.,0.));
#28488=DIRECTION('axis',(0.,0.,1.));
#28489=DIRECTION('refdir',(1.,0.,0.));
#28490=DIRECTION('center_axis',(0.,0.,1.));
#28491=DIRECTION('ref_axis',(1.,0.,0.));
#28492=DIRECTION('center_axis',(0.,0.,1.));
#28493=DIRECTION('ref_axis',(1.,0.,0.));
#28494=DIRECTION('',(0.,0.,-1.));
#28495=DIRECTION('center_axis',(0.,0.,1.));
#28496=DIRECTION('ref_axis',(1.,0.,0.));
#28497=DIRECTION('center_axis',(0.,0.,-1.));
#28498=DIRECTION('ref_axis',(-1.,0.,0.));
#28499=DIRECTION('center_axis',(0.,0.,1.));
#28500=DIRECTION('ref_axis',(1.,0.,0.));
#28501=DIRECTION('center_axis',(0.,0.,1.));
#28502=DIRECTION('ref_axis',(1.,0.,0.));
#28503=DIRECTION('center_axis',(0.,0.,1.));
#28504=DIRECTION('ref_axis',(1.,0.,0.));
#28505=DIRECTION('',(0.,0.,-1.));
#28506=DIRECTION('center_axis',(0.,0.,1.));
#28507=DIRECTION('ref_axis',(1.,0.,0.));
#28508=DIRECTION('axis',(0.,0.,1.));
#28509=DIRECTION('refdir',(1.,0.,0.));
#28510=DIRECTION('center_axis',(0.,0.,-1.));
#28511=DIRECTION('ref_axis',(1.,0.,0.));
#28512=DIRECTION('center_axis',(0.,0.,-1.));
#28513=DIRECTION('ref_axis',(1.,0.,0.));
#28514=DIRECTION('',(0.70710678118655,-8.65956056235497E-17,0.707106781186545));
#28515=DIRECTION('center_axis',(0.,0.,1.));
#28516=DIRECTION('ref_axis',(1.,0.,0.));
#28517=DIRECTION('center_axis',(0.,0.,1.));
#28518=DIRECTION('ref_axis',(1.,0.,0.));
#28519=DIRECTION('',(0.,0.,1.));
#28520=DIRECTION('center_axis',(0.,0.,-1.));
#28521=DIRECTION('ref_axis',(-1.,0.,0.));
#28522=DIRECTION('center_axis',(0.,0.,-1.));
#28523=DIRECTION('ref_axis',(-1.,0.,0.));
#28524=DIRECTION('center_axis',(0.,0.,1.));
#28525=DIRECTION('ref_axis',(1.,0.,0.));
#28526=DIRECTION('',(1.,0.,0.));
#28527=DIRECTION('center_axis',(0.,0.,1.));
#28528=DIRECTION('ref_axis',(-0.707106781186547,-0.707106781186548,0.));
#28529=DIRECTION('',(0.,-1.,0.));
#28530=DIRECTION('center_axis',(0.,0.,1.));
#28531=DIRECTION('ref_axis',(-0.707106781186548,0.707106781186547,0.));
#28532=DIRECTION('',(-1.,0.,0.));
#28533=DIRECTION('',(0.,-1.,0.));
#28534=DIRECTION('center_axis',(0.,0.,1.));
#28535=DIRECTION('ref_axis',(-1.,0.,0.));
#28536=DIRECTION('center_axis',(0.,0.,1.));
#28537=DIRECTION('ref_axis',(-1.,0.,0.));
#28538=DIRECTION('',(-0.70710678118655,-8.65956056235496E-17,-0.707106781186545));
#28539=DIRECTION('center_axis',(0.,0.,1.));
#28540=DIRECTION('ref_axis',(1.,0.,0.));
#28541=DIRECTION('center_axis',(0.,0.,-1.));
#28542=DIRECTION('ref_axis',(0.707106781186549,-0.707106781186546,0.));
#28543=DIRECTION('',(0.,-1.,0.));
#28544=DIRECTION('center_axis',(0.,0.,-1.));
#28545=DIRECTION('ref_axis',(0.707106781186546,0.707106781186549,0.));
#28546=DIRECTION('',(1.,0.,0.));
#28547=DIRECTION('center_axis',(0.,0.,-1.));
#28548=DIRECTION('ref_axis',(-0.707106781186548,0.707106781186547,0.));
#28549=DIRECTION('',(0.,1.,0.));
#28550=DIRECTION('center_axis',(0.,0.,-1.));
#28551=DIRECTION('ref_axis',(-0.707106781186547,-0.707106781186548,0.));
#28552=DIRECTION('',(-1.,0.,0.));
#28553=DIRECTION('center_axis',(0.,0.707106781186547,-0.707106781186548));
#28554=DIRECTION('ref_axis',(-1.,0.,0.));
#28555=DIRECTION('',(0.,0.707106781186548,0.707106781186547));
#28556=DIRECTION('',(0.,0.707106781186548,0.707106781186547));
#28557=DIRECTION('',(1.,0.,0.));
#28558=DIRECTION('center_axis',(0.,0.,1.));
#28559=DIRECTION('ref_axis',(-0.707106781186548,0.707106781186547,0.));
#28560=DIRECTION('',(-0.70710678118654,0.,0.707106781186555));
#28561=DIRECTION('center_axis',(0.,0.,-1.));
#28562=DIRECTION('ref_axis',(-0.707106781186548,0.707106781186547,0.));
#28563=DIRECTION('center_axis',(-0.707106781186545,0.,-0.70710678118655));
#28564=DIRECTION('ref_axis',(-0.70710678118655,0.,0.707106781186545));
#28565=DIRECTION('',(-0.70710678118655,0.,0.707106781186545));
#28566=DIRECTION('',(0.,1.,0.));
#28567=DIRECTION('center_axis',(0.,0.,1.));
#28568=DIRECTION('ref_axis',(-0.707106781186547,-0.707106781186548,0.));
#28569=DIRECTION('',(0.,-0.707106781186546,0.707106781186549));
#28570=DIRECTION('center_axis',(0.,0.,-1.));
#28571=DIRECTION('ref_axis',(-0.707106781186547,-0.707106781186548,0.));
#28572=DIRECTION('center_axis',(0.,-0.707106781186547,-0.707106781186548));
#28573=DIRECTION('ref_axis',(-1.,0.,0.));
#28574=DIRECTION('',(0.,0.707106781186548,-0.707106781186547));
#28575=DIRECTION('',(-1.,0.,0.));
#28576=DIRECTION('center_axis',(-0.707106781186545,0.,-0.70710678118655));
#28577=DIRECTION('ref_axis',(-0.70710678118655,0.,0.707106781186545));
#28578=DIRECTION('',(0.,1.,0.));
#28579=DIRECTION('',(0.577350269189629,-0.577350269189625,-0.577350269189624));
#28580=DIRECTION('',(0.,-1.,0.));
#28581=DIRECTION('',(-0.577350269189629,-0.577350269189625,0.577350269189624));
#28582=DIRECTION('center_axis',(0.,-0.707106781186547,-0.707106781186548));
#28583=DIRECTION('ref_axis',(-1.,0.,0.));
#28584=DIRECTION('',(1.,0.,0.));
#28585=DIRECTION('',(0.,-0.707106781186548,0.707106781186547));
#28586=DIRECTION('',(-1.,0.,0.));
#28587=DIRECTION('center_axis',(0.,0.,1.));
#28588=DIRECTION('ref_axis',(0.707106781186549,-0.707106781186546,0.));
#28589=DIRECTION('',(0.707106781186561,0.,0.707106781186534));
#28590=DIRECTION('center_axis',(0.,0.,-1.));
#28591=DIRECTION('ref_axis',(0.707106781186549,-0.707106781186546,0.));
#28592=DIRECTION('center_axis',(0.,0.,1.));
#28593=DIRECTION('ref_axis',(0.707106781186549,-0.707106781186546,0.));
#28594=DIRECTION('center_axis',(0.707106781186545,0.,-0.70710678118655));
#28595=DIRECTION('ref_axis',(-0.70710678118655,0.,-0.707106781186545));
#28596=DIRECTION('',(0.70710678118655,6.54205191118237E-16,0.707106781186545));
#28597=DIRECTION('',(0.,-1.,0.));
#28598=DIRECTION('',(0.,1.,0.));
#28599=DIRECTION('center_axis',(0.,0.,1.));
#28600=DIRECTION('ref_axis',(0.707106781186546,0.707106781186549,0.));
#28601=DIRECTION('',(0.,0.707106781186552,0.707106781186543));
#28602=DIRECTION('center_axis',(0.,0.,-1.));
#28603=DIRECTION('ref_axis',(0.707106781186546,0.707106781186549,0.));
#28604=DIRECTION('center_axis',(0.,0.,1.));
#28605=DIRECTION('ref_axis',(0.707106781186546,0.707106781186549,0.));
#28606=DIRECTION('center_axis',(0.,0.707106781186547,-0.707106781186548));
#28607=DIRECTION('ref_axis',(-1.,0.,0.));
#28608=DIRECTION('',(1.,0.,0.));
#28609=DIRECTION('',(-1.,0.,0.));
#28610=DIRECTION('center_axis',(0.,0.,1.));
#28611=DIRECTION('ref_axis',(0.707106781186546,0.707106781186549,0.));
#28612=DIRECTION('',(0.,0.,1.));
#28613=DIRECTION('center_axis',(0.,0.,1.));
#28614=DIRECTION('ref_axis',(0.707106781186546,0.707106781186549,0.));
#28615=DIRECTION('',(0.,0.,-1.));
#28616=DIRECTION('center_axis',(0.,1.,0.));
#28617=DIRECTION('ref_axis',(-1.,0.,0.));
#28618=DIRECTION('',(0.,0.,-1.));
#28619=DIRECTION('',(-1.,0.,0.));
#28620=DIRECTION('',(0.,0.,1.));
#28621=DIRECTION('center_axis',(-1.,0.,0.));
#28622=DIRECTION('ref_axis',(0.,-1.,0.));
#28623=DIRECTION('',(0.,0.,1.));
#28624=DIRECTION('center_axis',(0.,0.,1.));
#28625=DIRECTION('ref_axis',(1.,0.,0.));
#28626=DIRECTION('center_axis',(0.,0.,-1.));
#28627=DIRECTION('ref_axis',(0.707106781186549,-0.707106781186546,0.));
#28628=DIRECTION('',(0.,-0.70710678118655,-0.707106781186545));
#28629=DIRECTION('center_axis',(0.,0.,1.));
#28630=DIRECTION('ref_axis',(0.707106781186549,-0.707106781186546,0.));
#28631=DIRECTION('',(-0.707106781186561,0.,0.707106781186534));
#28632=DIRECTION('center_axis',(0.,-0.707106781186548,0.707106781186548));
#28633=DIRECTION('ref_axis',(1.,0.,0.));
#28634=DIRECTION('',(0.,-0.707106781186548,-0.707106781186548));
#28635=DIRECTION('',(1.,0.,0.));
#28636=DIRECTION('center_axis',(0.,0.,-1.));
#28637=DIRECTION('ref_axis',(-0.707106781186547,-0.707106781186548,0.));
#28638=DIRECTION('',(-0.70710678118654,0.,-0.707106781186555));
#28639=DIRECTION('center_axis',(0.,0.,1.));
#28640=DIRECTION('ref_axis',(-0.707106781186547,-0.707106781186548,0.));
#28641=DIRECTION('center_axis',(-0.70710678118655,0.,0.707106781186545));
#28642=DIRECTION('ref_axis',(0.707106781186545,0.,0.70710678118655));
#28643=DIRECTION('',(-0.707106781186545,0.,-0.70710678118655));
#28644=DIRECTION('',(0.,-1.,0.));
#28645=DIRECTION('center_axis',(0.,0.,-1.));
#28646=DIRECTION('ref_axis',(-0.707106781186548,0.707106781186547,0.));
#28647=DIRECTION('',(0.,0.707106781186544,-0.707106781186551));
#28648=DIRECTION('center_axis',(0.,0.,1.));
#28649=DIRECTION('ref_axis',(-0.707106781186548,0.707106781186547,0.));
#28650=DIRECTION('center_axis',(0.,0.707106781186548,0.707106781186548));
#28651=DIRECTION('ref_axis',(1.,0.,0.));
#28652=DIRECTION('',(0.,0.707106781186548,-0.707106781186548));
#28653=DIRECTION('center_axis',(0.,0.,-1.));
#28654=DIRECTION('ref_axis',(0.707106781186546,0.707106781186549,0.));
#28655=DIRECTION('',(0.70710678118655,6.54205191118237E-16,-0.707106781186545));
#28656=DIRECTION('center_axis',(0.707106781186545,0.,0.70710678118655));
#28657=DIRECTION('ref_axis',(0.70710678118655,0.,-0.707106781186545));
#28658=DIRECTION('',(0.,1.,0.));
#28659=DIRECTION('center_axis',(1.,0.,0.));
#28660=DIRECTION('ref_axis',(0.,1.,0.));
#28661=DIRECTION('',(0.,0.,1.));
#28662=DIRECTION('center_axis',(0.,0.,1.));
#28663=DIRECTION('ref_axis',(0.707106781186549,-0.707106781186546,0.));
#28664=DIRECTION('',(0.,0.,-1.));
#28665=DIRECTION('center_axis',(0.,-1.,0.));
#28666=DIRECTION('ref_axis',(1.,0.,0.));
#28667=DIRECTION('',(0.,0.,1.));
#28668=DIRECTION('center_axis',(0.,0.,1.));
#28669=DIRECTION('ref_axis',(-0.707106781186547,-0.707106781186548,0.));
#28670=DIRECTION('',(0.,0.,-1.));
#28671=DIRECTION('center_axis',(-1.,0.,0.));
#28672=DIRECTION('ref_axis',(0.,-1.,0.));
#28673=DIRECTION('',(0.,0.,1.));
#28674=DIRECTION('center_axis',(0.,0.,1.));
#28675=DIRECTION('ref_axis',(-0.707106781186548,0.707106781186547,0.));
#28676=DIRECTION('axis',(0.,0.,1.));
#28677=DIRECTION('refdir',(1.,0.,0.));
#28678=DIRECTION('center_axis',(0.,0.,1.));
#28679=DIRECTION('ref_axis',(1.,0.,0.));
#28680=DIRECTION('center_axis',(0.,0.,1.));
#28681=DIRECTION('ref_axis',(1.,0.,0.));
#28682=DIRECTION('',(0.,0.,-1.));
#28683=DIRECTION('center_axis',(0.,0.,1.));
#28684=DIRECTION('ref_axis',(1.,0.,0.));
#28685=DIRECTION('center_axis',(0.,0.,-1.));
#28686=DIRECTION('ref_axis',(1.,0.,0.));
#28687=DIRECTION('',(-0.994505452921406,-1.21791791965479E-16,-0.104684784518043));
#28688=DIRECTION('center_axis',(0.,0.,1.));
#28689=DIRECTION('ref_axis',(1.,0.,0.));
#28690=DIRECTION('center_axis',(0.,0.,1.));
#28691=DIRECTION('ref_axis',(1.,0.,0.));
#28692=DIRECTION('center_axis',(0.,0.,1.));
#28693=DIRECTION('ref_axis',(1.,0.,0.));
#28694=DIRECTION('',(0.,0.,-1.));
#28695=DIRECTION('center_axis',(0.,0.,-1.));
#28696=DIRECTION('ref_axis',(1.,0.,0.));
#28697=DIRECTION('',(-0.994505452921406,-1.21791791965479E-16,-0.104684784518043));
#28698=DIRECTION('axis',(0.,0.,1.));
#28699=DIRECTION('refdir',(1.,0.,0.));
#28700=DIRECTION('center_axis',(0.,0.,1.));
#28701=DIRECTION('ref_axis',(1.,0.,0.));
#28702=DIRECTION('',(0.,0.,-1.));
#28703=DIRECTION('center_axis',(0.,0.,-1.));
#28704=DIRECTION('ref_axis',(1.,0.,0.));
#28705=DIRECTION('',(0.,0.,-1.));
#28706=DIRECTION('center_axis',(0.,0.,1.));
#28707=DIRECTION('ref_axis',(1.,0.,0.));
#28708=DIRECTION('center_axis',(0.,0.,-1.));
#28709=DIRECTION('ref_axis',(1.,0.,0.));
#28710=DIRECTION('center_axis',(0.,0.,1.));
#28711=DIRECTION('ref_axis',(1.,0.,0.));
#28712=DIRECTION('',(0.,0.,-1.));
#28713=DIRECTION('center_axis',(0.,0.,1.));
#28714=DIRECTION('ref_axis',(1.,0.,0.));
#28715=DIRECTION('',(0.,0.,-1.));
#28716=DIRECTION('center_axis',(0.,0.,1.));
#28717=DIRECTION('ref_axis',(1.,0.,0.));
#28718=DIRECTION('',(0.,0.,-1.));
#28719=DIRECTION('center_axis',(0.,0.,1.));
#28720=DIRECTION('ref_axis',(1.,0.,0.));
#28721=DIRECTION('',(0.,0.,-1.));
#28722=DIRECTION('center_axis',(0.,0.,1.));
#28723=DIRECTION('ref_axis',(1.,0.,0.));
#28724=DIRECTION('',(0.,0.,-1.));
#28725=DIRECTION('center_axis',(0.,0.,1.));
#28726=DIRECTION('ref_axis',(1.,0.,0.));
#28727=DIRECTION('',(0.,0.,-1.));
#28728=DIRECTION('center_axis',(0.,0.,1.));
#28729=DIRECTION('ref_axis',(1.,0.,0.));
#28730=DIRECTION('',(0.,0.,-1.));
#28731=DIRECTION('center_axis',(0.,0.,1.));
#28732=DIRECTION('ref_axis',(1.,0.,0.));
#28733=DIRECTION('',(0.,0.,-1.));
#28734=DIRECTION('center_axis',(0.,0.,1.));
#28735=DIRECTION('ref_axis',(1.,0.,0.));
#28736=DIRECTION('',(0.,0.,-1.));
#28737=DIRECTION('center_axis',(0.,0.,1.));
#28738=DIRECTION('ref_axis',(1.,0.,0.));
#28739=DIRECTION('',(0.,0.,-1.));
#28740=DIRECTION('center_axis',(0.,0.,1.));
#28741=DIRECTION('ref_axis',(1.,0.,0.));
#28742=DIRECTION('',(0.,0.,-1.));
#28743=DIRECTION('center_axis',(0.,0.,1.));
#28744=DIRECTION('ref_axis',(1.,0.,0.));
#28745=DIRECTION('',(0.,0.,-1.));
#28746=DIRECTION('center_axis',(0.,0.,1.));
#28747=DIRECTION('ref_axis',(1.,0.,0.));
#28748=DIRECTION('',(0.,0.,-1.));
#28749=DIRECTION('center_axis',(0.,0.,1.));
#28750=DIRECTION('ref_axis',(-0.266010203854043,-0.963970212945157,0.));
#28751=DIRECTION('',(0.,0.,1.));
#28752=DIRECTION('center_axis',(0.,0.,1.));
#28753=DIRECTION('ref_axis',(1.,8.51023079448757E-14,0.));
#28754=DIRECTION('center_axis',(0.,0.,1.));
#28755=DIRECTION('ref_axis',(1.,8.51023079448757E-14,0.));
#28756=DIRECTION('',(0.,0.,1.));
#28757=DIRECTION('center_axis',(0.,0.,1.));
#28758=DIRECTION('ref_axis',(1.,8.51023079448757E-14,0.));
#28759=DIRECTION('',(0.,0.,1.));
#28760=DIRECTION('center_axis',(0.,0.,1.));
#28761=DIRECTION('ref_axis',(1.,8.51023079448757E-14,0.));
#28762=DIRECTION('',(0.,0.,1.));
#28763=DIRECTION('center_axis',(0.,0.,1.));
#28764=DIRECTION('ref_axis',(1.,8.51023079448757E-14,0.));
#28765=DIRECTION('',(0.,0.,1.));
#28766=DIRECTION('center_axis',(0.,0.,1.));
#28767=DIRECTION('ref_axis',(1.,8.51023079448757E-14,0.));
#28768=DIRECTION('',(0.,0.,1.));
#28769=DIRECTION('center_axis',(0.,0.,1.));
#28770=DIRECTION('ref_axis',(1.,8.51023079448757E-14,0.));
#28771=DIRECTION('',(0.,0.,1.));
#28772=DIRECTION('center_axis',(0.,0.,1.));
#28773=DIRECTION('ref_axis',(1.,8.51023079448757E-14,0.));
#28774=DIRECTION('',(0.,0.,1.));
#28775=DIRECTION('center_axis',(0.,0.,1.));
#28776=DIRECTION('ref_axis',(1.,8.51023079448757E-14,0.));
#28777=DIRECTION('',(0.,0.,1.));
#28778=DIRECTION('center_axis',(0.,0.,1.));
#28779=DIRECTION('ref_axis',(1.,8.51023079448757E-14,0.));
#28780=DIRECTION('',(0.,0.,1.));
#28781=DIRECTION('center_axis',(0.,0.,1.));
#28782=DIRECTION('ref_axis',(1.,8.51023079448757E-14,0.));
#28783=DIRECTION('',(0.,0.,1.));
#28784=DIRECTION('center_axis',(0.,0.,1.));
#28785=DIRECTION('ref_axis',(1.,8.51023079448757E-14,0.));
#28786=DIRECTION('',(0.,0.,1.));
#28787=DIRECTION('center_axis',(0.,0.,1.));
#28788=DIRECTION('ref_axis',(1.,8.51023079448757E-14,0.));
#28789=DIRECTION('',(0.,0.,1.));
#28790=DIRECTION('center_axis',(0.,0.,1.));
#28791=DIRECTION('ref_axis',(1.,8.51023079448757E-14,0.));
#28792=DIRECTION('',(0.,0.,1.));
#28793=DIRECTION('center_axis',(0.,0.,1.));
#28794=DIRECTION('ref_axis',(1.,8.51023079448757E-14,0.));
#28795=DIRECTION('',(0.,0.,1.));
#28796=DIRECTION('center_axis',(0.,0.,-1.));
#28797=DIRECTION('ref_axis',(1.,8.51023079448757E-14,0.));
#28798=DIRECTION('center_axis',(0.,0.,1.));
#28799=DIRECTION('ref_axis',(1.,0.,0.));
#28800=DIRECTION('center_axis',(0.,0.,-1.));
#28801=DIRECTION('ref_axis',(1.,8.51023079448757E-14,0.));
#28802=DIRECTION('center_axis',(0.,0.,1.));
#28803=DIRECTION('ref_axis',(1.,8.51023079448757E-14,0.));
#28804=DIRECTION('center_axis',(0.,0.,1.));
#28805=DIRECTION('ref_axis',(0.939073080792118,-0.343717542368148,0.));
#28806=DIRECTION('center_axis',(0.,0.,1.));
#28807=DIRECTION('ref_axis',(1.,0.,0.));
#28808=DIRECTION('center_axis',(0.,0.,1.));
#28809=DIRECTION('ref_axis',(1.,0.,0.));
#28810=DIRECTION('',(-0.957826285221151,-1.17299889433528E-16,0.287347885566345));
#28811=DIRECTION('center_axis',(0.,0.,-1.));
#28812=DIRECTION('ref_axis',(1.,0.,0.));
#28813=DIRECTION('center_axis',(-0.706367935150259,-0.707844856018294,0.));
#28814=DIRECTION('ref_axis',(0.707844856018294,-0.706367935150259,0.));
#28815=DIRECTION('',(0.,0.,1.));
#28816=DIRECTION('',(0.707844856018294,-0.706367935150259,0.));
#28817=DIRECTION('',(0.,0.,1.));
#28818=DIRECTION('',(0.707844856018294,-0.706367935150259,0.));
#28819=DIRECTION('center_axis',(0.,0.,1.));
#28820=DIRECTION('ref_axis',(0.965925826289068,-0.258819045102522,0.));
#28821=DIRECTION('center_axis',(0.,0.,1.));
#28822=DIRECTION('ref_axis',(1.,0.,0.));
#28823=DIRECTION('',(-0.966195594825111,-0.257810148249735,0.));
#28824=DIRECTION('center_axis',(-0.257810148249735,0.966195594825111,0.));
#28825=DIRECTION('ref_axis',(-0.966195594825111,-0.257810148249735,0.));
#28826=DIRECTION('',(0.,0.,-1.));
#28827=DIRECTION('',(-0.966195594825111,-0.257810148249735,0.));
#28828=DIRECTION('center_axis',(0.,0.,1.));
#28829=DIRECTION('ref_axis',(0.965925826289068,-0.258819045102522,0.));
#28830=DIRECTION('center_axis',(0.,0.,-1.));
#28831=DIRECTION('ref_axis',(1.,0.,0.));
#28832=DIRECTION('center_axis',(-0.865502761139503,-0.500904152967308,0.));
#28833=DIRECTION('ref_axis',(0.500904152967308,-0.865502761139503,0.));
#28834=DIRECTION('',(0.,0.,1.));
#28835=DIRECTION('',(0.500904152967308,-0.865502761139503,0.));
#28836=DIRECTION('',(0.,0.,1.));
#28837=DIRECTION('',(0.500904152967308,-0.865502761139503,0.));
#28838=DIRECTION('center_axis',(0.,0.,1.));
#28839=DIRECTION('ref_axis',(0.866025403784438,-0.500000000000001,0.));
#28840=DIRECTION('center_axis',(0.,0.,1.));
#28841=DIRECTION('ref_axis',(1.,0.,0.));
#28842=DIRECTION('',(-0.999999454676039,0.00104434076106441,0.));
#28843=DIRECTION('center_axis',(0.00104434076106438,0.999999454676039,0.));
#28844=DIRECTION('ref_axis',(-0.999999454676039,0.00104434076106438,0.));
#28845=DIRECTION('',(0.,0.,-1.));
#28846=DIRECTION('',(-0.999999454676039,0.00104434076106441,0.));
#28847=DIRECTION('center_axis',(0.,0.,1.));
#28848=DIRECTION('ref_axis',(0.866025403784438,-0.500000000000001,0.));
#28849=DIRECTION('center_axis',(0.,0.,-1.));
#28850=DIRECTION('ref_axis',(1.,0.,0.));
#28851=DIRECTION('center_axis',(-0.96565500426803,-0.259827659674851,0.));
#28852=DIRECTION('ref_axis',(0.259827659674851,-0.96565500426803,0.));
#28853=DIRECTION('',(0.,0.,1.));
#28854=DIRECTION('',(0.259827659674851,-0.96565500426803,0.));
#28855=DIRECTION('',(0.,0.,1.));
#28856=DIRECTION('',(0.259827659674851,-0.96565500426803,0.));
#28857=DIRECTION('center_axis',(0.,0.,1.));
#28858=DIRECTION('ref_axis',(0.707106781186547,-0.707106781186548,0.));
#28859=DIRECTION('center_axis',(0.,0.,1.));
#28860=DIRECTION('ref_axis',(1.,0.,0.));
#28861=DIRECTION('',(-0.96565500426803,0.259827659674852,0.));
#28862=DIRECTION('center_axis',(0.259827659674852,0.96565500426803,0.));
#28863=DIRECTION('ref_axis',(-0.96565500426803,0.259827659674852,0.));
#28864=DIRECTION('',(0.,0.,-1.));
#28865=DIRECTION('',(-0.96565500426803,0.259827659674852,0.));
#28866=DIRECTION('center_axis',(0.,0.,1.));
#28867=DIRECTION('ref_axis',(0.707106781186547,-0.707106781186548,0.));
#28868=DIRECTION('center_axis',(0.,0.,-1.));
#28869=DIRECTION('ref_axis',(1.,0.,0.));
#28870=DIRECTION('center_axis',(-0.999999454676039,-0.00104434076106302,
0.));
#28871=DIRECTION('ref_axis',(0.00104434076106302,-0.999999454676039,0.));
#28872=DIRECTION('',(0.,0.,1.));
#28873=DIRECTION('',(0.00104434076106297,-0.999999454676039,0.));
#28874=DIRECTION('',(0.,0.,1.));
#28875=DIRECTION('',(0.00104434076106297,-0.999999454676039,0.));
#28876=DIRECTION('center_axis',(0.,0.,1.));
#28877=DIRECTION('ref_axis',(0.499999999999999,-0.866025403784439,0.));
#28878=DIRECTION('center_axis',(0.,0.,1.));
#28879=DIRECTION('ref_axis',(1.,0.,0.));
#28880=DIRECTION('',(-0.865502761139503,0.500904152967309,0.));
#28881=DIRECTION('center_axis',(0.500904152967309,0.865502761139503,0.));
#28882=DIRECTION('ref_axis',(-0.865502761139503,0.500904152967309,0.));
#28883=DIRECTION('',(0.,0.,-1.));
#28884=DIRECTION('',(-0.865502761139503,0.500904152967309,0.));
#28885=DIRECTION('center_axis',(0.,0.,1.));
#28886=DIRECTION('ref_axis',(0.499999999999999,-0.866025403784439,0.));
#28887=DIRECTION('center_axis',(0.,0.,-1.));
#28888=DIRECTION('ref_axis',(1.,0.,0.));
#28889=DIRECTION('center_axis',(-0.966195594825111,0.257810148249736,0.));
#28890=DIRECTION('ref_axis',(-0.257810148249736,-0.966195594825111,0.));
#28891=DIRECTION('',(0.,0.,1.));
#28892=DIRECTION('',(-0.257810148249736,-0.96619559482511,0.));
#28893=DIRECTION('',(0.,0.,1.));
#28894=DIRECTION('',(-0.257810148249736,-0.96619559482511,0.));
#28895=DIRECTION('center_axis',(0.,0.,1.));
#28896=DIRECTION('ref_axis',(0.25881904510252,-0.965925826289068,0.));
#28897=DIRECTION('center_axis',(0.,0.,1.));
#28898=DIRECTION('ref_axis',(1.,0.,0.));
#28899=DIRECTION('',(-0.706367935150259,0.707844856018295,0.));
#28900=DIRECTION('center_axis',(0.707844856018295,0.706367935150259,0.));
#28901=DIRECTION('ref_axis',(-0.706367935150259,0.707844856018295,0.));
#28902=DIRECTION('',(0.,0.,-1.));
#28903=DIRECTION('',(-0.706367935150259,0.707844856018295,0.));
#28904=DIRECTION('center_axis',(0.,0.,1.));
#28905=DIRECTION('ref_axis',(0.25881904510252,-0.965925826289068,0.));
#28906=DIRECTION('center_axis',(0.,0.,-1.));
#28907=DIRECTION('ref_axis',(1.,0.,0.));
#28908=DIRECTION('center_axis',(-0.866547101900567,0.499095301708731,0.));
#28909=DIRECTION('ref_axis',(-0.499095301708731,-0.866547101900567,0.));
#28910=DIRECTION('',(0.,0.,1.));
#28911=DIRECTION('',(-0.499095301708731,-0.866547101900567,0.));
#28912=DIRECTION('',(0.,0.,1.));
#28913=DIRECTION('',(-0.499095301708731,-0.866547101900567,0.));
#28914=DIRECTION('center_axis',(0.,0.,1.));
#28915=DIRECTION('ref_axis',(-1.94289029309402E-16,-1.,0.));
#28916=DIRECTION('center_axis',(0.,0.,1.));
#28917=DIRECTION('ref_axis',(1.,0.,0.));
#28918=DIRECTION('',(-0.49909530170873,0.866547101900567,0.));
#28919=DIRECTION('center_axis',(0.866547101900567,0.49909530170873,0.));
#28920=DIRECTION('ref_axis',(-0.49909530170873,0.866547101900567,0.));
#28921=DIRECTION('',(0.,0.,-1.));
#28922=DIRECTION('',(-0.49909530170873,0.866547101900567,0.));
#28923=DIRECTION('center_axis',(0.,0.,1.));
#28924=DIRECTION('ref_axis',(-1.94289029309402E-16,-1.,0.));
#28925=DIRECTION('center_axis',(0.,0.,-1.));
#28926=DIRECTION('ref_axis',(1.,0.,0.));
#28927=DIRECTION('center_axis',(-0.707844856018294,0.706367935150259,0.));
#28928=DIRECTION('ref_axis',(-0.706367935150259,-0.707844856018294,0.));
#28929=DIRECTION('',(0.,0.,1.));
#28930=DIRECTION('',(-0.706367935150259,-0.707844856018294,0.));
#28931=DIRECTION('',(0.,0.,1.));
#28932=DIRECTION('',(-0.706367935150259,-0.707844856018294,0.));
#28933=DIRECTION('center_axis',(0.,0.,1.));
#28934=DIRECTION('ref_axis',(-0.258819045102522,-0.965925826289068,0.));
#28935=DIRECTION('center_axis',(0.,0.,1.));
#28936=DIRECTION('ref_axis',(1.,0.,0.));
#28937=DIRECTION('',(-0.257810148249735,0.966195594825111,0.));
#28938=DIRECTION('center_axis',(0.966195594825111,0.257810148249735,0.));
#28939=DIRECTION('ref_axis',(-0.257810148249735,0.966195594825111,0.));
#28940=DIRECTION('',(0.,0.,-1.));
#28941=DIRECTION('',(-0.257810148249735,0.966195594825111,0.));
#28942=DIRECTION('center_axis',(0.,0.,1.));
#28943=DIRECTION('ref_axis',(-0.258819045102522,-0.965925826289068,0.));
#28944=DIRECTION('center_axis',(0.,0.,-1.));
#28945=DIRECTION('ref_axis',(1.,0.,0.));
#28946=DIRECTION('center_axis',(-0.500904152967308,0.865502761139503,0.));
#28947=DIRECTION('ref_axis',(-0.865502761139503,-0.500904152967308,0.));
#28948=DIRECTION('',(0.,0.,1.));
#28949=DIRECTION('',(-0.865502761139503,-0.500904152967308,0.));
#28950=DIRECTION('',(0.,0.,1.));
#28951=DIRECTION('',(-0.865502761139503,-0.500904152967308,0.));
#28952=DIRECTION('center_axis',(0.,0.,1.));
#28953=DIRECTION('ref_axis',(-0.500000000000001,-0.866025403784438,0.));
#28954=DIRECTION('center_axis',(0.,0.,1.));
#28955=DIRECTION('ref_axis',(1.,0.,0.));
#28956=DIRECTION('',(0.00104434076106441,0.999999454676039,0.));
#28957=DIRECTION('center_axis',(0.999999454676039,-0.00104434076106438,
0.));
#28958=DIRECTION('ref_axis',(0.00104434076106438,0.999999454676039,0.));
#28959=DIRECTION('',(0.,0.,-1.));
#28960=DIRECTION('',(0.00104434076106441,0.999999454676039,0.));
#28961=DIRECTION('center_axis',(0.,0.,1.));
#28962=DIRECTION('ref_axis',(-0.500000000000001,-0.866025403784438,0.));
#28963=DIRECTION('center_axis',(0.,0.,-1.));
#28964=DIRECTION('ref_axis',(1.,0.,0.));
#28965=DIRECTION('center_axis',(-0.259827659674851,0.96565500426803,0.));
#28966=DIRECTION('ref_axis',(-0.96565500426803,-0.259827659674851,0.));
#28967=DIRECTION('',(0.,0.,1.));
#28968=DIRECTION('',(-0.96565500426803,-0.259827659674851,0.));
#28969=DIRECTION('',(0.,0.,1.));
#28970=DIRECTION('',(-0.96565500426803,-0.259827659674851,0.));
#28971=DIRECTION('center_axis',(0.,0.,1.));
#28972=DIRECTION('ref_axis',(-0.707106781186548,-0.707106781186547,0.));
#28973=DIRECTION('center_axis',(0.,0.,1.));
#28974=DIRECTION('ref_axis',(1.,0.,0.));
#28975=DIRECTION('',(0.259827659674852,0.96565500426803,0.));
#28976=DIRECTION('center_axis',(0.96565500426803,-0.259827659674852,0.));
#28977=DIRECTION('ref_axis',(0.259827659674852,0.96565500426803,0.));
#28978=DIRECTION('',(0.,0.,-1.));
#28979=DIRECTION('',(0.259827659674852,0.96565500426803,0.));
#28980=DIRECTION('center_axis',(0.,0.,1.));
#28981=DIRECTION('ref_axis',(-0.707106781186548,-0.707106781186547,0.));
#28982=DIRECTION('center_axis',(0.,0.,-1.));
#28983=DIRECTION('ref_axis',(1.,0.,0.));
#28984=DIRECTION('center_axis',(-0.00104434076106344,0.999999454676039,
0.));
#28985=DIRECTION('ref_axis',(-0.999999454676039,-0.00104434076106344,0.));
#28986=DIRECTION('',(0.,0.,1.));
#28987=DIRECTION('',(-0.999999454676039,-0.00104434076106344,0.));
#28988=DIRECTION('',(0.,0.,1.));
#28989=DIRECTION('',(-0.999999454676039,-0.00104434076106344,0.));
#28990=DIRECTION('center_axis',(0.,0.,1.));
#28991=DIRECTION('ref_axis',(-0.866025403784439,-0.5,0.));
#28992=DIRECTION('center_axis',(0.,0.,1.));
#28993=DIRECTION('ref_axis',(1.,0.,0.));
#28994=DIRECTION('',(0.500904152967309,0.865502761139503,0.));
#28995=DIRECTION('center_axis',(0.865502761139503,-0.500904152967309,0.));
#28996=DIRECTION('ref_axis',(0.500904152967309,0.865502761139503,0.));
#28997=DIRECTION('',(0.,0.,-1.));
#28998=DIRECTION('',(0.500904152967309,0.865502761139503,0.));
#28999=DIRECTION('center_axis',(0.,0.,1.));
#29000=DIRECTION('ref_axis',(-0.866025403784439,-0.5,0.));
#29001=DIRECTION('center_axis',(0.,0.,-1.));
#29002=DIRECTION('ref_axis',(1.,0.,0.));
#29003=DIRECTION('center_axis',(0.257810148249736,0.966195594825111,0.));
#29004=DIRECTION('ref_axis',(-0.966195594825111,0.257810148249736,0.));
#29005=DIRECTION('',(0.,0.,1.));
#29006=DIRECTION('',(-0.96619559482511,0.257810148249736,0.));
#29007=DIRECTION('',(0.,0.,1.));
#29008=DIRECTION('',(-0.96619559482511,0.257810148249736,0.));
#29009=DIRECTION('center_axis',(0.,0.,1.));
#29010=DIRECTION('ref_axis',(-0.965925826289068,-0.25881904510252,0.));
#29011=DIRECTION('center_axis',(0.,0.,1.));
#29012=DIRECTION('ref_axis',(1.,0.,0.));
#29013=DIRECTION('',(0.707844856018295,0.706367935150259,0.));
#29014=DIRECTION('center_axis',(0.706367935150259,-0.707844856018295,0.));
#29015=DIRECTION('ref_axis',(0.707844856018295,0.706367935150259,0.));
#29016=DIRECTION('',(0.,0.,-1.));
#29017=DIRECTION('',(0.707844856018295,0.706367935150259,0.));
#29018=DIRECTION('center_axis',(0.,0.,1.));
#29019=DIRECTION('ref_axis',(-0.965925826289068,-0.25881904510252,0.));
#29020=DIRECTION('center_axis',(0.,0.,-1.));
#29021=DIRECTION('ref_axis',(1.,0.,0.));
#29022=DIRECTION('center_axis',(0.499095301708731,0.866547101900567,0.));
#29023=DIRECTION('ref_axis',(-0.866547101900567,0.499095301708731,0.));
#29024=DIRECTION('',(0.,0.,1.));
#29025=DIRECTION('',(-0.866547101900567,0.499095301708731,0.));
#29026=DIRECTION('',(0.,0.,1.));
#29027=DIRECTION('',(-0.866547101900567,0.499095301708731,0.));
#29028=DIRECTION('center_axis',(0.,0.,1.));
#29029=DIRECTION('ref_axis',(-1.,1.38777878078145E-16,0.));
#29030=DIRECTION('center_axis',(0.,0.,1.));
#29031=DIRECTION('ref_axis',(1.,0.,0.));
#29032=DIRECTION('',(0.866547101900567,0.499095301708731,0.));
#29033=DIRECTION('center_axis',(0.,0.,1.));
#29034=DIRECTION('ref_axis',(1.,0.,0.));
#29035=DIRECTION('center_axis',(0.499095301708731,-0.866547101900567,0.));
#29036=DIRECTION('ref_axis',(0.866547101900567,0.499095301708731,0.));
#29037=DIRECTION('',(0.,0.,-1.));
#29038=DIRECTION('',(0.866547101900567,0.499095301708731,0.));
#29039=DIRECTION('center_axis',(0.,0.,1.));
#29040=DIRECTION('ref_axis',(-1.,1.38777878078145E-16,0.));
#29041=DIRECTION('center_axis',(0.,0.,-1.));
#29042=DIRECTION('ref_axis',(1.,0.,0.));
#29043=DIRECTION('center_axis',(0.,0.,-1.));
#29044=DIRECTION('ref_axis',(1.,0.,0.));
#29045=DIRECTION('center_axis',(0.706367935150259,0.707844856018294,0.));
#29046=DIRECTION('ref_axis',(-0.707844856018294,0.706367935150259,0.));
#29047=DIRECTION('',(0.,0.,1.));
#29048=DIRECTION('',(-0.707844856018294,0.706367935150259,0.));
#29049=DIRECTION('',(0.,0.,1.));
#29050=DIRECTION('',(-0.707844856018294,0.706367935150259,0.));
#29051=DIRECTION('center_axis',(0.,0.,1.));
#29052=DIRECTION('ref_axis',(-0.965925826289068,0.258819045102521,0.));
#29053=DIRECTION('center_axis',(0.,0.,1.));
#29054=DIRECTION('ref_axis',(1.,0.,0.));
#29055=DIRECTION('',(0.966195594825111,0.257810148249736,0.));
#29056=DIRECTION('center_axis',(0.257810148249736,-0.966195594825111,0.));
#29057=DIRECTION('ref_axis',(0.966195594825111,0.257810148249736,0.));
#29058=DIRECTION('',(0.,0.,-1.));
#29059=DIRECTION('',(0.966195594825111,0.257810148249736,0.));
#29060=DIRECTION('center_axis',(0.,0.,1.));
#29061=DIRECTION('ref_axis',(-0.965925826289068,0.258819045102521,0.));
#29062=DIRECTION('center_axis',(0.,0.,-1.));
#29063=DIRECTION('ref_axis',(1.,0.,0.));
#29064=DIRECTION('center_axis',(0.865502761139503,0.500904152967308,0.));
#29065=DIRECTION('ref_axis',(-0.500904152967308,0.865502761139503,0.));
#29066=DIRECTION('',(0.,0.,1.));
#29067=DIRECTION('',(-0.500904152967308,0.865502761139503,0.));
#29068=DIRECTION('',(0.,0.,1.));
#29069=DIRECTION('',(-0.500904152967308,0.865502761139503,0.));
#29070=DIRECTION('center_axis',(0.,0.,1.));
#29071=DIRECTION('ref_axis',(-0.866025403784438,0.5,0.));
#29072=DIRECTION('center_axis',(0.,0.,1.));
#29073=DIRECTION('ref_axis',(1.,0.,0.));
#29074=DIRECTION('',(0.999999454676039,-0.00104434076106422,0.));
#29075=DIRECTION('center_axis',(-0.00104434076106422,-0.999999454676039,
0.));
#29076=DIRECTION('ref_axis',(0.999999454676039,-0.00104434076106422,0.));
#29077=DIRECTION('',(0.,0.,-1.));
#29078=DIRECTION('',(0.999999454676039,-0.00104434076106422,0.));
#29079=DIRECTION('center_axis',(0.,0.,1.));
#29080=DIRECTION('ref_axis',(-0.866025403784438,0.5,0.));
#29081=DIRECTION('center_axis',(0.,0.,-1.));
#29082=DIRECTION('ref_axis',(1.,0.,0.));
#29083=DIRECTION('center_axis',(0.96565500426803,0.259827659674852,0.));
#29084=DIRECTION('ref_axis',(-0.259827659674852,0.96565500426803,0.));
#29085=DIRECTION('',(0.,0.,1.));
#29086=DIRECTION('',(-0.259827659674852,0.96565500426803,0.));
#29087=DIRECTION('',(0.,0.,1.));
#29088=DIRECTION('',(-0.259827659674852,0.96565500426803,0.));
#29089=DIRECTION('center_axis',(0.,0.,1.));
#29090=DIRECTION('ref_axis',(-0.707106781186548,0.707106781186548,0.));
#29091=DIRECTION('center_axis',(0.,0.,1.));
#29092=DIRECTION('ref_axis',(1.,0.,0.));
#29093=DIRECTION('',(0.96565500426803,-0.259827659674852,0.));
#29094=DIRECTION('center_axis',(-0.259827659674852,-0.96565500426803,0.));
#29095=DIRECTION('ref_axis',(0.96565500426803,-0.259827659674852,0.));
#29096=DIRECTION('',(0.,0.,-1.));
#29097=DIRECTION('',(0.96565500426803,-0.259827659674852,0.));
#29098=DIRECTION('center_axis',(0.,0.,1.));
#29099=DIRECTION('ref_axis',(-0.707106781186548,0.707106781186548,0.));
#29100=DIRECTION('center_axis',(0.,0.,-1.));
#29101=DIRECTION('ref_axis',(1.,0.,0.));
#29102=DIRECTION('center_axis',(0.999999454676039,0.00104434076106355,0.));
#29103=DIRECTION('ref_axis',(-0.00104434076106355,0.999999454676039,0.));
#29104=DIRECTION('',(0.,0.,1.));
#29105=DIRECTION('',(-0.00104434076106355,0.999999454676039,0.));
#29106=DIRECTION('',(0.,0.,1.));
#29107=DIRECTION('',(-0.00104434076106355,0.999999454676039,0.));
#29108=DIRECTION('center_axis',(0.,0.,1.));
#29109=DIRECTION('ref_axis',(-0.5,0.866025403784439,0.));
#29110=DIRECTION('center_axis',(0.,0.,1.));
#29111=DIRECTION('ref_axis',(1.,0.,0.));
#29112=DIRECTION('',(0.865502761139503,-0.500904152967308,0.));
#29113=DIRECTION('center_axis',(-0.500904152967309,-0.865502761139503,0.));
#29114=DIRECTION('ref_axis',(0.865502761139503,-0.500904152967309,0.));
#29115=DIRECTION('',(0.,0.,-1.));
#29116=DIRECTION('',(0.865502761139503,-0.500904152967308,0.));
#29117=DIRECTION('center_axis',(0.,0.,1.));
#29118=DIRECTION('ref_axis',(-0.5,0.866025403784439,0.));
#29119=DIRECTION('center_axis',(0.,0.,-1.));
#29120=DIRECTION('ref_axis',(1.,0.,0.));
#29121=DIRECTION('center_axis',(0.966195594825111,-0.257810148249736,0.));
#29122=DIRECTION('ref_axis',(0.257810148249736,0.966195594825111,0.));
#29123=DIRECTION('',(0.,0.,1.));
#29124=DIRECTION('',(0.257810148249736,0.966195594825111,0.));
#29125=DIRECTION('',(0.,0.,1.));
#29126=DIRECTION('',(0.257810148249736,0.966195594825111,0.));
#29127=DIRECTION('center_axis',(0.,0.,1.));
#29128=DIRECTION('ref_axis',(-0.258819045102521,0.965925826289068,0.));
#29129=DIRECTION('center_axis',(0.,0.,1.));
#29130=DIRECTION('ref_axis',(1.,0.,0.));
#29131=DIRECTION('',(0.706367935150259,-0.707844856018294,0.));
#29132=DIRECTION('center_axis',(-0.707844856018294,-0.706367935150259,0.));
#29133=DIRECTION('ref_axis',(0.706367935150259,-0.707844856018294,0.));
#29134=DIRECTION('',(0.,0.,-1.));
#29135=DIRECTION('',(0.706367935150259,-0.707844856018294,0.));
#29136=DIRECTION('center_axis',(0.,0.,1.));
#29137=DIRECTION('ref_axis',(-0.258819045102521,0.965925826289068,0.));
#29138=DIRECTION('center_axis',(0.,0.,-1.));
#29139=DIRECTION('ref_axis',(1.,0.,0.));
#29140=DIRECTION('center_axis',(0.866547101900567,-0.499095301708731,0.));
#29141=DIRECTION('ref_axis',(0.499095301708731,0.866547101900567,0.));
#29142=DIRECTION('',(0.,0.,1.));
#29143=DIRECTION('',(0.499095301708731,0.866547101900567,0.));
#29144=DIRECTION('',(0.,0.,1.));
#29145=DIRECTION('',(0.499095301708731,0.866547101900567,0.));
#29146=DIRECTION('center_axis',(0.,0.,1.));
#29147=DIRECTION('ref_axis',(8.32667268468867E-17,1.,0.));
#29148=DIRECTION('center_axis',(0.,0.,1.));
#29149=DIRECTION('ref_axis',(1.,0.,0.));
#29150=DIRECTION('',(0.499095301708731,-0.866547101900567,0.));
#29151=DIRECTION('center_axis',(-0.866547101900567,-0.499095301708731,0.));
#29152=DIRECTION('ref_axis',(0.499095301708731,-0.866547101900567,0.));
#29153=DIRECTION('',(0.,0.,-1.));
#29154=DIRECTION('',(0.499095301708731,-0.866547101900567,0.));
#29155=DIRECTION('center_axis',(0.,0.,1.));
#29156=DIRECTION('ref_axis',(8.32667268468867E-17,1.,0.));
#29157=DIRECTION('center_axis',(0.,0.,-1.));
#29158=DIRECTION('ref_axis',(1.,0.,0.));
#29159=DIRECTION('center_axis',(0.707844856018294,-0.706367935150259,0.));
#29160=DIRECTION('ref_axis',(0.706367935150259,0.707844856018294,0.));
#29161=DIRECTION('',(0.,0.,1.));
#29162=DIRECTION('',(0.706367935150259,0.707844856018294,0.));
#29163=DIRECTION('',(0.,0.,1.));
#29164=DIRECTION('',(0.706367935150259,0.707844856018294,0.));
#29165=DIRECTION('center_axis',(0.,0.,1.));
#29166=DIRECTION('ref_axis',(0.258819045102521,0.965925826289068,0.));
#29167=DIRECTION('center_axis',(0.,0.,1.));
#29168=DIRECTION('ref_axis',(1.,0.,0.));
#29169=DIRECTION('',(0.257810148249736,-0.966195594825111,0.));
#29170=DIRECTION('center_axis',(-0.966195594825111,-0.257810148249736,0.));
#29171=DIRECTION('ref_axis',(0.257810148249736,-0.966195594825111,0.));
#29172=DIRECTION('',(0.,0.,-1.));
#29173=DIRECTION('',(0.257810148249736,-0.966195594825111,0.));
#29174=DIRECTION('center_axis',(0.,0.,1.));
#29175=DIRECTION('ref_axis',(0.258819045102521,0.965925826289068,0.));
#29176=DIRECTION('center_axis',(0.,0.,-1.));
#29177=DIRECTION('ref_axis',(1.,0.,0.));
#29178=DIRECTION('center_axis',(0.500904152967308,-0.865502761139503,0.));
#29179=DIRECTION('ref_axis',(0.865502761139503,0.500904152967308,0.));
#29180=DIRECTION('',(0.,0.,1.));
#29181=DIRECTION('',(0.865502761139503,0.500904152967308,0.));
#29182=DIRECTION('',(0.,0.,1.));
#29183=DIRECTION('',(0.865502761139503,0.500904152967308,0.));
#29184=DIRECTION('center_axis',(0.,0.,1.));
#29185=DIRECTION('ref_axis',(0.5,0.866025403784439,0.));
#29186=DIRECTION('center_axis',(0.,0.,1.));
#29187=DIRECTION('ref_axis',(1.,0.,0.));
#29188=DIRECTION('',(-0.00104434076106397,-0.999999454676039,0.));
#29189=DIRECTION('center_axis',(-0.999999454676039,0.00104434076106394,
0.));
#29190=DIRECTION('ref_axis',(-0.00104434076106394,-0.999999454676039,0.));
#29191=DIRECTION('',(0.,0.,-1.));
#29192=DIRECTION('',(-0.00104434076106397,-0.999999454676039,0.));
#29193=DIRECTION('center_axis',(0.,0.,1.));
#29194=DIRECTION('ref_axis',(0.5,0.866025403784439,0.));
#29195=DIRECTION('center_axis',(0.,0.,-1.));
#29196=DIRECTION('ref_axis',(1.,0.,0.));
#29197=DIRECTION('center_axis',(0.259827659674852,-0.96565500426803,0.));
#29198=DIRECTION('ref_axis',(0.96565500426803,0.259827659674852,0.));
#29199=DIRECTION('',(0.,0.,1.));
#29200=DIRECTION('',(0.96565500426803,0.259827659674852,0.));
#29201=DIRECTION('',(0.,0.,1.));
#29202=DIRECTION('',(0.96565500426803,0.259827659674852,0.));
#29203=DIRECTION('center_axis',(0.,0.,1.));
#29204=DIRECTION('ref_axis',(0.707106781186547,0.707106781186548,0.));
#29205=DIRECTION('center_axis',(0.,0.,1.));
#29206=DIRECTION('ref_axis',(1.,0.,0.));
#29207=DIRECTION('',(-0.259827659674852,-0.96565500426803,0.));
#29208=DIRECTION('center_axis',(-0.96565500426803,0.259827659674852,0.));
#29209=DIRECTION('ref_axis',(-0.259827659674852,-0.96565500426803,0.));
#29210=DIRECTION('',(0.,0.,-1.));
#29211=DIRECTION('',(-0.259827659674852,-0.96565500426803,0.));
#29212=DIRECTION('center_axis',(0.,0.,1.));
#29213=DIRECTION('ref_axis',(0.707106781186547,0.707106781186548,0.));
#29214=DIRECTION('center_axis',(0.,0.,-1.));
#29215=DIRECTION('ref_axis',(1.,0.,0.));
#29216=DIRECTION('center_axis',(0.00104434076106372,-0.999999454676039,
0.));
#29217=DIRECTION('ref_axis',(0.999999454676039,0.00104434076106372,0.));
#29218=DIRECTION('',(0.,0.,1.));
#29219=DIRECTION('',(0.999999454676039,0.00104434076106372,0.));
#29220=DIRECTION('',(0.,0.,1.));
#29221=DIRECTION('',(0.999999454676039,0.00104434076106372,0.));
#29222=DIRECTION('center_axis',(0.,0.,1.));
#29223=DIRECTION('ref_axis',(0.866025403784439,0.5,0.));
#29224=DIRECTION('center_axis',(0.,0.,1.));
#29225=DIRECTION('ref_axis',(1.,0.,0.));
#29226=DIRECTION('',(-0.500904152967308,-0.865502761139503,0.));
#29227=DIRECTION('center_axis',(-0.865502761139503,0.500904152967308,0.));
#29228=DIRECTION('ref_axis',(-0.500904152967308,-0.865502761139503,0.));
#29229=DIRECTION('',(0.,0.,-1.));
#29230=DIRECTION('',(-0.500904152967308,-0.865502761139503,0.));
#29231=DIRECTION('center_axis',(0.,0.,1.));
#29232=DIRECTION('ref_axis',(0.866025403784439,0.5,0.));
#29233=DIRECTION('center_axis',(0.,0.,-1.));
#29234=DIRECTION('ref_axis',(1.,0.,0.));
#29235=DIRECTION('center_axis',(-0.257810148249736,-0.966195594825111,0.));
#29236=DIRECTION('ref_axis',(0.966195594825111,-0.257810148249736,0.));
#29237=DIRECTION('',(0.,0.,1.));
#29238=DIRECTION('',(0.966195594825111,-0.257810148249736,0.));
#29239=DIRECTION('',(0.,0.,1.));
#29240=DIRECTION('',(0.966195594825111,-0.257810148249736,0.));
#29241=DIRECTION('center_axis',(0.,0.,1.));
#29242=DIRECTION('ref_axis',(0.965925826289068,0.258819045102521,0.));
#29243=DIRECTION('center_axis',(0.,0.,1.));
#29244=DIRECTION('ref_axis',(1.,0.,0.));
#29245=DIRECTION('',(-0.707844856018294,-0.706367935150259,0.));
#29246=DIRECTION('center_axis',(-0.706367935150259,0.707844856018294,0.));
#29247=DIRECTION('ref_axis',(-0.707844856018294,-0.706367935150259,0.));
#29248=DIRECTION('',(0.,0.,-1.));
#29249=DIRECTION('',(-0.707844856018294,-0.706367935150259,0.));
#29250=DIRECTION('center_axis',(0.,0.,1.));
#29251=DIRECTION('ref_axis',(0.965925826289068,0.258819045102521,0.));
#29252=DIRECTION('center_axis',(0.,0.,-1.));
#29253=DIRECTION('ref_axis',(1.,0.,0.));
#29254=DIRECTION('center_axis',(-0.499095301708731,-0.866547101900567,0.));
#29255=DIRECTION('ref_axis',(0.866547101900567,-0.499095301708731,0.));
#29256=DIRECTION('',(0.,0.,1.));
#29257=DIRECTION('',(0.866547101900567,-0.499095301708731,0.));
#29258=DIRECTION('',(0.,0.,1.));
#29259=DIRECTION('',(0.866547101900567,-0.499095301708731,0.));
#29260=DIRECTION('center_axis',(0.,0.,1.));
#29261=DIRECTION('ref_axis',(1.,0.,0.));
#29262=DIRECTION('center_axis',(0.,0.,1.));
#29263=DIRECTION('ref_axis',(1.,0.,0.));
#29264=DIRECTION('',(-0.866547101900567,-0.499095301708731,0.));
#29265=DIRECTION('center_axis',(-0.499095301708731,0.866547101900567,0.));
#29266=DIRECTION('ref_axis',(-0.866547101900567,-0.499095301708731,0.));
#29267=DIRECTION('',(0.,0.,-1.));
#29268=DIRECTION('',(-0.866547101900567,-0.499095301708731,0.));
#29269=DIRECTION('center_axis',(0.,0.,1.));
#29270=DIRECTION('ref_axis',(1.,0.,0.));
#29271=DIRECTION('center_axis',(0.,0.,-1.));
#29272=DIRECTION('ref_axis',(1.,0.,0.));
#29273=DIRECTION('center_axis',(0.,0.,-1.));
#29274=DIRECTION('ref_axis',(-1.,0.,0.));
#29275=DIRECTION('center_axis',(0.,0.,1.));
#29276=DIRECTION('ref_axis',(1.,0.,0.));
#29277=DIRECTION('center_axis',(0.,0.,1.));
#29278=DIRECTION('ref_axis',(1.,0.,0.));
#29279=DIRECTION('',(0.707106781186547,8.65956056235493E-17,-0.707106781186548));
#29280=DIRECTION('center_axis',(0.,0.,-1.));
#29281=DIRECTION('ref_axis',(-1.,0.,0.));
#29282=DIRECTION('center_axis',(0.,0.,1.));
#29283=DIRECTION('ref_axis',(1.,0.,0.));
#29284=DIRECTION('center_axis',(0.,0.,1.));
#29285=DIRECTION('ref_axis',(1.,0.,0.));
#29286=DIRECTION('center_axis',(0.,0.,1.));
#29287=DIRECTION('ref_axis',(1.,0.,0.));
#29288=DIRECTION('',(0.707106781186547,8.65956056235493E-17,-0.707106781186548));
#29289=DIRECTION('center_axis',(0.,0.,1.));
#29290=DIRECTION('ref_axis',(1.,0.,0.));
#29291=DIRECTION('center_axis',(0.,0.,1.));
#29292=DIRECTION('ref_axis',(1.,0.,0.));
#29293=DIRECTION('',(0.,0.,-1.));
#29294=DIRECTION('',(0.,0.,-1.));
#29295=DIRECTION('center_axis',(0.,0.,-1.));
#29296=DIRECTION('ref_axis',(1.,0.,0.));
#29297=DIRECTION('center_axis',(0.,0.,1.));
#29298=DIRECTION('ref_axis',(1.,0.,0.));
#29299=DIRECTION('',(-0.707106781186548,-8.65956056235493E-17,-0.707106781186547));
#29300=DIRECTION('center_axis',(0.,0.,1.));
#29301=DIRECTION('ref_axis',(1.,0.,0.));
#29302=DIRECTION('axis',(0.,0.,1.));
#29303=DIRECTION('refdir',(1.,0.,0.));
#29304=DIRECTION('center_axis',(0.,0.,1.));
#29305=DIRECTION('ref_axis',(1.,0.,0.));
#29306=DIRECTION('',(0.,0.,-1.));
#29307=DIRECTION('center_axis',(0.,0.,-1.));
#29308=DIRECTION('ref_axis',(1.,0.,0.));
#29309=DIRECTION('',(0.,0.,-1.));
#29310=DIRECTION('center_axis',(0.,0.,1.));
#29311=DIRECTION('ref_axis',(1.,0.,0.));
#29312=DIRECTION('center_axis',(0.,0.,-1.));
#29313=DIRECTION('ref_axis',(1.,0.,0.));
#29314=DIRECTION('center_axis',(0.,0.,1.));
#29315=DIRECTION('ref_axis',(1.,0.,0.));
#29316=DIRECTION('',(0.,0.,-1.));
#29317=DIRECTION('center_axis',(0.,0.,1.));
#29318=DIRECTION('ref_axis',(1.,0.,0.));
#29319=DIRECTION('',(0.,0.,-1.));
#29320=DIRECTION('center_axis',(0.,0.,1.));
#29321=DIRECTION('ref_axis',(1.,0.,0.));
#29322=DIRECTION('',(0.,0.,-1.));
#29323=DIRECTION('center_axis',(0.,0.,1.));
#29324=DIRECTION('ref_axis',(1.,0.,0.));
#29325=DIRECTION('',(0.,0.,-1.));
#29326=DIRECTION('center_axis',(0.,0.,1.));
#29327=DIRECTION('ref_axis',(1.,0.,0.));
#29328=DIRECTION('',(0.,0.,-1.));
#29329=DIRECTION('center_axis',(0.,0.,1.));
#29330=DIRECTION('ref_axis',(1.,0.,0.));
#29331=DIRECTION('',(0.,0.,-1.));
#29332=DIRECTION('center_axis',(0.,0.,1.));
#29333=DIRECTION('ref_axis',(1.,0.,0.));
#29334=DIRECTION('',(0.,0.,-1.));
#29335=DIRECTION('center_axis',(0.,0.,1.));
#29336=DIRECTION('ref_axis',(1.,0.,0.));
#29337=DIRECTION('',(0.,0.,-1.));
#29338=DIRECTION('center_axis',(0.,0.,1.));
#29339=DIRECTION('ref_axis',(1.,0.,0.));
#29340=DIRECTION('',(0.,0.,-1.));
#29341=DIRECTION('center_axis',(0.,0.,1.));
#29342=DIRECTION('ref_axis',(1.,0.,0.));
#29343=DIRECTION('',(0.,0.,-1.));
#29344=DIRECTION('center_axis',(0.,0.,1.));
#29345=DIRECTION('ref_axis',(1.,0.,0.));
#29346=DIRECTION('',(0.,0.,-1.));
#29347=DIRECTION('center_axis',(0.,0.,1.));
#29348=DIRECTION('ref_axis',(1.,0.,0.));
#29349=DIRECTION('',(0.,0.,-1.));
#29350=DIRECTION('center_axis',(0.,0.,1.));
#29351=DIRECTION('ref_axis',(1.,0.,0.));
#29352=DIRECTION('',(0.,0.,-1.));
#29353=DIRECTION('center_axis',(0.,0.,1.));
#29354=DIRECTION('ref_axis',(-0.222205845997876,-0.97499977538683,0.));
#29355=DIRECTION('',(0.,0.,1.));
#29356=DIRECTION('center_axis',(0.,0.,1.));
#29357=DIRECTION('ref_axis',(1.,9.74274476199959E-14,0.));
#29358=DIRECTION('center_axis',(0.,0.,1.));
#29359=DIRECTION('ref_axis',(1.,9.74274476199959E-14,0.));
#29360=DIRECTION('',(0.,0.,1.));
#29361=DIRECTION('center_axis',(0.,0.,1.));
#29362=DIRECTION('ref_axis',(1.,9.74274476199959E-14,0.));
#29363=DIRECTION('',(0.,0.,1.));
#29364=DIRECTION('center_axis',(0.,0.,1.));
#29365=DIRECTION('ref_axis',(1.,9.74274476199959E-14,0.));
#29366=DIRECTION('',(0.,0.,1.));
#29367=DIRECTION('center_axis',(0.,0.,1.));
#29368=DIRECTION('ref_axis',(1.,9.74274476199959E-14,0.));
#29369=DIRECTION('',(0.,0.,1.));
#29370=DIRECTION('center_axis',(0.,0.,1.));
#29371=DIRECTION('ref_axis',(1.,9.74274476199959E-14,0.));
#29372=DIRECTION('',(0.,0.,1.));
#29373=DIRECTION('center_axis',(0.,0.,1.));
#29374=DIRECTION('ref_axis',(1.,9.74274476199959E-14,0.));
#29375=DIRECTION('',(0.,0.,1.));
#29376=DIRECTION('center_axis',(0.,0.,1.));
#29377=DIRECTION('ref_axis',(1.,9.74274476199959E-14,0.));
#29378=DIRECTION('',(0.,0.,1.));
#29379=DIRECTION('center_axis',(0.,0.,1.));
#29380=DIRECTION('ref_axis',(1.,9.74274476199959E-14,0.));
#29381=DIRECTION('',(0.,0.,1.));
#29382=DIRECTION('center_axis',(0.,0.,1.));
#29383=DIRECTION('ref_axis',(1.,9.74274476199959E-14,0.));
#29384=DIRECTION('',(0.,0.,1.));
#29385=DIRECTION('center_axis',(0.,0.,1.));
#29386=DIRECTION('ref_axis',(1.,9.74274476199959E-14,0.));
#29387=DIRECTION('',(0.,0.,1.));
#29388=DIRECTION('center_axis',(0.,0.,1.));
#29389=DIRECTION('ref_axis',(1.,9.74274476199959E-14,0.));
#29390=DIRECTION('',(0.,0.,1.));
#29391=DIRECTION('center_axis',(0.,0.,1.));
#29392=DIRECTION('ref_axis',(1.,9.74274476199959E-14,0.));
#29393=DIRECTION('',(0.,0.,1.));
#29394=DIRECTION('center_axis',(0.,0.,1.));
#29395=DIRECTION('ref_axis',(1.,9.74274476199959E-14,0.));
#29396=DIRECTION('',(0.,0.,1.));
#29397=DIRECTION('center_axis',(0.,0.,1.));
#29398=DIRECTION('ref_axis',(1.,9.74274476199959E-14,0.));
#29399=DIRECTION('',(0.,0.,1.));
#29400=DIRECTION('center_axis',(0.,0.,1.));
#29401=DIRECTION('ref_axis',(1.,0.,0.));
#29402=DIRECTION('center_axis',(0.,0.,1.));
#29403=DIRECTION('ref_axis',(1.,0.,0.));
#29404=DIRECTION('center_axis',(0.,0.,1.));
#29405=DIRECTION('ref_axis',(1.,0.,0.));
#29406=DIRECTION('center_axis',(0.,0.,1.));
#29407=DIRECTION('ref_axis',(1.,0.,0.));
#29408=DIRECTION('center_axis',(0.,0.,-1.));
#29409=DIRECTION('ref_axis',(1.,9.74274476199959E-14,0.));
#29410=DIRECTION('center_axis',(0.,0.,1.));
#29411=DIRECTION('ref_axis',(-0.710030672795894,0.704170748958667,0.));
#29412=DIRECTION('center_axis',(0.,0.,1.));
#29413=DIRECTION('ref_axis',(0.984807753012208,-0.17364817766693,0.));
#29414=DIRECTION('center_axis',(0.,0.,-1.));
#29415=DIRECTION('ref_axis',(1.,0.,0.));
#29416=DIRECTION('',(-0.996089805327885,-0.0883464754353932,0.));
#29417=DIRECTION('',(0.905801965515954,-0.423701309022563,0.));
#29418=DIRECTION('center_axis',(-0.423701309022563,-0.905801965515954,0.));
#29419=DIRECTION('ref_axis',(0.905801965515954,-0.423701309022563,0.));
#29420=DIRECTION('',(0.,0.,1.));
#29421=DIRECTION('',(0.,0.,1.));
#29422=DIRECTION('center_axis',(-0.0883464754353932,0.996089805327885,0.));
#29423=DIRECTION('ref_axis',(-0.996089805327885,-0.0883464754353932,0.));
#29424=DIRECTION('',(0.,0.,-1.));
#29425=DIRECTION('center_axis',(0.,0.,1.));
#29426=DIRECTION('ref_axis',(0.939692620785908,-0.342020143325669,0.));
#29427=DIRECTION('center_axis',(0.,0.,-1.));
#29428=DIRECTION('ref_axis',(1.,0.,0.));
#29429=DIRECTION('',(-0.996298167445974,0.0859648855277176,0.));
#29430=DIRECTION('',(0.818465838146947,-0.574555194725812,0.));
#29431=DIRECTION('center_axis',(-0.574555194725812,-0.818465838146947,0.));
#29432=DIRECTION('ref_axis',(0.818465838146947,-0.574555194725812,0.));
#29433=DIRECTION('',(0.,0.,1.));
#29434=DIRECTION('',(0.,0.,1.));
#29435=DIRECTION('center_axis',(0.0859648855277176,0.996298167445974,0.));
#29436=DIRECTION('ref_axis',(-0.996298167445974,0.0859648855277176,0.));
#29437=DIRECTION('',(0.,0.,-1.));
#29438=DIRECTION('center_axis',(0.,0.,1.));
#29439=DIRECTION('ref_axis',(0.866025403784438,-0.5,0.));
#29440=DIRECTION('center_axis',(0.,0.,-1.));
#29441=DIRECTION('ref_axis',(1.,0.,0.));
#29442=DIRECTION('',(-0.966234513897416,0.257664246944399,0.));
#29443=DIRECTION('',(0.706261040449543,-0.707951511576272,0.));
#29444=DIRECTION('center_axis',(-0.707951511576272,-0.706261040449543,0.));
#29445=DIRECTION('ref_axis',(0.706261040449543,-0.707951511576272,0.));
#29446=DIRECTION('',(0.,0.,1.));
#29447=DIRECTION('',(0.,0.,1.));
#29448=DIRECTION('center_axis',(0.257664246944399,0.966234513897416,0.));
#29449=DIRECTION('ref_axis',(-0.966234513897416,0.257664246944399,0.));
#29450=DIRECTION('',(0.,0.,-1.));
#29451=DIRECTION('center_axis',(0.,0.,1.));
#29452=DIRECTION('ref_axis',(0.766044443118978,-0.64278760968654,0.));
#29453=DIRECTION('center_axis',(0.,0.,-1.));
#29454=DIRECTION('ref_axis',(1.,0.,0.));
#29455=DIRECTION('',(-0.906812313582341,0.421534610602074,0.));
#29456=DIRECTION('',(0.572596858423411,-0.819837079988238,0.));
#29457=DIRECTION('center_axis',(-0.819837079988238,-0.572596858423411,0.));
#29458=DIRECTION('ref_axis',(0.572596858423411,-0.819837079988238,0.));
#29459=DIRECTION('',(0.,0.,1.));
#29460=DIRECTION('',(0.,0.,1.));
#29461=DIRECTION('center_axis',(0.421534610602074,0.906812313582341,0.));
#29462=DIRECTION('ref_axis',(-0.906812313582341,0.421534610602074,0.));
#29463=DIRECTION('',(0.,0.,-1.));
#29464=DIRECTION('center_axis',(0.,0.,1.));
#29465=DIRECTION('ref_axis',(0.642787609686539,-0.766044443118978,0.));
#29466=DIRECTION('center_axis',(0.,0.,-1.));
#29467=DIRECTION('ref_axis',(1.,0.,0.));
#29468=DIRECTION('',(-0.819837079988238,0.572596858423411,0.));
#29469=DIRECTION('',(0.421534610602074,-0.906812313582341,0.));
#29470=DIRECTION('center_axis',(-0.906812313582341,-0.421534610602074,0.));
#29471=DIRECTION('ref_axis',(0.421534610602074,-0.906812313582341,0.));
#29472=DIRECTION('',(0.,0.,1.));
#29473=DIRECTION('',(0.,0.,1.));
#29474=DIRECTION('center_axis',(0.572596858423411,0.819837079988238,0.));
#29475=DIRECTION('ref_axis',(-0.819837079988238,0.572596858423411,0.));
#29476=DIRECTION('',(0.,0.,-1.));
#29477=DIRECTION('center_axis',(0.,0.,1.));
#29478=DIRECTION('ref_axis',(0.5,-0.866025403784438,0.));
#29479=DIRECTION('center_axis',(0.,0.,-1.));
#29480=DIRECTION('ref_axis',(1.,0.,0.));
#29481=DIRECTION('',(-0.707951511576272,0.706261040449544,0.));
#29482=DIRECTION('',(0.257664246944398,-0.966234513897416,0.));
#29483=DIRECTION('center_axis',(-0.966234513897416,-0.257664246944398,0.));
#29484=DIRECTION('ref_axis',(0.257664246944398,-0.966234513897416,0.));
#29485=DIRECTION('',(0.,0.,1.));
#29486=DIRECTION('',(0.,0.,1.));
#29487=DIRECTION('center_axis',(0.706261040449544,0.707951511576272,0.));
#29488=DIRECTION('ref_axis',(-0.707951511576272,0.706261040449544,0.));
#29489=DIRECTION('',(0.,0.,-1.));
#29490=DIRECTION('center_axis',(0.,0.,1.));
#29491=DIRECTION('ref_axis',(0.342020143325668,-0.939692620785909,0.));
#29492=DIRECTION('center_axis',(0.,0.,-1.));
#29493=DIRECTION('ref_axis',(1.,0.,0.));
#29494=DIRECTION('',(-0.57455519472581,0.818465838146948,0.));
#29495=DIRECTION('',(0.0859648855277162,-0.996298167445974,0.));
#29496=DIRECTION('center_axis',(-0.996298167445974,-0.0859648855277162,
0.));
#29497=DIRECTION('ref_axis',(0.0859648855277162,-0.996298167445974,0.));
#29498=DIRECTION('',(0.,0.,1.));
#29499=DIRECTION('',(0.,0.,1.));
#29500=DIRECTION('center_axis',(0.818465838146948,0.57455519472581,0.));
#29501=DIRECTION('ref_axis',(-0.57455519472581,0.818465838146948,0.));
#29502=DIRECTION('',(0.,0.,-1.));
#29503=DIRECTION('center_axis',(0.,0.,1.));
#29504=DIRECTION('ref_axis',(0.17364817766693,-0.984807753012208,0.));
#29505=DIRECTION('center_axis',(0.,0.,-1.));
#29506=DIRECTION('ref_axis',(1.,0.,0.));
#29507=DIRECTION('',(-0.423701309022563,0.905801965515955,0.));
#29508=DIRECTION('',(-0.0883464754353936,-0.996089805327885,0.));
#29509=DIRECTION('center_axis',(-0.996089805327885,0.0883464754353937,0.));
#29510=DIRECTION('ref_axis',(-0.0883464754353937,-0.996089805327885,0.));
#29511=DIRECTION('',(0.,0.,1.));
#29512=DIRECTION('',(0.,0.,1.));
#29513=DIRECTION('center_axis',(0.905801965515955,0.423701309022563,0.));
#29514=DIRECTION('ref_axis',(-0.423701309022563,0.905801965515955,0.));
#29515=DIRECTION('',(0.,0.,-1.));
#29516=DIRECTION('center_axis',(0.,0.,1.));
#29517=DIRECTION('ref_axis',(-1.94289029309402E-16,-1.,0.));
#29518=DIRECTION('center_axis',(0.,0.,-1.));
#29519=DIRECTION('ref_axis',(1.,0.,0.));
#29520=DIRECTION('',(-0.259973473447872,0.96561575852067,0.));
#29521=DIRECTION('',(-0.259973473447873,-0.96561575852067,0.));
#29522=DIRECTION('center_axis',(-0.96561575852067,0.259973473447873,0.));
#29523=DIRECTION('ref_axis',(-0.259973473447873,-0.96561575852067,0.));
#29524=DIRECTION('',(0.,0.,1.));
#29525=DIRECTION('',(0.,0.,1.));
#29526=DIRECTION('center_axis',(0.96561575852067,0.259973473447872,0.));
#29527=DIRECTION('ref_axis',(-0.259973473447872,0.96561575852067,0.));
#29528=DIRECTION('',(0.,0.,-1.));
#29529=DIRECTION('center_axis',(0.,0.,1.));
#29530=DIRECTION('ref_axis',(-0.17364817766693,-0.984807753012208,0.));
#29531=DIRECTION('center_axis',(0.,0.,-1.));
#29532=DIRECTION('ref_axis',(1.,0.,0.));
#29533=DIRECTION('',(-0.0883464754353933,0.996089805327885,0.));
#29534=DIRECTION('',(-0.423701309022563,-0.905801965515955,0.));
#29535=DIRECTION('center_axis',(-0.905801965515955,0.423701309022563,0.));
#29536=DIRECTION('ref_axis',(-0.423701309022563,-0.905801965515955,0.));
#29537=DIRECTION('',(0.,0.,1.));
#29538=DIRECTION('',(0.,0.,1.));
#29539=DIRECTION('center_axis',(0.996089805327885,0.0883464754353932,0.));
#29540=DIRECTION('ref_axis',(-0.0883464754353932,0.996089805327885,0.));
#29541=DIRECTION('',(0.,0.,-1.));
#29542=DIRECTION('center_axis',(0.,0.,1.));
#29543=DIRECTION('ref_axis',(-0.342020143325669,-0.939692620785908,0.));
#29544=DIRECTION('center_axis',(0.,0.,-1.));
#29545=DIRECTION('ref_axis',(1.,0.,0.));
#29546=DIRECTION('',(0.0859648855277175,0.996298167445974,0.));
#29547=DIRECTION('',(-0.574555194725811,-0.818465838146947,0.));
#29548=DIRECTION('center_axis',(-0.818465838146947,0.574555194725811,0.));
#29549=DIRECTION('ref_axis',(-0.574555194725811,-0.818465838146947,0.));
#29550=DIRECTION('',(0.,0.,1.));
#29551=DIRECTION('',(0.,0.,1.));
#29552=DIRECTION('center_axis',(0.996298167445974,-0.0859648855277175,0.));
#29553=DIRECTION('ref_axis',(0.0859648855277175,0.996298167445974,0.));
#29554=DIRECTION('',(0.,0.,-1.));
#29555=DIRECTION('center_axis',(0.,0.,1.));
#29556=DIRECTION('ref_axis',(-0.5,-0.866025403784438,0.));
#29557=DIRECTION('center_axis',(0.,0.,-1.));
#29558=DIRECTION('ref_axis',(1.,0.,0.));
#29559=DIRECTION('',(0.257664246944399,0.966234513897416,0.));
#29560=DIRECTION('',(-0.707951511576272,-0.706261040449543,0.));
#29561=DIRECTION('center_axis',(-0.706261040449543,0.707951511576272,0.));
#29562=DIRECTION('ref_axis',(-0.707951511576272,-0.706261040449543,0.));
#29563=DIRECTION('',(0.,0.,1.));
#29564=DIRECTION('',(0.,0.,1.));
#29565=DIRECTION('center_axis',(0.966234513897416,-0.257664246944399,0.));
#29566=DIRECTION('ref_axis',(0.257664246944399,0.966234513897416,0.));
#29567=DIRECTION('',(0.,0.,-1.));
#29568=DIRECTION('center_axis',(0.,0.,1.));
#29569=DIRECTION('ref_axis',(-0.642787609686539,-0.766044443118978,0.));
#29570=DIRECTION('center_axis',(0.,0.,-1.));
#29571=DIRECTION('ref_axis',(1.,0.,0.));
#29572=DIRECTION('',(0.421534610602074,0.906812313582341,0.));
#29573=DIRECTION('',(-0.819837079988238,-0.572596858423411,0.));
#29574=DIRECTION('center_axis',(-0.572596858423411,0.819837079988238,0.));
#29575=DIRECTION('ref_axis',(-0.819837079988238,-0.572596858423411,0.));
#29576=DIRECTION('',(0.,0.,1.));
#29577=DIRECTION('',(0.,0.,1.));
#29578=DIRECTION('center_axis',(0.906812313582341,-0.421534610602074,0.));
#29579=DIRECTION('ref_axis',(0.421534610602074,0.906812313582341,0.));
#29580=DIRECTION('',(0.,0.,-1.));
#29581=DIRECTION('center_axis',(0.,0.,1.));
#29582=DIRECTION('ref_axis',(-0.766044443118978,-0.642787609686539,0.));
#29583=DIRECTION('center_axis',(0.,0.,-1.));
#29584=DIRECTION('ref_axis',(1.,0.,0.));
#29585=DIRECTION('',(0.572596858423411,0.819837079988238,0.));
#29586=DIRECTION('',(-0.906812313582341,-0.421534610602074,0.));
#29587=DIRECTION('center_axis',(-0.421534610602074,0.906812313582341,0.));
#29588=DIRECTION('ref_axis',(-0.906812313582341,-0.421534610602074,0.));
#29589=DIRECTION('',(0.,0.,1.));
#29590=DIRECTION('',(0.,0.,1.));
#29591=DIRECTION('center_axis',(0.819837079988238,-0.572596858423411,0.));
#29592=DIRECTION('ref_axis',(0.572596858423411,0.819837079988238,0.));
#29593=DIRECTION('',(0.,0.,-1.));
#29594=DIRECTION('center_axis',(0.,0.,1.));
#29595=DIRECTION('ref_axis',(-0.866025403784439,-0.5,0.));
#29596=DIRECTION('center_axis',(0.,0.,-1.));
#29597=DIRECTION('ref_axis',(1.,0.,0.));
#29598=DIRECTION('',(0.706261040449544,0.707951511576271,0.));
#29599=DIRECTION('',(-0.966234513897416,-0.257664246944398,0.));
#29600=DIRECTION('center_axis',(-0.257664246944398,0.966234513897416,0.));
#29601=DIRECTION('ref_axis',(-0.966234513897416,-0.257664246944398,0.));
#29602=DIRECTION('',(0.,0.,1.));
#29603=DIRECTION('',(0.,0.,1.));
#29604=DIRECTION('center_axis',(0.707951511576271,-0.706261040449544,0.));
#29605=DIRECTION('ref_axis',(0.706261040449544,0.707951511576271,0.));
#29606=DIRECTION('',(0.,0.,-1.));
#29607=DIRECTION('center_axis',(0.,0.,1.));
#29608=DIRECTION('ref_axis',(-0.939692620785909,-0.342020143325669,0.));
#29609=DIRECTION('center_axis',(0.,0.,-1.));
#29610=DIRECTION('ref_axis',(1.,0.,0.));
#29611=DIRECTION('',(0.818465838146948,0.574555194725811,0.));
#29612=DIRECTION('',(-0.996298167445974,-0.0859648855277167,0.));
#29613=DIRECTION('center_axis',(-0.0859648855277167,0.996298167445974,0.));
#29614=DIRECTION('ref_axis',(-0.996298167445974,-0.0859648855277167,0.));
#29615=DIRECTION('',(0.,0.,1.));
#29616=DIRECTION('',(0.,0.,1.));
#29617=DIRECTION('center_axis',(0.574555194725811,-0.818465838146948,0.));
#29618=DIRECTION('ref_axis',(0.818465838146948,0.574555194725811,0.));
#29619=DIRECTION('',(0.,0.,-1.));
#29620=DIRECTION('center_axis',(0.,0.,1.));
#29621=DIRECTION('ref_axis',(-0.984807753012208,-0.17364817766693,0.));
#29622=DIRECTION('center_axis',(0.,0.,-1.));
#29623=DIRECTION('ref_axis',(1.,0.,0.));
#29624=DIRECTION('',(0.905801965515955,0.423701309022563,0.));
#29625=DIRECTION('',(-0.996089805327885,0.0883464754353936,0.));
#29626=DIRECTION('center_axis',(0.0883464754353936,0.996089805327885,0.));
#29627=DIRECTION('ref_axis',(-0.996089805327885,0.0883464754353936,0.));
#29628=DIRECTION('',(0.,0.,1.));
#29629=DIRECTION('',(0.,0.,1.));
#29630=DIRECTION('center_axis',(0.423701309022563,-0.905801965515955,0.));
#29631=DIRECTION('ref_axis',(0.905801965515955,0.423701309022563,0.));
#29632=DIRECTION('',(0.,0.,-1.));
#29633=DIRECTION('center_axis',(0.,0.,1.));
#29634=DIRECTION('ref_axis',(-1.,1.11022302462516E-16,0.));
#29635=DIRECTION('center_axis',(0.,0.,-1.));
#29636=DIRECTION('ref_axis',(1.,0.,0.));
#29637=DIRECTION('',(0.96561575852067,0.259973473447872,0.));
#29638=DIRECTION('',(-0.96561575852067,0.259973473447873,0.));
#29639=DIRECTION('center_axis',(0.,0.,-1.));
#29640=DIRECTION('ref_axis',(1.,0.,0.));
#29641=DIRECTION('center_axis',(0.259973473447873,0.96561575852067,0.));
#29642=DIRECTION('ref_axis',(-0.96561575852067,0.259973473447873,0.));
#29643=DIRECTION('',(0.,0.,1.));
#29644=DIRECTION('',(0.,0.,1.));
#29645=DIRECTION('center_axis',(0.259973473447872,-0.96561575852067,0.));
#29646=DIRECTION('ref_axis',(0.96561575852067,0.259973473447872,0.));
#29647=DIRECTION('',(0.,0.,-1.));
#29648=DIRECTION('center_axis',(0.,0.,1.));
#29649=DIRECTION('ref_axis',(-0.984807753012208,0.173648177666931,0.));
#29650=DIRECTION('center_axis',(0.,0.,-1.));
#29651=DIRECTION('ref_axis',(1.,0.,0.));
#29652=DIRECTION('',(0.996089805327885,0.0883464754353928,0.));
#29653=DIRECTION('',(-0.905801965515954,0.423701309022564,0.));
#29654=DIRECTION('center_axis',(0.423701309022564,0.905801965515954,0.));
#29655=DIRECTION('ref_axis',(-0.905801965515954,0.423701309022564,0.));
#29656=DIRECTION('',(0.,0.,1.));
#29657=DIRECTION('',(0.,0.,1.));
#29658=DIRECTION('center_axis',(0.0883464754353928,-0.996089805327885,0.));
#29659=DIRECTION('ref_axis',(0.996089805327885,0.0883464754353928,0.));
#29660=DIRECTION('',(0.,0.,-1.));
#29661=DIRECTION('center_axis',(0.,0.,1.));
#29662=DIRECTION('ref_axis',(-0.939692620785908,0.342020143325669,0.));
#29663=DIRECTION('center_axis',(0.,0.,-1.));
#29664=DIRECTION('ref_axis',(1.,0.,0.));
#29665=DIRECTION('',(0.996298167445974,-0.085964885527717,0.));
#29666=DIRECTION('',(-0.818465838146948,0.574555194725811,0.));
#29667=DIRECTION('center_axis',(0.574555194725811,0.818465838146948,0.));
#29668=DIRECTION('ref_axis',(-0.818465838146948,0.574555194725811,0.));
#29669=DIRECTION('',(0.,0.,1.));
#29670=DIRECTION('',(0.,0.,1.));
#29671=DIRECTION('center_axis',(-0.085964885527717,-0.996298167445974,0.));
#29672=DIRECTION('ref_axis',(0.996298167445974,-0.085964885527717,0.));
#29673=DIRECTION('',(0.,0.,-1.));
#29674=DIRECTION('center_axis',(0.,0.,1.));
#29675=DIRECTION('ref_axis',(-0.866025403784439,0.5,0.));
#29676=DIRECTION('center_axis',(0.,0.,-1.));
#29677=DIRECTION('ref_axis',(1.,0.,0.));
#29678=DIRECTION('',(0.966234513897416,-0.257664246944398,0.));
#29679=DIRECTION('',(-0.706261040449544,0.707951511576272,0.));
#29680=DIRECTION('center_axis',(0.707951511576272,0.706261040449544,0.));
#29681=DIRECTION('ref_axis',(-0.706261040449544,0.707951511576272,0.));
#29682=DIRECTION('',(0.,0.,1.));
#29683=DIRECTION('',(0.,0.,1.));
#29684=DIRECTION('center_axis',(-0.257664246944398,-0.966234513897416,0.));
#29685=DIRECTION('ref_axis',(0.966234513897416,-0.257664246944398,0.));
#29686=DIRECTION('',(0.,0.,-1.));
#29687=DIRECTION('center_axis',(0.,0.,1.));
#29688=DIRECTION('ref_axis',(-0.766044443118978,0.642787609686539,0.));
#29689=DIRECTION('center_axis',(0.,0.,-1.));
#29690=DIRECTION('ref_axis',(1.,0.,0.));
#29691=DIRECTION('',(0.906812313582341,-0.421534610602074,0.));
#29692=DIRECTION('',(-0.572596858423411,0.819837079988238,0.));
#29693=DIRECTION('center_axis',(0.819837079988238,0.572596858423411,0.));
#29694=DIRECTION('ref_axis',(-0.572596858423411,0.819837079988238,0.));
#29695=DIRECTION('',(0.,0.,1.));
#29696=DIRECTION('',(0.,0.,1.));
#29697=DIRECTION('center_axis',(-0.421534610602074,-0.906812313582341,0.));
#29698=DIRECTION('ref_axis',(0.906812313582341,-0.421534610602074,0.));
#29699=DIRECTION('',(0.,0.,-1.));
#29700=DIRECTION('center_axis',(0.,0.,1.));
#29701=DIRECTION('ref_axis',(-0.642787609686539,0.766044443118978,0.));
#29702=DIRECTION('center_axis',(0.,0.,-1.));
#29703=DIRECTION('ref_axis',(1.,0.,0.));
#29704=DIRECTION('',(0.819837079988238,-0.572596858423411,0.));
#29705=DIRECTION('',(-0.421534610602074,0.906812313582341,0.));
#29706=DIRECTION('center_axis',(0.906812313582341,0.421534610602074,0.));
#29707=DIRECTION('ref_axis',(-0.421534610602074,0.906812313582341,0.));
#29708=DIRECTION('',(0.,0.,1.));
#29709=DIRECTION('',(0.,0.,1.));
#29710=DIRECTION('center_axis',(-0.572596858423411,-0.819837079988238,0.));
#29711=DIRECTION('ref_axis',(0.819837079988238,-0.572596858423411,0.));
#29712=DIRECTION('',(0.,0.,-1.));
#29713=DIRECTION('center_axis',(0.,0.,1.));
#29714=DIRECTION('ref_axis',(-0.5,0.866025403784439,0.));
#29715=DIRECTION('center_axis',(0.,0.,-1.));
#29716=DIRECTION('ref_axis',(1.,0.,0.));
#29717=DIRECTION('',(0.707951511576272,-0.706261040449544,0.));
#29718=DIRECTION('',(-0.257664246944398,0.966234513897416,0.));
#29719=DIRECTION('center_axis',(0.966234513897416,0.257664246944398,0.));
#29720=DIRECTION('ref_axis',(-0.257664246944398,0.966234513897416,0.));
#29721=DIRECTION('',(0.,0.,1.));
#29722=DIRECTION('',(0.,0.,1.));
#29723=DIRECTION('center_axis',(-0.706261040449544,-0.707951511576272,0.));
#29724=DIRECTION('ref_axis',(0.707951511576272,-0.706261040449544,0.));
#29725=DIRECTION('',(0.,0.,-1.));
#29726=DIRECTION('center_axis',(0.,0.,1.));
#29727=DIRECTION('ref_axis',(-0.342020143325669,0.939692620785909,0.));
#29728=DIRECTION('center_axis',(0.,0.,-1.));
#29729=DIRECTION('ref_axis',(1.,0.,0.));
#29730=DIRECTION('',(0.574555194725811,-0.818465838146948,0.));
#29731=DIRECTION('',(-0.0859648855277167,0.996298167445974,0.));
#29732=DIRECTION('center_axis',(0.996298167445974,0.0859648855277167,0.));
#29733=DIRECTION('ref_axis',(-0.0859648855277167,0.996298167445974,0.));
#29734=DIRECTION('',(0.,0.,1.));
#29735=DIRECTION('',(0.,0.,1.));
#29736=DIRECTION('center_axis',(-0.818465838146948,-0.574555194725811,0.));
#29737=DIRECTION('ref_axis',(0.574555194725811,-0.818465838146948,0.));
#29738=DIRECTION('',(0.,0.,-1.));
#29739=DIRECTION('center_axis',(0.,0.,1.));
#29740=DIRECTION('ref_axis',(-0.17364817766693,0.984807753012208,0.));
#29741=DIRECTION('center_axis',(0.,0.,-1.));
#29742=DIRECTION('ref_axis',(1.,0.,0.));
#29743=DIRECTION('',(0.423701309022563,-0.905801965515955,0.));
#29744=DIRECTION('',(0.0883464754353932,0.996089805327885,0.));
#29745=DIRECTION('center_axis',(0.996089805327885,-0.0883464754353932,0.));
#29746=DIRECTION('ref_axis',(0.0883464754353932,0.996089805327885,0.));
#29747=DIRECTION('',(0.,0.,1.));
#29748=DIRECTION('',(0.,0.,1.));
#29749=DIRECTION('center_axis',(-0.905801965515955,-0.423701309022563,0.));
#29750=DIRECTION('ref_axis',(0.423701309022563,-0.905801965515955,0.));
#29751=DIRECTION('',(0.,0.,-1.));
#29752=DIRECTION('center_axis',(0.,0.,1.));
#29753=DIRECTION('ref_axis',(5.55111512312578E-17,1.,0.));
#29754=DIRECTION('center_axis',(0.,0.,-1.));
#29755=DIRECTION('ref_axis',(1.,0.,0.));
#29756=DIRECTION('',(0.259973473447872,-0.96561575852067,0.));
#29757=DIRECTION('',(0.259973473447872,0.96561575852067,0.));
#29758=DIRECTION('center_axis',(0.96561575852067,-0.259973473447873,0.));
#29759=DIRECTION('ref_axis',(0.259973473447873,0.96561575852067,0.));
#29760=DIRECTION('',(0.,0.,1.));
#29761=DIRECTION('',(0.,0.,1.));
#29762=DIRECTION('center_axis',(-0.96561575852067,-0.259973473447872,0.));
#29763=DIRECTION('ref_axis',(0.259973473447872,-0.96561575852067,0.));
#29764=DIRECTION('',(0.,0.,-1.));
#29765=DIRECTION('center_axis',(0.,0.,1.));
#29766=DIRECTION('ref_axis',(0.17364817766693,0.984807753012208,0.));
#29767=DIRECTION('center_axis',(0.,0.,-1.));
#29768=DIRECTION('ref_axis',(1.,0.,0.));
#29769=DIRECTION('',(0.0883464754353931,-0.996089805327885,0.));
#29770=DIRECTION('',(0.423701309022563,0.905801965515954,0.));
#29771=DIRECTION('center_axis',(0.905801965515954,-0.423701309022563,0.));
#29772=DIRECTION('ref_axis',(0.423701309022563,0.905801965515954,0.));
#29773=DIRECTION('',(0.,0.,1.));
#29774=DIRECTION('',(0.,0.,1.));
#29775=DIRECTION('center_axis',(-0.996089805327885,-0.0883464754353932,
0.));
#29776=DIRECTION('ref_axis',(0.0883464754353932,-0.996089805327885,0.));
#29777=DIRECTION('',(0.,0.,-1.));
#29778=DIRECTION('center_axis',(0.,0.,1.));
#29779=DIRECTION('ref_axis',(0.342020143325669,0.939692620785908,0.));
#29780=DIRECTION('center_axis',(0.,0.,-1.));
#29781=DIRECTION('ref_axis',(1.,0.,0.));
#29782=DIRECTION('',(-0.085964885527717,-0.996298167445974,0.));
#29783=DIRECTION('',(0.574555194725811,0.818465838146948,0.));
#29784=DIRECTION('center_axis',(0.818465838146948,-0.574555194725811,0.));
#29785=DIRECTION('ref_axis',(0.574555194725811,0.818465838146948,0.));
#29786=DIRECTION('',(0.,0.,1.));
#29787=DIRECTION('',(0.,0.,1.));
#29788=DIRECTION('center_axis',(-0.996298167445974,0.085964885527717,0.));
#29789=DIRECTION('ref_axis',(-0.085964885527717,-0.996298167445974,0.));
#29790=DIRECTION('',(0.,0.,-1.));
#29791=DIRECTION('center_axis',(0.,0.,1.));
#29792=DIRECTION('ref_axis',(0.5,0.866025403784439,0.));
#29793=DIRECTION('center_axis',(0.,0.,-1.));
#29794=DIRECTION('ref_axis',(1.,0.,0.));
#29795=DIRECTION('',(-0.257664246944398,-0.966234513897416,0.));
#29796=DIRECTION('',(0.707951511576272,0.706261040449544,0.));
#29797=DIRECTION('center_axis',(0.706261040449544,-0.707951511576272,0.));
#29798=DIRECTION('ref_axis',(0.707951511576272,0.706261040449544,0.));
#29799=DIRECTION('',(0.,0.,1.));
#29800=DIRECTION('',(0.,0.,1.));
#29801=DIRECTION('center_axis',(-0.966234513897416,0.257664246944398,0.));
#29802=DIRECTION('ref_axis',(-0.257664246944398,-0.966234513897416,0.));
#29803=DIRECTION('',(0.,0.,-1.));
#29804=DIRECTION('center_axis',(0.,0.,1.));
#29805=DIRECTION('ref_axis',(0.642787609686539,0.766044443118978,0.));
#29806=DIRECTION('center_axis',(0.,0.,-1.));
#29807=DIRECTION('ref_axis',(1.,0.,0.));
#29808=DIRECTION('',(-0.421534610602074,-0.906812313582341,0.));
#29809=DIRECTION('',(0.819837079988238,0.572596858423411,0.));
#29810=DIRECTION('center_axis',(0.572596858423411,-0.819837079988238,0.));
#29811=DIRECTION('ref_axis',(0.819837079988238,0.572596858423411,0.));
#29812=DIRECTION('',(0.,0.,1.));
#29813=DIRECTION('',(0.,0.,1.));
#29814=DIRECTION('center_axis',(-0.906812313582341,0.421534610602074,0.));
#29815=DIRECTION('ref_axis',(-0.421534610602074,-0.906812313582341,0.));
#29816=DIRECTION('',(0.,0.,-1.));
#29817=DIRECTION('center_axis',(0.,0.,1.));
#29818=DIRECTION('ref_axis',(0.766044443118978,0.642787609686539,0.));
#29819=DIRECTION('center_axis',(0.,0.,-1.));
#29820=DIRECTION('ref_axis',(1.,0.,0.));
#29821=DIRECTION('',(-0.572596858423411,-0.819837079988238,0.));
#29822=DIRECTION('',(0.906812313582341,0.421534610602074,0.));
#29823=DIRECTION('center_axis',(0.421534610602074,-0.906812313582341,0.));
#29824=DIRECTION('ref_axis',(0.906812313582341,0.421534610602074,0.));
#29825=DIRECTION('',(0.,0.,1.));
#29826=DIRECTION('',(0.,0.,1.));
#29827=DIRECTION('center_axis',(-0.819837079988238,0.572596858423411,0.));
#29828=DIRECTION('ref_axis',(-0.572596858423411,-0.819837079988238,0.));
#29829=DIRECTION('',(0.,0.,-1.));
#29830=DIRECTION('center_axis',(0.,0.,1.));
#29831=DIRECTION('ref_axis',(0.866025403784439,0.5,0.));
#29832=DIRECTION('center_axis',(0.,0.,-1.));
#29833=DIRECTION('ref_axis',(1.,0.,0.));
#29834=DIRECTION('',(-0.706261040449544,-0.707951511576272,0.));
#29835=DIRECTION('',(0.966234513897416,0.257664246944398,0.));
#29836=DIRECTION('center_axis',(0.257664246944398,-0.966234513897416,0.));
#29837=DIRECTION('ref_axis',(0.966234513897416,0.257664246944398,0.));
#29838=DIRECTION('',(0.,0.,1.));
#29839=DIRECTION('',(0.,0.,1.));
#29840=DIRECTION('center_axis',(-0.707951511576272,0.706261040449544,0.));
#29841=DIRECTION('ref_axis',(-0.706261040449544,-0.707951511576272,0.));
#29842=DIRECTION('',(0.,0.,-1.));
#29843=DIRECTION('center_axis',(0.,0.,1.));
#29844=DIRECTION('ref_axis',(0.939692620785909,0.342020143325669,0.));
#29845=DIRECTION('center_axis',(0.,0.,-1.));
#29846=DIRECTION('ref_axis',(1.,0.,0.));
#29847=DIRECTION('',(-0.818465838146948,-0.574555194725811,0.));
#29848=DIRECTION('',(0.996298167445974,0.0859648855277167,0.));
#29849=DIRECTION('center_axis',(0.0859648855277167,-0.996298167445974,0.));
#29850=DIRECTION('ref_axis',(0.996298167445974,0.0859648855277167,0.));
#29851=DIRECTION('',(0.,0.,1.));
#29852=DIRECTION('',(0.,0.,1.));
#29853=DIRECTION('center_axis',(-0.574555194725811,0.818465838146948,0.));
#29854=DIRECTION('ref_axis',(-0.818465838146948,-0.574555194725811,0.));
#29855=DIRECTION('',(0.,0.,-1.));
#29856=DIRECTION('center_axis',(0.,0.,1.));
#29857=DIRECTION('ref_axis',(0.984807753012208,0.17364817766693,0.));
#29858=DIRECTION('center_axis',(0.,0.,-1.));
#29859=DIRECTION('ref_axis',(1.,0.,0.));
#29860=DIRECTION('',(-0.905801965515955,-0.423701309022563,0.));
#29861=DIRECTION('',(0.996089805327885,-0.0883464754353932,0.));
#29862=DIRECTION('center_axis',(-0.0883464754353933,-0.996089805327885,
0.));
#29863=DIRECTION('ref_axis',(0.996089805327885,-0.0883464754353933,0.));
#29864=DIRECTION('',(0.,0.,1.));
#29865=DIRECTION('',(0.,0.,1.));
#29866=DIRECTION('center_axis',(-0.423701309022563,0.905801965515955,0.));
#29867=DIRECTION('ref_axis',(-0.905801965515954,-0.423701309022563,0.));
#29868=DIRECTION('',(0.,0.,-1.));
#29869=DIRECTION('center_axis',(0.,0.,1.));
#29870=DIRECTION('ref_axis',(1.,0.,0.));
#29871=DIRECTION('center_axis',(0.,0.,1.));
#29872=DIRECTION('ref_axis',(1.,0.,0.));
#29873=DIRECTION('center_axis',(0.,0.,1.));
#29874=DIRECTION('ref_axis',(1.,0.,0.));
#29875=DIRECTION('center_axis',(0.,0.,1.));
#29876=DIRECTION('ref_axis',(1.,0.,0.));
#29877=DIRECTION('center_axis',(0.,0.,1.));
#29878=DIRECTION('ref_axis',(1.,0.,0.));
#29879=DIRECTION('center_axis',(0.,0.,1.));
#29880=DIRECTION('ref_axis',(1.,0.,0.));
#29881=DIRECTION('center_axis',(0.,0.,1.));
#29882=DIRECTION('ref_axis',(1.,0.,0.));
#29883=DIRECTION('center_axis',(0.,0.,1.));
#29884=DIRECTION('ref_axis',(1.,0.,0.));
#29885=DIRECTION('center_axis',(0.,0.,1.));
#29886=DIRECTION('ref_axis',(1.,0.,0.));
#29887=DIRECTION('center_axis',(0.,0.,1.));
#29888=DIRECTION('ref_axis',(1.,0.,0.));
#29889=DIRECTION('center_axis',(0.,0.,1.));
#29890=DIRECTION('ref_axis',(1.,0.,0.));
#29891=DIRECTION('center_axis',(0.,0.,1.));
#29892=DIRECTION('ref_axis',(1.,0.,0.));
#29893=DIRECTION('center_axis',(0.,0.,1.));
#29894=DIRECTION('ref_axis',(1.,0.,0.));
#29895=DIRECTION('center_axis',(0.,0.,1.));
#29896=DIRECTION('ref_axis',(1.,0.,0.));
#29897=DIRECTION('center_axis',(0.,0.,1.));
#29898=DIRECTION('ref_axis',(1.,0.,0.));
#29899=DIRECTION('center_axis',(0.,0.,1.));
#29900=DIRECTION('ref_axis',(1.,0.,0.));
#29901=DIRECTION('center_axis',(0.,0.,1.));
#29902=DIRECTION('ref_axis',(1.,0.,0.));
#29903=DIRECTION('center_axis',(0.,0.,1.));
#29904=DIRECTION('ref_axis',(1.,0.,0.));
#29905=DIRECTION('',(0.,0.,-1.));
#29906=DIRECTION('center_axis',(0.,0.,1.));
#29907=DIRECTION('ref_axis',(1.,0.,0.));
#29908=DIRECTION('center_axis',(0.,0.,1.));
#29909=DIRECTION('ref_axis',(1.,0.,0.));
#29910=DIRECTION('center_axis',(0.,0.,1.));
#29911=DIRECTION('ref_axis',(1.,0.,0.));
#29912=DIRECTION('center_axis',(0.,0.,1.));
#29913=DIRECTION('ref_axis',(1.,0.,0.));
#29914=DIRECTION('center_axis',(0.,0.,1.));
#29915=DIRECTION('ref_axis',(1.,0.,0.));
#29916=DIRECTION('center_axis',(0.,0.,1.));
#29917=DIRECTION('ref_axis',(1.,0.,0.));
#29918=DIRECTION('center_axis',(0.,0.,1.));
#29919=DIRECTION('ref_axis',(1.,0.,0.));
#29920=DIRECTION('center_axis',(0.,0.,1.));
#29921=DIRECTION('ref_axis',(1.,0.,0.));
#29922=DIRECTION('center_axis',(0.,0.,1.));
#29923=DIRECTION('ref_axis',(1.,0.,0.));
#29924=DIRECTION('center_axis',(0.,0.,1.));
#29925=DIRECTION('ref_axis',(1.,0.,0.));
#29926=DIRECTION('center_axis',(0.,0.,1.));
#29927=DIRECTION('ref_axis',(1.,0.,0.));
#29928=DIRECTION('center_axis',(0.,0.,1.));
#29929=DIRECTION('ref_axis',(1.,0.,0.));
#29930=DIRECTION('center_axis',(0.,0.,1.));
#29931=DIRECTION('ref_axis',(1.,0.,0.));
#29932=DIRECTION('center_axis',(0.,0.,1.));
#29933=DIRECTION('ref_axis',(1.,0.,0.));
#29934=DIRECTION('center_axis',(0.,0.,1.));
#29935=DIRECTION('ref_axis',(1.,0.,0.));
#29936=DIRECTION('center_axis',(0.,0.,1.));
#29937=DIRECTION('ref_axis',(1.,0.,0.));
#29938=DIRECTION('center_axis',(0.,0.,1.));
#29939=DIRECTION('ref_axis',(1.,0.,0.));
#29940=DIRECTION('center_axis',(0.,0.,1.));
#29941=DIRECTION('ref_axis',(1.,0.,0.));
#29942=DIRECTION('center_axis',(0.,0.,1.));
#29943=DIRECTION('ref_axis',(1.,0.,0.));
#29944=DIRECTION('',(0.,0.,-1.));
#29945=DIRECTION('center_axis',(0.,0.,-1.));
#29946=DIRECTION('ref_axis',(1.,0.,0.));
#29947=DIRECTION('',(0.,0.,1.));
#29948=DIRECTION('center_axis',(0.,0.,1.));
#29949=DIRECTION('ref_axis',(1.,0.,0.));
#29950=DIRECTION('center_axis',(-0.259973473447872,-0.96561575852067,0.));
#29951=DIRECTION('ref_axis',(0.96561575852067,-0.259973473447872,0.));
#29952=DIRECTION('',(0.96561575852067,-0.259973473447872,0.));
#29953=DIRECTION('',(0.,0.,1.));
#29954=DIRECTION('center_axis',(-0.259973473447872,0.96561575852067,0.));
#29955=DIRECTION('ref_axis',(-0.96561575852067,-0.259973473447872,0.));
#29956=DIRECTION('',(-0.96561575852067,-0.259973473447872,0.));
#29957=DIRECTION('center_axis',(0.,0.,1.));
#29958=DIRECTION('ref_axis',(1.,0.,0.));
#29959=DIRECTION('center_axis',(0.,0.,-1.));
#29960=DIRECTION('ref_axis',(1.,0.,0.));
#29961=DIRECTION('center_axis',(0.,0.,1.));
#29962=DIRECTION('ref_axis',(1.,0.,0.));
#29963=DIRECTION('',(-0.707106781186549,-8.65956056235495E-17,-0.707106781186546));
#29964=DIRECTION('center_axis',(0.,0.,1.));
#29965=DIRECTION('ref_axis',(1.,0.,0.));
#29966=DIRECTION('',(-0.844694227521705,-1.0344520819927E-16,0.535249158795705));
#29967=DIRECTION('center_axis',(0.,0.,-1.));
#29968=DIRECTION('ref_axis',(1.,0.,0.));
#29969=DIRECTION('center_axis',(0.5,0.866025403784439,0.));
#29970=DIRECTION('ref_axis',(0.866025403784439,-0.5,0.));
#29971=DIRECTION('',(0.866025403784439,-0.5,0.));
#29972=DIRECTION('',(0.,0.,-1.));
#29973=DIRECTION('',(0.866025403784439,-0.5,0.));
#29974=DIRECTION('',(0.,0.,-1.));
#29975=DIRECTION('center_axis',(-0.5,0.866025403784439,0.));
#29976=DIRECTION('ref_axis',(0.866025403784439,0.5,0.));
#29977=DIRECTION('',(0.866025403784439,0.5,0.));
#29978=DIRECTION('',(0.,0.,-1.));
#29979=DIRECTION('',(0.866025403784439,0.5,0.));
#29980=DIRECTION('center_axis',(-1.,-1.92296268638356E-16,0.));
#29981=DIRECTION('ref_axis',(-1.92296268638356E-16,1.,0.));
#29982=DIRECTION('',(-1.92296268638356E-16,1.,0.));
#29983=DIRECTION('',(0.,0.,-1.));
#29984=DIRECTION('',(-1.92296268638356E-16,1.,0.));
#29985=DIRECTION('center_axis',(-0.5,-0.866025403784439,0.));
#29986=DIRECTION('ref_axis',(-0.866025403784439,0.5,0.));
#29987=DIRECTION('',(-0.866025403784439,0.5,0.));
#29988=DIRECTION('',(0.,0.,-1.));
#29989=DIRECTION('',(-0.866025403784439,0.5,0.));
#29990=DIRECTION('center_axis',(0.5,-0.866025403784439,0.));
#29991=DIRECTION('ref_axis',(-0.866025403784439,-0.5,0.));
#29992=DIRECTION('',(-0.866025403784439,-0.5,0.));
#29993=DIRECTION('',(0.,0.,-1.));
#29994=DIRECTION('',(-0.866025403784439,-0.5,0.));
#29995=DIRECTION('center_axis',(1.,-3.84592537276713E-16,0.));
#29996=DIRECTION('ref_axis',(-3.84592537276713E-16,-1.,0.));
#29997=DIRECTION('',(-3.84592537276713E-16,-1.,0.));
#29998=DIRECTION('',(-3.84592537276713E-16,-1.,0.));
#29999=DIRECTION('center_axis',(0.,0.,-1.));
#30000=DIRECTION('ref_axis',(-1.,0.,0.));
#30001=DIRECTION('center_axis',(0.,0.,-1.));
#30002=DIRECTION('ref_axis',(-1.,0.,0.));
#30003=DIRECTION('center_axis',(0.,0.,1.));
#30004=DIRECTION('ref_axis',(1.,0.,0.));
#30005=DIRECTION('center_axis',(0.,0.,1.));
#30006=DIRECTION('ref_axis',(1.,0.,0.));
#30007=DIRECTION('',(0.707106781186547,8.65956056235493E-17,-0.707106781186548));
#30008=DIRECTION('center_axis',(0.,0.,1.));
#30009=DIRECTION('ref_axis',(0.952262827709432,-0.305279391644502,0.));
#30010=DIRECTION('center_axis',(0.,0.,1.));
#30011=DIRECTION('ref_axis',(1.,0.,0.));
#30012=DIRECTION('center_axis',(0.,0.,1.));
#30013=DIRECTION('ref_axis',(1.,0.,0.));
#30014=DIRECTION('center_axis',(0.,0.,1.));
#30015=DIRECTION('ref_axis',(1.,0.,0.));
#30016=DIRECTION('',(0.707106781186548,8.65956056235494E-17,-0.707106781186547));
#30017=DIRECTION('center_axis',(0.,0.,-1.));
#30018=DIRECTION('ref_axis',(-1.,0.,0.));
#30019=DIRECTION('center_axis',(0.,0.,1.));
#30020=DIRECTION('ref_axis',(1.,0.,0.));
#30021=DIRECTION('axis',(0.,0.,1.));
#30022=DIRECTION('refdir',(1.,0.,0.));
#30023=DIRECTION('center_axis',(0.,0.,1.));
#30024=DIRECTION('ref_axis',(1.,0.,0.));
#30025=DIRECTION('',(0.,0.,-1.));
#30026=DIRECTION('center_axis',(0.,0.,-1.));
#30027=DIRECTION('ref_axis',(1.,0.,0.));
#30028=DIRECTION('',(0.,0.,-1.));
#30029=DIRECTION('center_axis',(0.,0.,1.));
#30030=DIRECTION('ref_axis',(1.,0.,0.));
#30031=DIRECTION('center_axis',(0.,0.,-1.));
#30032=DIRECTION('ref_axis',(1.,0.,0.));
#30033=DIRECTION('center_axis',(0.,0.,1.));
#30034=DIRECTION('ref_axis',(1.,0.,0.));
#30035=DIRECTION('',(0.,0.,-1.));
#30036=DIRECTION('center_axis',(0.,0.,1.));
#30037=DIRECTION('ref_axis',(1.,0.,0.));
#30038=DIRECTION('',(0.,0.,-1.));
#30039=DIRECTION('center_axis',(0.,0.,1.));
#30040=DIRECTION('ref_axis',(1.,0.,0.));
#30041=DIRECTION('',(0.,0.,-1.));
#30042=DIRECTION('center_axis',(0.,0.,1.));
#30043=DIRECTION('ref_axis',(1.,0.,0.));
#30044=DIRECTION('',(0.,0.,-1.));
#30045=DIRECTION('center_axis',(0.,0.,1.));
#30046=DIRECTION('ref_axis',(1.,0.,0.));
#30047=DIRECTION('',(0.,0.,-1.));
#30048=DIRECTION('center_axis',(0.,0.,1.));
#30049=DIRECTION('ref_axis',(1.,0.,0.));
#30050=DIRECTION('',(0.,0.,-1.));
#30051=DIRECTION('center_axis',(0.,0.,1.));
#30052=DIRECTION('ref_axis',(1.,0.,0.));
#30053=DIRECTION('',(0.,0.,-1.));
#30054=DIRECTION('center_axis',(0.,0.,1.));
#30055=DIRECTION('ref_axis',(1.,0.,0.));
#30056=DIRECTION('',(0.,0.,-1.));
#30057=DIRECTION('center_axis',(0.,0.,1.));
#30058=DIRECTION('ref_axis',(1.,0.,0.));
#30059=DIRECTION('',(0.,0.,-1.));
#30060=DIRECTION('center_axis',(0.,0.,1.));
#30061=DIRECTION('ref_axis',(1.,0.,0.));
#30062=DIRECTION('',(0.,0.,-1.));
#30063=DIRECTION('center_axis',(0.,0.,1.));
#30064=DIRECTION('ref_axis',(1.,0.,0.));
#30065=DIRECTION('',(0.,0.,-1.));
#30066=DIRECTION('center_axis',(0.,0.,1.));
#30067=DIRECTION('ref_axis',(1.,0.,0.));
#30068=DIRECTION('',(0.,0.,-1.));
#30069=DIRECTION('center_axis',(0.,0.,1.));
#30070=DIRECTION('ref_axis',(1.,0.,0.));
#30071=DIRECTION('',(0.,0.,-1.));
#30072=DIRECTION('center_axis',(0.,0.,1.));
#30073=DIRECTION('ref_axis',(1.,0.,0.));
#30074=DIRECTION('',(0.,0.,-1.));
#30075=DIRECTION('center_axis',(0.,0.,1.));
#30076=DIRECTION('ref_axis',(1.,0.,0.));
#30077=DIRECTION('',(0.,0.,-1.));
#30078=DIRECTION('center_axis',(0.,0.,1.));
#30079=DIRECTION('ref_axis',(1.,0.,0.));
#30080=DIRECTION('',(0.,0.,-1.));
#30081=DIRECTION('center_axis',(0.,0.,1.));
#30082=DIRECTION('ref_axis',(1.,0.,0.));
#30083=DIRECTION('',(0.,0.,-1.));
#30084=DIRECTION('center_axis',(0.,0.,1.));
#30085=DIRECTION('ref_axis',(1.,0.,0.));
#30086=DIRECTION('',(0.,0.,-1.));
#30087=DIRECTION('center_axis',(0.,0.,1.));
#30088=DIRECTION('ref_axis',(1.,0.,0.));
#30089=DIRECTION('',(0.,0.,-1.));
#30090=DIRECTION('center_axis',(0.,0.,1.));
#30091=DIRECTION('ref_axis',(1.,0.,0.));
#30092=DIRECTION('',(0.,0.,-1.));
#30093=DIRECTION('center_axis',(0.,0.,1.));
#30094=DIRECTION('ref_axis',(1.,0.,0.));
#30095=DIRECTION('',(0.,0.,-1.));
#30096=DIRECTION('center_axis',(0.,0.,1.));
#30097=DIRECTION('ref_axis',(1.,0.,0.));
#30098=DIRECTION('',(0.,0.,-1.));
#30099=DIRECTION('center_axis',(0.,0.,1.));
#30100=DIRECTION('ref_axis',(1.,0.,0.));
#30101=DIRECTION('',(0.,0.,-1.));
#30102=DIRECTION('center_axis',(0.,0.,1.));
#30103=DIRECTION('ref_axis',(1.,0.,0.));
#30104=DIRECTION('',(0.,0.,-1.));
#30105=DIRECTION('center_axis',(0.,0.,1.));
#30106=DIRECTION('ref_axis',(1.,0.,0.));
#30107=DIRECTION('',(0.,0.,-1.));
#30108=DIRECTION('center_axis',(0.,0.,1.));
#30109=DIRECTION('ref_axis',(1.,0.,0.));
#30110=DIRECTION('',(0.,0.,-1.));
#30111=DIRECTION('center_axis',(0.,0.,1.));
#30112=DIRECTION('ref_axis',(1.,0.,0.));
#30113=DIRECTION('',(0.,0.,-1.));
#30114=DIRECTION('center_axis',(0.,0.,1.));
#30115=DIRECTION('ref_axis',(1.,0.,0.));
#30116=DIRECTION('',(0.,0.,-1.));
#30117=DIRECTION('center_axis',(0.,0.,1.));
#30118=DIRECTION('ref_axis',(1.,0.,0.));
#30119=DIRECTION('',(0.,0.,-1.));
#30120=DIRECTION('center_axis',(0.,0.,1.));
#30121=DIRECTION('ref_axis',(1.,0.,0.));
#30122=DIRECTION('',(0.,0.,-1.));
#30123=DIRECTION('center_axis',(0.,0.,1.));
#30124=DIRECTION('ref_axis',(1.,0.,0.));
#30125=DIRECTION('',(0.,0.,-1.));
#30126=DIRECTION('center_axis',(0.,0.,1.));
#30127=DIRECTION('ref_axis',(1.,0.,0.));
#30128=DIRECTION('',(0.,0.,-1.));
#30129=DIRECTION('center_axis',(0.,0.,1.));
#30130=DIRECTION('ref_axis',(1.,0.,0.));
#30131=DIRECTION('',(0.,0.,-1.));
#30132=DIRECTION('center_axis',(0.,0.,1.));
#30133=DIRECTION('ref_axis',(1.,0.,0.));
#30134=DIRECTION('',(0.,0.,-1.));
#30135=DIRECTION('center_axis',(0.,0.,1.));
#30136=DIRECTION('ref_axis',(1.,0.,0.));
#30137=DIRECTION('',(0.,0.,-1.));
#30138=DIRECTION('center_axis',(0.,0.,1.));
#30139=DIRECTION('ref_axis',(1.,0.,0.));
#30140=DIRECTION('',(0.,0.,-1.));
#30141=DIRECTION('center_axis',(0.,0.,1.));
#30142=DIRECTION('ref_axis',(1.,0.,0.));
#30143=DIRECTION('',(0.,0.,-1.));
#30144=DIRECTION('center_axis',(0.,0.,1.));
#30145=DIRECTION('ref_axis',(1.,0.,0.));
#30146=DIRECTION('',(0.,0.,-1.));
#30147=DIRECTION('center_axis',(0.,0.,1.));
#30148=DIRECTION('ref_axis',(1.,0.,0.));
#30149=DIRECTION('',(0.,0.,-1.));
#30150=DIRECTION('center_axis',(0.,0.,1.));
#30151=DIRECTION('ref_axis',(1.,0.,0.));
#30152=DIRECTION('',(0.,0.,-1.));
#30153=DIRECTION('center_axis',(0.,0.,1.));
#30154=DIRECTION('ref_axis',(1.,0.,0.));
#30155=DIRECTION('',(0.,0.,-1.));
#30156=DIRECTION('center_axis',(0.,0.,1.));
#30157=DIRECTION('ref_axis',(1.,0.,0.));
#30158=DIRECTION('',(0.,0.,-1.));
#30159=DIRECTION('center_axis',(0.,0.,1.));
#30160=DIRECTION('ref_axis',(1.,0.,0.));
#30161=DIRECTION('',(0.,0.,-1.));
#30162=DIRECTION('center_axis',(0.,0.,1.));
#30163=DIRECTION('ref_axis',(1.,0.,0.));
#30164=DIRECTION('',(0.,0.,-1.));
#30165=DIRECTION('center_axis',(0.,0.,1.));
#30166=DIRECTION('ref_axis',(1.,0.,0.));
#30167=DIRECTION('',(0.,0.,-1.));
#30168=DIRECTION('center_axis',(0.,0.,1.));
#30169=DIRECTION('ref_axis',(1.,0.,0.));
#30170=DIRECTION('',(0.,0.,-1.));
#30171=DIRECTION('center_axis',(0.,0.,1.));
#30172=DIRECTION('ref_axis',(1.,0.,0.));
#30173=DIRECTION('',(0.,0.,-1.));
#30174=DIRECTION('center_axis',(0.,0.,1.));
#30175=DIRECTION('ref_axis',(1.,0.,0.));
#30176=DIRECTION('',(0.,0.,-1.));
#30177=DIRECTION('center_axis',(0.,0.,1.));
#30178=DIRECTION('ref_axis',(1.,0.,0.));
#30179=DIRECTION('',(0.,0.,-1.));
#30180=DIRECTION('center_axis',(0.,0.,1.));
#30181=DIRECTION('ref_axis',(1.,0.,0.));
#30182=DIRECTION('',(0.,0.,-1.));
#30183=DIRECTION('center_axis',(0.,0.,1.));
#30184=DIRECTION('ref_axis',(1.,0.,0.));
#30185=DIRECTION('',(0.,0.,-1.));
#30186=DIRECTION('center_axis',(0.,0.,1.));
#30187=DIRECTION('ref_axis',(1.,0.,0.));
#30188=DIRECTION('',(0.,0.,-1.));
#30189=DIRECTION('center_axis',(0.,0.,1.));
#30190=DIRECTION('ref_axis',(1.,0.,0.));
#30191=DIRECTION('',(0.,0.,-1.));
#30192=DIRECTION('center_axis',(0.,0.,1.));
#30193=DIRECTION('ref_axis',(1.,0.,0.));
#30194=DIRECTION('',(0.,0.,-1.));
#30195=DIRECTION('center_axis',(0.,0.,1.));
#30196=DIRECTION('ref_axis',(1.,0.,0.));
#30197=DIRECTION('',(0.,0.,-1.));
#30198=DIRECTION('center_axis',(0.,0.,1.));
#30199=DIRECTION('ref_axis',(1.,0.,0.));
#30200=DIRECTION('',(0.,0.,-1.));
#30201=DIRECTION('center_axis',(0.,0.,1.));
#30202=DIRECTION('ref_axis',(1.,0.,0.));
#30203=DIRECTION('',(0.,0.,-1.));
#30204=DIRECTION('center_axis',(0.,0.,1.));
#30205=DIRECTION('ref_axis',(-0.222283644230434,-0.974982041633402,0.));
#30206=DIRECTION('',(0.,0.,1.));
#30207=DIRECTION('center_axis',(0.,0.,1.));
#30208=DIRECTION('ref_axis',(1.,-9.62097198987423E-13,0.));
#30209=DIRECTION('center_axis',(0.,0.,1.));
#30210=DIRECTION('ref_axis',(1.,-9.62097198987423E-13,0.));
#30211=DIRECTION('',(0.,0.,1.));
#30212=DIRECTION('center_axis',(0.,0.,1.));
#30213=DIRECTION('ref_axis',(1.,-9.62097198987423E-13,0.));
#30214=DIRECTION('',(0.,0.,1.));
#30215=DIRECTION('center_axis',(0.,0.,1.));
#30216=DIRECTION('ref_axis',(1.,-9.62097198987423E-13,0.));
#30217=DIRECTION('',(0.,0.,1.));
#30218=DIRECTION('center_axis',(0.,0.,1.));
#30219=DIRECTION('ref_axis',(1.,-9.62097198987423E-13,0.));
#30220=DIRECTION('',(0.,0.,1.));
#30221=DIRECTION('center_axis',(0.,0.,1.));
#30222=DIRECTION('ref_axis',(1.,-9.62097198987423E-13,0.));
#30223=DIRECTION('',(0.,0.,1.));
#30224=DIRECTION('center_axis',(0.,0.,1.));
#30225=DIRECTION('ref_axis',(1.,-9.62097198987423E-13,0.));
#30226=DIRECTION('',(0.,0.,1.));
#30227=DIRECTION('center_axis',(0.,0.,1.));
#30228=DIRECTION('ref_axis',(1.,-9.62097198987423E-13,0.));
#30229=DIRECTION('',(0.,0.,1.));
#30230=DIRECTION('center_axis',(0.,0.,1.));
#30231=DIRECTION('ref_axis',(1.,-9.62097198987423E-13,0.));
#30232=DIRECTION('',(0.,0.,1.));
#30233=DIRECTION('center_axis',(0.,0.,1.));
#30234=DIRECTION('ref_axis',(1.,-9.62097198987423E-13,0.));
#30235=DIRECTION('',(0.,0.,1.));
#30236=DIRECTION('center_axis',(0.,0.,1.));
#30237=DIRECTION('ref_axis',(1.,-9.62097198987423E-13,0.));
#30238=DIRECTION('',(0.,0.,1.));
#30239=DIRECTION('center_axis',(0.,0.,1.));
#30240=DIRECTION('ref_axis',(1.,-9.62097198987423E-13,0.));
#30241=DIRECTION('',(0.,0.,1.));
#30242=DIRECTION('center_axis',(0.,0.,1.));
#30243=DIRECTION('ref_axis',(1.,-9.62097198987423E-13,0.));
#30244=DIRECTION('',(0.,0.,1.));
#30245=DIRECTION('center_axis',(0.,0.,1.));
#30246=DIRECTION('ref_axis',(1.,-9.62097198987423E-13,0.));
#30247=DIRECTION('',(0.,0.,1.));
#30248=DIRECTION('center_axis',(0.,0.,1.));
#30249=DIRECTION('ref_axis',(1.,-9.62097198987423E-13,0.));
#30250=DIRECTION('',(0.,0.,1.));
#30251=DIRECTION('center_axis',(0.,0.,1.));
#30252=DIRECTION('ref_axis',(1.,-9.62097198987423E-13,0.));
#30253=DIRECTION('',(0.,0.,1.));
#30254=DIRECTION('center_axis',(0.,0.,1.));
#30255=DIRECTION('ref_axis',(1.,-9.62097198987423E-13,0.));
#30256=DIRECTION('',(0.,0.,1.));
#30257=DIRECTION('center_axis',(0.,0.,1.));
#30258=DIRECTION('ref_axis',(1.,-9.62097198987423E-13,0.));
#30259=DIRECTION('',(0.,0.,1.));
#30260=DIRECTION('center_axis',(0.,0.,1.));
#30261=DIRECTION('ref_axis',(1.,-9.62097198987423E-13,0.));
#30262=DIRECTION('',(0.,0.,1.));
#30263=DIRECTION('center_axis',(0.,0.,1.));
#30264=DIRECTION('ref_axis',(1.,-9.62097198987423E-13,0.));
#30265=DIRECTION('',(0.,0.,1.));
#30266=DIRECTION('center_axis',(0.,0.,1.));
#30267=DIRECTION('ref_axis',(1.,-9.62097198987423E-13,0.));
#30268=DIRECTION('',(0.,0.,1.));
#30269=DIRECTION('center_axis',(0.,0.,1.));
#30270=DIRECTION('ref_axis',(1.,-9.62097198987423E-13,0.));
#30271=DIRECTION('',(0.,0.,1.));
#30272=DIRECTION('center_axis',(0.,0.,1.));
#30273=DIRECTION('ref_axis',(1.,-9.62097198987423E-13,0.));
#30274=DIRECTION('',(0.,0.,1.));
#30275=DIRECTION('center_axis',(0.,0.,1.));
#30276=DIRECTION('ref_axis',(1.,-9.62097198987423E-13,0.));
#30277=DIRECTION('',(0.,0.,1.));
#30278=DIRECTION('center_axis',(0.,0.,1.));
#30279=DIRECTION('ref_axis',(1.,-9.62097198987423E-13,0.));
#30280=DIRECTION('',(0.,0.,1.));
#30281=DIRECTION('center_axis',(0.,0.,1.));
#30282=DIRECTION('ref_axis',(1.,-9.62097198987423E-13,0.));
#30283=DIRECTION('',(0.,0.,1.));
#30284=DIRECTION('center_axis',(0.,0.,1.));
#30285=DIRECTION('ref_axis',(1.,-9.62097198987423E-13,0.));
#30286=DIRECTION('',(0.,0.,1.));
#30287=DIRECTION('center_axis',(0.,0.,1.));
#30288=DIRECTION('ref_axis',(1.,-9.62097198987423E-13,0.));
#30289=DIRECTION('',(0.,0.,1.));
#30290=DIRECTION('center_axis',(0.,0.,1.));
#30291=DIRECTION('ref_axis',(1.,-9.62097198987423E-13,0.));
#30292=DIRECTION('',(0.,0.,1.));
#30293=DIRECTION('center_axis',(0.,0.,1.));
#30294=DIRECTION('ref_axis',(1.,-9.62097198987423E-13,0.));
#30295=DIRECTION('',(0.,0.,1.));
#30296=DIRECTION('center_axis',(0.,0.,1.));
#30297=DIRECTION('ref_axis',(1.,-9.62097198987423E-13,0.));
#30298=DIRECTION('',(0.,0.,1.));
#30299=DIRECTION('center_axis',(0.,0.,1.));
#30300=DIRECTION('ref_axis',(1.,-9.62097198987423E-13,0.));
#30301=DIRECTION('',(0.,0.,1.));
#30302=DIRECTION('center_axis',(0.,0.,1.));
#30303=DIRECTION('ref_axis',(1.,-9.62097198987423E-13,0.));
#30304=DIRECTION('',(0.,0.,1.));
#30305=DIRECTION('center_axis',(0.,0.,1.));
#30306=DIRECTION('ref_axis',(1.,-9.62097198987423E-13,0.));
#30307=DIRECTION('',(0.,0.,1.));
#30308=DIRECTION('center_axis',(0.,0.,1.));
#30309=DIRECTION('ref_axis',(1.,-9.62097198987423E-13,0.));
#30310=DIRECTION('',(0.,0.,1.));
#30311=DIRECTION('center_axis',(0.,0.,1.));
#30312=DIRECTION('ref_axis',(1.,-9.62097198987423E-13,0.));
#30313=DIRECTION('',(0.,0.,1.));
#30314=DIRECTION('center_axis',(0.,0.,1.));
#30315=DIRECTION('ref_axis',(1.,-9.62097198987423E-13,0.));
#30316=DIRECTION('',(0.,0.,1.));
#30317=DIRECTION('center_axis',(0.,0.,1.));
#30318=DIRECTION('ref_axis',(1.,-9.62097198987423E-13,0.));
#30319=DIRECTION('',(0.,0.,1.));
#30320=DIRECTION('center_axis',(0.,0.,1.));
#30321=DIRECTION('ref_axis',(1.,-9.62097198987423E-13,0.));
#30322=DIRECTION('',(0.,0.,1.));
#30323=DIRECTION('center_axis',(0.,0.,1.));
#30324=DIRECTION('ref_axis',(1.,-9.62097198987423E-13,0.));
#30325=DIRECTION('',(0.,0.,1.));
#30326=DIRECTION('center_axis',(0.,0.,1.));
#30327=DIRECTION('ref_axis',(1.,-9.62097198987423E-13,0.));
#30328=DIRECTION('',(0.,0.,1.));
#30329=DIRECTION('center_axis',(0.,0.,1.));
#30330=DIRECTION('ref_axis',(1.,-9.62097198987423E-13,0.));
#30331=DIRECTION('',(0.,0.,1.));
#30332=DIRECTION('center_axis',(0.,0.,1.));
#30333=DIRECTION('ref_axis',(1.,-9.62097198987423E-13,0.));
#30334=DIRECTION('',(0.,0.,1.));
#30335=DIRECTION('center_axis',(0.,0.,1.));
#30336=DIRECTION('ref_axis',(1.,-9.62097198987423E-13,0.));
#30337=DIRECTION('',(0.,0.,1.));
#30338=DIRECTION('center_axis',(0.,0.,1.));
#30339=DIRECTION('ref_axis',(1.,-9.62097198987423E-13,0.));
#30340=DIRECTION('',(0.,0.,1.));
#30341=DIRECTION('center_axis',(0.,0.,1.));
#30342=DIRECTION('ref_axis',(1.,-9.62097198987423E-13,0.));
#30343=DIRECTION('',(0.,0.,1.));
#30344=DIRECTION('center_axis',(0.,0.,1.));
#30345=DIRECTION('ref_axis',(1.,-9.62097198987423E-13,0.));
#30346=DIRECTION('',(0.,0.,1.));
#30347=DIRECTION('center_axis',(0.,0.,1.));
#30348=DIRECTION('ref_axis',(1.,-9.62097198987423E-13,0.));
#30349=DIRECTION('',(0.,0.,1.));
#30350=DIRECTION('center_axis',(0.,0.,1.));
#30351=DIRECTION('ref_axis',(1.,-9.62097198987423E-13,0.));
#30352=DIRECTION('',(0.,0.,1.));
#30353=DIRECTION('center_axis',(0.,0.,1.));
#30354=DIRECTION('ref_axis',(1.,-9.62097198987423E-13,0.));
#30355=DIRECTION('',(0.,0.,1.));
#30356=DIRECTION('center_axis',(0.,0.,1.));
#30357=DIRECTION('ref_axis',(1.,-9.62097198987423E-13,0.));
#30358=DIRECTION('',(0.,0.,1.));
#30359=DIRECTION('center_axis',(0.,0.,1.));
#30360=DIRECTION('ref_axis',(1.,-9.62097198987423E-13,0.));
#30361=DIRECTION('',(0.,0.,1.));
#30362=DIRECTION('center_axis',(0.,0.,1.));
#30363=DIRECTION('ref_axis',(1.,-9.62097198987423E-13,0.));
#30364=DIRECTION('',(0.,0.,1.));
#30365=DIRECTION('center_axis',(0.,0.,1.));
#30366=DIRECTION('ref_axis',(1.,-9.62097198987423E-13,0.));
#30367=DIRECTION('',(0.,0.,1.));
#30368=DIRECTION('center_axis',(0.,0.,1.));
#30369=DIRECTION('ref_axis',(1.,-9.62097198987423E-13,0.));
#30370=DIRECTION('',(0.,0.,1.));
#30371=DIRECTION('center_axis',(0.,0.,1.));
#30372=DIRECTION('ref_axis',(1.,-9.62097198987423E-13,0.));
#30373=DIRECTION('',(0.,0.,1.));
#30374=DIRECTION('center_axis',(0.,0.,1.));
#30375=DIRECTION('ref_axis',(1.,-9.62097198987423E-13,0.));
#30376=DIRECTION('',(0.,0.,1.));
#30377=DIRECTION('center_axis',(0.,0.,1.));
#30378=DIRECTION('ref_axis',(1.,-9.62097198987423E-13,0.));
#30379=DIRECTION('',(0.,0.,1.));
#30380=DIRECTION('center_axis',(0.,0.,1.));
#30381=DIRECTION('ref_axis',(1.,-9.62097198987423E-13,0.));
#30382=DIRECTION('',(0.,0.,1.));
#30383=DIRECTION('center_axis',(0.,0.,1.));
#30384=DIRECTION('ref_axis',(1.,0.,0.));
#30385=DIRECTION('center_axis',(0.,0.,1.));
#30386=DIRECTION('ref_axis',(1.,0.,0.));
#30387=DIRECTION('center_axis',(0.,0.,1.));
#30388=DIRECTION('ref_axis',(1.,0.,0.));
#30389=DIRECTION('center_axis',(0.,0.,1.));
#30390=DIRECTION('ref_axis',(1.,0.,0.));
#30391=DIRECTION('center_axis',(0.,0.,-1.));
#30392=DIRECTION('ref_axis',(1.,-9.62097198987423E-13,0.));
#30393=DIRECTION('center_axis',(0.,0.,1.));
#30394=DIRECTION('ref_axis',(-0.710035149338663,0.70416623513459,0.));
#30395=DIRECTION('center_axis',(0.,0.,1.));
#30396=DIRECTION('ref_axis',(0.984807753012208,-0.17364817766693,0.));
#30397=DIRECTION('center_axis',(0.,0.,-1.));
#30398=DIRECTION('ref_axis',(1.,0.,0.));
#30399=DIRECTION('',(-0.996089805327885,-0.0883464754353932,0.));
#30400=DIRECTION('',(0.905801965515954,-0.423701309022563,0.));
#30401=DIRECTION('center_axis',(-0.423701309022563,-0.905801965515954,0.));
#30402=DIRECTION('ref_axis',(0.905801965515954,-0.423701309022563,0.));
#30403=DIRECTION('',(0.,0.,1.));
#30404=DIRECTION('',(0.,0.,1.));
#30405=DIRECTION('center_axis',(-0.0883464754353932,0.996089805327885,0.));
#30406=DIRECTION('ref_axis',(-0.996089805327885,-0.0883464754353932,0.));
#30407=DIRECTION('',(0.,0.,-1.));
#30408=DIRECTION('center_axis',(0.,0.,1.));
#30409=DIRECTION('ref_axis',(0.939692620785908,-0.342020143325669,0.));
#30410=DIRECTION('center_axis',(0.,0.,-1.));
#30411=DIRECTION('ref_axis',(1.,0.,0.));
#30412=DIRECTION('',(-0.996298167445974,0.0859648855277176,0.));
#30413=DIRECTION('',(0.818465838146947,-0.574555194725812,0.));
#30414=DIRECTION('center_axis',(-0.574555194725812,-0.818465838146947,0.));
#30415=DIRECTION('ref_axis',(0.818465838146947,-0.574555194725812,0.));
#30416=DIRECTION('',(0.,0.,1.));
#30417=DIRECTION('',(0.,0.,1.));
#30418=DIRECTION('center_axis',(0.0859648855277176,0.996298167445974,0.));
#30419=DIRECTION('ref_axis',(-0.996298167445974,0.0859648855277176,0.));
#30420=DIRECTION('',(0.,0.,-1.));
#30421=DIRECTION('center_axis',(0.,0.,1.));
#30422=DIRECTION('ref_axis',(0.866025403784438,-0.5,0.));
#30423=DIRECTION('center_axis',(0.,0.,-1.));
#30424=DIRECTION('ref_axis',(1.,0.,0.));
#30425=DIRECTION('',(-0.966234513897416,0.257664246944399,0.));
#30426=DIRECTION('',(0.706261040449543,-0.707951511576272,0.));
#30427=DIRECTION('center_axis',(-0.707951511576272,-0.706261040449543,0.));
#30428=DIRECTION('ref_axis',(0.706261040449543,-0.707951511576272,0.));
#30429=DIRECTION('',(0.,0.,1.));
#30430=DIRECTION('',(0.,0.,1.));
#30431=DIRECTION('center_axis',(0.257664246944399,0.966234513897416,0.));
#30432=DIRECTION('ref_axis',(-0.966234513897416,0.257664246944399,0.));
#30433=DIRECTION('',(0.,0.,-1.));
#30434=DIRECTION('center_axis',(0.,0.,1.));
#30435=DIRECTION('ref_axis',(0.766044443118978,-0.64278760968654,0.));
#30436=DIRECTION('center_axis',(0.,0.,-1.));
#30437=DIRECTION('ref_axis',(1.,0.,0.));
#30438=DIRECTION('',(-0.906812313582341,0.421534610602074,0.));
#30439=DIRECTION('',(0.572596858423411,-0.819837079988238,0.));
#30440=DIRECTION('center_axis',(-0.819837079988238,-0.572596858423411,0.));
#30441=DIRECTION('ref_axis',(0.572596858423411,-0.819837079988238,0.));
#30442=DIRECTION('',(0.,0.,1.));
#30443=DIRECTION('',(0.,0.,1.));
#30444=DIRECTION('center_axis',(0.421534610602074,0.906812313582341,0.));
#30445=DIRECTION('ref_axis',(-0.906812313582341,0.421534610602074,0.));
#30446=DIRECTION('',(0.,0.,-1.));
#30447=DIRECTION('center_axis',(0.,0.,1.));
#30448=DIRECTION('ref_axis',(0.642787609686539,-0.766044443118978,0.));
#30449=DIRECTION('center_axis',(0.,0.,-1.));
#30450=DIRECTION('ref_axis',(1.,0.,0.));
#30451=DIRECTION('',(-0.819837079988238,0.572596858423411,0.));
#30452=DIRECTION('',(0.421534610602074,-0.906812313582341,0.));
#30453=DIRECTION('center_axis',(-0.906812313582341,-0.421534610602074,0.));
#30454=DIRECTION('ref_axis',(0.421534610602074,-0.906812313582341,0.));
#30455=DIRECTION('',(0.,0.,1.));
#30456=DIRECTION('',(0.,0.,1.));
#30457=DIRECTION('center_axis',(0.572596858423411,0.819837079988238,0.));
#30458=DIRECTION('ref_axis',(-0.819837079988238,0.572596858423411,0.));
#30459=DIRECTION('',(0.,0.,-1.));
#30460=DIRECTION('center_axis',(0.,0.,1.));
#30461=DIRECTION('ref_axis',(0.5,-0.866025403784438,0.));
#30462=DIRECTION('center_axis',(0.,0.,-1.));
#30463=DIRECTION('ref_axis',(1.,0.,0.));
#30464=DIRECTION('',(-0.707951511576272,0.706261040449544,0.));
#30465=DIRECTION('',(0.257664246944398,-0.966234513897416,0.));
#30466=DIRECTION('center_axis',(-0.966234513897416,-0.257664246944398,0.));
#30467=DIRECTION('ref_axis',(0.257664246944398,-0.966234513897416,0.));
#30468=DIRECTION('',(0.,0.,1.));
#30469=DIRECTION('',(0.,0.,1.));
#30470=DIRECTION('center_axis',(0.706261040449544,0.707951511576272,0.));
#30471=DIRECTION('ref_axis',(-0.707951511576272,0.706261040449544,0.));
#30472=DIRECTION('',(0.,0.,-1.));
#30473=DIRECTION('center_axis',(0.,0.,1.));
#30474=DIRECTION('ref_axis',(0.342020143325668,-0.939692620785909,0.));
#30475=DIRECTION('center_axis',(0.,0.,-1.));
#30476=DIRECTION('ref_axis',(1.,0.,0.));
#30477=DIRECTION('',(-0.57455519472581,0.818465838146948,0.));
#30478=DIRECTION('',(0.0859648855277162,-0.996298167445974,0.));
#30479=DIRECTION('center_axis',(-0.996298167445974,-0.0859648855277162,
0.));
#30480=DIRECTION('ref_axis',(0.0859648855277162,-0.996298167445974,0.));
#30481=DIRECTION('',(0.,0.,1.));
#30482=DIRECTION('',(0.,0.,1.));
#30483=DIRECTION('center_axis',(0.818465838146948,0.57455519472581,0.));
#30484=DIRECTION('ref_axis',(-0.57455519472581,0.818465838146948,0.));
#30485=DIRECTION('',(0.,0.,-1.));
#30486=DIRECTION('center_axis',(0.,0.,1.));
#30487=DIRECTION('ref_axis',(0.17364817766693,-0.984807753012208,0.));
#30488=DIRECTION('center_axis',(0.,0.,-1.));
#30489=DIRECTION('ref_axis',(1.,0.,0.));
#30490=DIRECTION('',(-0.423701309022563,0.905801965515955,0.));
#30491=DIRECTION('',(-0.0883464754353936,-0.996089805327885,0.));
#30492=DIRECTION('center_axis',(-0.996089805327885,0.0883464754353937,0.));
#30493=DIRECTION('ref_axis',(-0.0883464754353937,-0.996089805327885,0.));
#30494=DIRECTION('',(0.,0.,1.));
#30495=DIRECTION('',(0.,0.,1.));
#30496=DIRECTION('center_axis',(0.905801965515955,0.423701309022563,0.));
#30497=DIRECTION('ref_axis',(-0.423701309022563,0.905801965515955,0.));
#30498=DIRECTION('',(0.,0.,-1.));
#30499=DIRECTION('center_axis',(0.,0.,1.));
#30500=DIRECTION('ref_axis',(-1.94289029309402E-16,-1.,0.));
#30501=DIRECTION('center_axis',(0.,0.,-1.));
#30502=DIRECTION('ref_axis',(1.,0.,0.));
#30503=DIRECTION('',(-0.259973473447872,0.96561575852067,0.));
#30504=DIRECTION('',(-0.259973473447873,-0.96561575852067,0.));
#30505=DIRECTION('center_axis',(-0.96561575852067,0.259973473447873,0.));
#30506=DIRECTION('ref_axis',(-0.259973473447873,-0.96561575852067,0.));
#30507=DIRECTION('',(0.,0.,1.));
#30508=DIRECTION('',(0.,0.,1.));
#30509=DIRECTION('center_axis',(0.96561575852067,0.259973473447872,0.));
#30510=DIRECTION('ref_axis',(-0.259973473447872,0.96561575852067,0.));
#30511=DIRECTION('',(0.,0.,-1.));
#30512=DIRECTION('center_axis',(0.,0.,1.));
#30513=DIRECTION('ref_axis',(-0.17364817766693,-0.984807753012208,0.));
#30514=DIRECTION('center_axis',(0.,0.,-1.));
#30515=DIRECTION('ref_axis',(1.,0.,0.));
#30516=DIRECTION('',(-0.0883464754353933,0.996089805327885,0.));
#30517=DIRECTION('',(-0.423701309022563,-0.905801965515955,0.));
#30518=DIRECTION('center_axis',(-0.905801965515955,0.423701309022563,0.));
#30519=DIRECTION('ref_axis',(-0.423701309022563,-0.905801965515955,0.));
#30520=DIRECTION('',(0.,0.,1.));
#30521=DIRECTION('',(0.,0.,1.));
#30522=DIRECTION('center_axis',(0.996089805327885,0.0883464754353932,0.));
#30523=DIRECTION('ref_axis',(-0.0883464754353932,0.996089805327885,0.));
#30524=DIRECTION('',(0.,0.,-1.));
#30525=DIRECTION('center_axis',(0.,0.,1.));
#30526=DIRECTION('ref_axis',(-0.342020143325669,-0.939692620785908,0.));
#30527=DIRECTION('center_axis',(0.,0.,-1.));
#30528=DIRECTION('ref_axis',(1.,0.,0.));
#30529=DIRECTION('',(0.0859648855277175,0.996298167445974,0.));
#30530=DIRECTION('',(-0.574555194725811,-0.818465838146947,0.));
#30531=DIRECTION('center_axis',(-0.818465838146947,0.574555194725811,0.));
#30532=DIRECTION('ref_axis',(-0.574555194725811,-0.818465838146947,0.));
#30533=DIRECTION('',(0.,0.,1.));
#30534=DIRECTION('',(0.,0.,1.));
#30535=DIRECTION('center_axis',(0.996298167445974,-0.0859648855277175,0.));
#30536=DIRECTION('ref_axis',(0.0859648855277175,0.996298167445974,0.));
#30537=DIRECTION('',(0.,0.,-1.));
#30538=DIRECTION('center_axis',(0.,0.,1.));
#30539=DIRECTION('ref_axis',(-0.5,-0.866025403784438,0.));
#30540=DIRECTION('center_axis',(0.,0.,-1.));
#30541=DIRECTION('ref_axis',(1.,0.,0.));
#30542=DIRECTION('',(0.257664246944399,0.966234513897416,0.));
#30543=DIRECTION('',(-0.707951511576272,-0.706261040449543,0.));
#30544=DIRECTION('center_axis',(-0.706261040449543,0.707951511576272,0.));
#30545=DIRECTION('ref_axis',(-0.707951511576272,-0.706261040449543,0.));
#30546=DIRECTION('',(0.,0.,1.));
#30547=DIRECTION('',(0.,0.,1.));
#30548=DIRECTION('center_axis',(0.966234513897416,-0.257664246944399,0.));
#30549=DIRECTION('ref_axis',(0.257664246944399,0.966234513897416,0.));
#30550=DIRECTION('',(0.,0.,-1.));
#30551=DIRECTION('center_axis',(0.,0.,1.));
#30552=DIRECTION('ref_axis',(-0.642787609686539,-0.766044443118978,0.));
#30553=DIRECTION('center_axis',(0.,0.,-1.));
#30554=DIRECTION('ref_axis',(1.,0.,0.));
#30555=DIRECTION('',(0.421534610602074,0.906812313582341,0.));
#30556=DIRECTION('',(-0.819837079988238,-0.572596858423411,0.));
#30557=DIRECTION('center_axis',(-0.572596858423411,0.819837079988238,0.));
#30558=DIRECTION('ref_axis',(-0.819837079988238,-0.572596858423411,0.));
#30559=DIRECTION('',(0.,0.,1.));
#30560=DIRECTION('',(0.,0.,1.));
#30561=DIRECTION('center_axis',(0.906812313582341,-0.421534610602074,0.));
#30562=DIRECTION('ref_axis',(0.421534610602074,0.906812313582341,0.));
#30563=DIRECTION('',(0.,0.,-1.));
#30564=DIRECTION('center_axis',(0.,0.,1.));
#30565=DIRECTION('ref_axis',(-0.766044443118978,-0.642787609686539,0.));
#30566=DIRECTION('center_axis',(0.,0.,-1.));
#30567=DIRECTION('ref_axis',(1.,0.,0.));
#30568=DIRECTION('',(0.572596858423411,0.819837079988238,0.));
#30569=DIRECTION('',(-0.906812313582341,-0.421534610602074,0.));
#30570=DIRECTION('center_axis',(-0.421534610602074,0.906812313582341,0.));
#30571=DIRECTION('ref_axis',(-0.906812313582341,-0.421534610602074,0.));
#30572=DIRECTION('',(0.,0.,1.));
#30573=DIRECTION('',(0.,0.,1.));
#30574=DIRECTION('center_axis',(0.819837079988238,-0.572596858423411,0.));
#30575=DIRECTION('ref_axis',(0.572596858423411,0.819837079988238,0.));
#30576=DIRECTION('',(0.,0.,-1.));
#30577=DIRECTION('center_axis',(0.,0.,1.));
#30578=DIRECTION('ref_axis',(-0.866025403784439,-0.5,0.));
#30579=DIRECTION('center_axis',(0.,0.,-1.));
#30580=DIRECTION('ref_axis',(1.,0.,0.));
#30581=DIRECTION('',(0.706261040449544,0.707951511576271,0.));
#30582=DIRECTION('',(-0.966234513897416,-0.257664246944398,0.));
#30583=DIRECTION('center_axis',(-0.257664246944398,0.966234513897416,0.));
#30584=DIRECTION('ref_axis',(-0.966234513897416,-0.257664246944398,0.));
#30585=DIRECTION('',(0.,0.,1.));
#30586=DIRECTION('',(0.,0.,1.));
#30587=DIRECTION('center_axis',(0.707951511576271,-0.706261040449544,0.));
#30588=DIRECTION('ref_axis',(0.706261040449544,0.707951511576271,0.));
#30589=DIRECTION('',(0.,0.,-1.));
#30590=DIRECTION('center_axis',(0.,0.,1.));
#30591=DIRECTION('ref_axis',(-0.939692620785909,-0.342020143325669,0.));
#30592=DIRECTION('center_axis',(0.,0.,-1.));
#30593=DIRECTION('ref_axis',(1.,0.,0.));
#30594=DIRECTION('',(0.818465838146948,0.574555194725811,0.));
#30595=DIRECTION('',(-0.996298167445974,-0.0859648855277167,0.));
#30596=DIRECTION('center_axis',(-0.0859648855277167,0.996298167445974,0.));
#30597=DIRECTION('ref_axis',(-0.996298167445974,-0.0859648855277167,0.));
#30598=DIRECTION('',(0.,0.,1.));
#30599=DIRECTION('',(0.,0.,1.));
#30600=DIRECTION('center_axis',(0.574555194725811,-0.818465838146948,0.));
#30601=DIRECTION('ref_axis',(0.818465838146948,0.574555194725811,0.));
#30602=DIRECTION('',(0.,0.,-1.));
#30603=DIRECTION('center_axis',(0.,0.,1.));
#30604=DIRECTION('ref_axis',(-0.984807753012208,-0.17364817766693,0.));
#30605=DIRECTION('center_axis',(0.,0.,-1.));
#30606=DIRECTION('ref_axis',(1.,0.,0.));
#30607=DIRECTION('',(0.905801965515955,0.423701309022563,0.));
#30608=DIRECTION('',(-0.996089805327885,0.0883464754353936,0.));
#30609=DIRECTION('center_axis',(0.0883464754353936,0.996089805327885,0.));
#30610=DIRECTION('ref_axis',(-0.996089805327885,0.0883464754353936,0.));
#30611=DIRECTION('',(0.,0.,1.));
#30612=DIRECTION('',(0.,0.,1.));
#30613=DIRECTION('center_axis',(0.423701309022563,-0.905801965515955,0.));
#30614=DIRECTION('ref_axis',(0.905801965515955,0.423701309022563,0.));
#30615=DIRECTION('',(0.,0.,-1.));
#30616=DIRECTION('center_axis',(0.,0.,1.));
#30617=DIRECTION('ref_axis',(-1.,1.11022302462516E-16,0.));
#30618=DIRECTION('center_axis',(0.,0.,-1.));
#30619=DIRECTION('ref_axis',(1.,0.,0.));
#30620=DIRECTION('',(0.96561575852067,0.259973473447872,0.));
#30621=DIRECTION('',(-0.96561575852067,0.259973473447873,0.));
#30622=DIRECTION('center_axis',(0.,0.,-1.));
#30623=DIRECTION('ref_axis',(1.,0.,0.));
#30624=DIRECTION('center_axis',(0.259973473447873,0.96561575852067,0.));
#30625=DIRECTION('ref_axis',(-0.96561575852067,0.259973473447873,0.));
#30626=DIRECTION('',(0.,0.,1.));
#30627=DIRECTION('',(0.,0.,1.));
#30628=DIRECTION('center_axis',(0.259973473447872,-0.96561575852067,0.));
#30629=DIRECTION('ref_axis',(0.96561575852067,0.259973473447872,0.));
#30630=DIRECTION('',(0.,0.,-1.));
#30631=DIRECTION('center_axis',(0.,0.,1.));
#30632=DIRECTION('ref_axis',(-0.984807753012208,0.173648177666931,0.));
#30633=DIRECTION('center_axis',(0.,0.,-1.));
#30634=DIRECTION('ref_axis',(1.,0.,0.));
#30635=DIRECTION('',(0.996089805327885,0.0883464754353928,0.));
#30636=DIRECTION('',(-0.905801965515954,0.423701309022564,0.));
#30637=DIRECTION('center_axis',(0.423701309022564,0.905801965515954,0.));
#30638=DIRECTION('ref_axis',(-0.905801965515954,0.423701309022564,0.));
#30639=DIRECTION('',(0.,0.,1.));
#30640=DIRECTION('',(0.,0.,1.));
#30641=DIRECTION('center_axis',(0.0883464754353928,-0.996089805327885,0.));
#30642=DIRECTION('ref_axis',(0.996089805327885,0.0883464754353928,0.));
#30643=DIRECTION('',(0.,0.,-1.));
#30644=DIRECTION('center_axis',(0.,0.,1.));
#30645=DIRECTION('ref_axis',(-0.939692620785908,0.342020143325669,0.));
#30646=DIRECTION('center_axis',(0.,0.,-1.));
#30647=DIRECTION('ref_axis',(1.,0.,0.));
#30648=DIRECTION('',(0.996298167445974,-0.085964885527717,0.));
#30649=DIRECTION('',(-0.818465838146948,0.574555194725811,0.));
#30650=DIRECTION('center_axis',(0.574555194725811,0.818465838146948,0.));
#30651=DIRECTION('ref_axis',(-0.818465838146948,0.574555194725811,0.));
#30652=DIRECTION('',(0.,0.,1.));
#30653=DIRECTION('',(0.,0.,1.));
#30654=DIRECTION('center_axis',(-0.085964885527717,-0.996298167445974,0.));
#30655=DIRECTION('ref_axis',(0.996298167445974,-0.085964885527717,0.));
#30656=DIRECTION('',(0.,0.,-1.));
#30657=DIRECTION('center_axis',(0.,0.,1.));
#30658=DIRECTION('ref_axis',(-0.866025403784439,0.5,0.));
#30659=DIRECTION('center_axis',(0.,0.,-1.));
#30660=DIRECTION('ref_axis',(1.,0.,0.));
#30661=DIRECTION('',(0.966234513897416,-0.257664246944398,0.));
#30662=DIRECTION('',(-0.706261040449544,0.707951511576272,0.));
#30663=DIRECTION('center_axis',(0.707951511576272,0.706261040449544,0.));
#30664=DIRECTION('ref_axis',(-0.706261040449544,0.707951511576272,0.));
#30665=DIRECTION('',(0.,0.,1.));
#30666=DIRECTION('',(0.,0.,1.));
#30667=DIRECTION('center_axis',(-0.257664246944398,-0.966234513897416,0.));
#30668=DIRECTION('ref_axis',(0.966234513897416,-0.257664246944398,0.));
#30669=DIRECTION('',(0.,0.,-1.));
#30670=DIRECTION('center_axis',(0.,0.,1.));
#30671=DIRECTION('ref_axis',(-0.766044443118978,0.642787609686539,0.));
#30672=DIRECTION('center_axis',(0.,0.,-1.));
#30673=DIRECTION('ref_axis',(1.,0.,0.));
#30674=DIRECTION('',(0.906812313582341,-0.421534610602074,0.));
#30675=DIRECTION('',(-0.572596858423411,0.819837079988238,0.));
#30676=DIRECTION('center_axis',(0.819837079988238,0.572596858423411,0.));
#30677=DIRECTION('ref_axis',(-0.572596858423411,0.819837079988238,0.));
#30678=DIRECTION('',(0.,0.,1.));
#30679=DIRECTION('',(0.,0.,1.));
#30680=DIRECTION('center_axis',(-0.421534610602074,-0.906812313582341,0.));
#30681=DIRECTION('ref_axis',(0.906812313582341,-0.421534610602074,0.));
#30682=DIRECTION('',(0.,0.,-1.));
#30683=DIRECTION('center_axis',(0.,0.,1.));
#30684=DIRECTION('ref_axis',(-0.642787609686539,0.766044443118978,0.));
#30685=DIRECTION('center_axis',(0.,0.,-1.));
#30686=DIRECTION('ref_axis',(1.,0.,0.));
#30687=DIRECTION('',(0.819837079988238,-0.572596858423411,0.));
#30688=DIRECTION('',(-0.421534610602074,0.906812313582341,0.));
#30689=DIRECTION('center_axis',(0.906812313582341,0.421534610602074,0.));
#30690=DIRECTION('ref_axis',(-0.421534610602074,0.906812313582341,0.));
#30691=DIRECTION('',(0.,0.,1.));
#30692=DIRECTION('',(0.,0.,1.));
#30693=DIRECTION('center_axis',(-0.572596858423411,-0.819837079988238,0.));
#30694=DIRECTION('ref_axis',(0.819837079988238,-0.572596858423411,0.));
#30695=DIRECTION('',(0.,0.,-1.));
#30696=DIRECTION('center_axis',(0.,0.,1.));
#30697=DIRECTION('ref_axis',(-0.5,0.866025403784439,0.));
#30698=DIRECTION('center_axis',(0.,0.,-1.));
#30699=DIRECTION('ref_axis',(1.,0.,0.));
#30700=DIRECTION('',(0.707951511576272,-0.706261040449544,0.));
#30701=DIRECTION('',(-0.257664246944398,0.966234513897416,0.));
#30702=DIRECTION('center_axis',(0.966234513897416,0.257664246944398,0.));
#30703=DIRECTION('ref_axis',(-0.257664246944398,0.966234513897416,0.));
#30704=DIRECTION('',(0.,0.,1.));
#30705=DIRECTION('',(0.,0.,1.));
#30706=DIRECTION('center_axis',(-0.706261040449544,-0.707951511576272,0.));
#30707=DIRECTION('ref_axis',(0.707951511576272,-0.706261040449544,0.));
#30708=DIRECTION('',(0.,0.,-1.));
#30709=DIRECTION('center_axis',(0.,0.,1.));
#30710=DIRECTION('ref_axis',(-0.342020143325669,0.939692620785909,0.));
#30711=DIRECTION('center_axis',(0.,0.,-1.));
#30712=DIRECTION('ref_axis',(1.,0.,0.));
#30713=DIRECTION('',(0.574555194725811,-0.818465838146948,0.));
#30714=DIRECTION('',(-0.0859648855277167,0.996298167445974,0.));
#30715=DIRECTION('center_axis',(0.996298167445974,0.0859648855277167,0.));
#30716=DIRECTION('ref_axis',(-0.0859648855277167,0.996298167445974,0.));
#30717=DIRECTION('',(0.,0.,1.));
#30718=DIRECTION('',(0.,0.,1.));
#30719=DIRECTION('center_axis',(-0.818465838146948,-0.574555194725811,0.));
#30720=DIRECTION('ref_axis',(0.574555194725811,-0.818465838146948,0.));
#30721=DIRECTION('',(0.,0.,-1.));
#30722=DIRECTION('center_axis',(0.,0.,1.));
#30723=DIRECTION('ref_axis',(-0.17364817766693,0.984807753012208,0.));
#30724=DIRECTION('center_axis',(0.,0.,-1.));
#30725=DIRECTION('ref_axis',(1.,0.,0.));
#30726=DIRECTION('',(0.423701309022563,-0.905801965515955,0.));
#30727=DIRECTION('',(0.0883464754353932,0.996089805327885,0.));
#30728=DIRECTION('center_axis',(0.996089805327885,-0.0883464754353932,0.));
#30729=DIRECTION('ref_axis',(0.0883464754353932,0.996089805327885,0.));
#30730=DIRECTION('',(0.,0.,1.));
#30731=DIRECTION('',(0.,0.,1.));
#30732=DIRECTION('center_axis',(-0.905801965515955,-0.423701309022563,0.));
#30733=DIRECTION('ref_axis',(0.423701309022563,-0.905801965515955,0.));
#30734=DIRECTION('',(0.,0.,-1.));
#30735=DIRECTION('center_axis',(0.,0.,1.));
#30736=DIRECTION('ref_axis',(5.55111512312578E-17,1.,0.));
#30737=DIRECTION('center_axis',(0.,0.,-1.));
#30738=DIRECTION('ref_axis',(1.,0.,0.));
#30739=DIRECTION('',(0.259973473447872,-0.96561575852067,0.));
#30740=DIRECTION('',(0.259973473447872,0.96561575852067,0.));
#30741=DIRECTION('center_axis',(0.96561575852067,-0.259973473447873,0.));
#30742=DIRECTION('ref_axis',(0.259973473447873,0.96561575852067,0.));
#30743=DIRECTION('',(0.,0.,1.));
#30744=DIRECTION('',(0.,0.,1.));
#30745=DIRECTION('center_axis',(-0.96561575852067,-0.259973473447872,0.));
#30746=DIRECTION('ref_axis',(0.259973473447872,-0.96561575852067,0.));
#30747=DIRECTION('',(0.,0.,-1.));
#30748=DIRECTION('center_axis',(0.,0.,1.));
#30749=DIRECTION('ref_axis',(0.17364817766693,0.984807753012208,0.));
#30750=DIRECTION('center_axis',(0.,0.,-1.));
#30751=DIRECTION('ref_axis',(1.,0.,0.));
#30752=DIRECTION('',(0.0883464754353931,-0.996089805327885,0.));
#30753=DIRECTION('',(0.423701309022563,0.905801965515954,0.));
#30754=DIRECTION('center_axis',(0.905801965515954,-0.423701309022563,0.));
#30755=DIRECTION('ref_axis',(0.423701309022563,0.905801965515954,0.));
#30756=DIRECTION('',(0.,0.,1.));
#30757=DIRECTION('',(0.,0.,1.));
#30758=DIRECTION('center_axis',(-0.996089805327885,-0.0883464754353932,
0.));
#30759=DIRECTION('ref_axis',(0.0883464754353932,-0.996089805327885,0.));
#30760=DIRECTION('',(0.,0.,-1.));
#30761=DIRECTION('center_axis',(0.,0.,1.));
#30762=DIRECTION('ref_axis',(0.342020143325669,0.939692620785908,0.));
#30763=DIRECTION('center_axis',(0.,0.,-1.));
#30764=DIRECTION('ref_axis',(1.,0.,0.));
#30765=DIRECTION('',(-0.085964885527717,-0.996298167445974,0.));
#30766=DIRECTION('',(0.574555194725811,0.818465838146948,0.));
#30767=DIRECTION('center_axis',(0.818465838146948,-0.574555194725811,0.));
#30768=DIRECTION('ref_axis',(0.574555194725811,0.818465838146948,0.));
#30769=DIRECTION('',(0.,0.,1.));
#30770=DIRECTION('',(0.,0.,1.));
#30771=DIRECTION('center_axis',(-0.996298167445974,0.085964885527717,0.));
#30772=DIRECTION('ref_axis',(-0.085964885527717,-0.996298167445974,0.));
#30773=DIRECTION('',(0.,0.,-1.));
#30774=DIRECTION('center_axis',(0.,0.,1.));
#30775=DIRECTION('ref_axis',(0.5,0.866025403784439,0.));
#30776=DIRECTION('center_axis',(0.,0.,-1.));
#30777=DIRECTION('ref_axis',(1.,0.,0.));
#30778=DIRECTION('',(-0.257664246944398,-0.966234513897416,0.));
#30779=DIRECTION('',(0.707951511576272,0.706261040449544,0.));
#30780=DIRECTION('center_axis',(0.706261040449544,-0.707951511576272,0.));
#30781=DIRECTION('ref_axis',(0.707951511576272,0.706261040449544,0.));
#30782=DIRECTION('',(0.,0.,1.));
#30783=DIRECTION('',(0.,0.,1.));
#30784=DIRECTION('center_axis',(-0.966234513897416,0.257664246944398,0.));
#30785=DIRECTION('ref_axis',(-0.257664246944398,-0.966234513897416,0.));
#30786=DIRECTION('',(0.,0.,-1.));
#30787=DIRECTION('center_axis',(0.,0.,1.));
#30788=DIRECTION('ref_axis',(0.642787609686539,0.766044443118978,0.));
#30789=DIRECTION('center_axis',(0.,0.,-1.));
#30790=DIRECTION('ref_axis',(1.,0.,0.));
#30791=DIRECTION('',(-0.421534610602074,-0.906812313582341,0.));
#30792=DIRECTION('',(0.819837079988238,0.572596858423411,0.));
#30793=DIRECTION('center_axis',(0.572596858423411,-0.819837079988238,0.));
#30794=DIRECTION('ref_axis',(0.819837079988238,0.572596858423411,0.));
#30795=DIRECTION('',(0.,0.,1.));
#30796=DIRECTION('',(0.,0.,1.));
#30797=DIRECTION('center_axis',(-0.906812313582341,0.421534610602074,0.));
#30798=DIRECTION('ref_axis',(-0.421534610602074,-0.906812313582341,0.));
#30799=DIRECTION('',(0.,0.,-1.));
#30800=DIRECTION('center_axis',(0.,0.,1.));
#30801=DIRECTION('ref_axis',(0.766044443118978,0.642787609686539,0.));
#30802=DIRECTION('center_axis',(0.,0.,-1.));
#30803=DIRECTION('ref_axis',(1.,0.,0.));
#30804=DIRECTION('',(-0.572596858423411,-0.819837079988238,0.));
#30805=DIRECTION('',(0.906812313582341,0.421534610602074,0.));
#30806=DIRECTION('center_axis',(0.421534610602074,-0.906812313582341,0.));
#30807=DIRECTION('ref_axis',(0.906812313582341,0.421534610602074,0.));
#30808=DIRECTION('',(0.,0.,1.));
#30809=DIRECTION('',(0.,0.,1.));
#30810=DIRECTION('center_axis',(-0.819837079988238,0.572596858423411,0.));
#30811=DIRECTION('ref_axis',(-0.572596858423411,-0.819837079988238,0.));
#30812=DIRECTION('',(0.,0.,-1.));
#30813=DIRECTION('center_axis',(0.,0.,1.));
#30814=DIRECTION('ref_axis',(0.866025403784439,0.5,0.));
#30815=DIRECTION('center_axis',(0.,0.,-1.));
#30816=DIRECTION('ref_axis',(1.,0.,0.));
#30817=DIRECTION('',(-0.706261040449544,-0.707951511576272,0.));
#30818=DIRECTION('',(0.966234513897416,0.257664246944398,0.));
#30819=DIRECTION('center_axis',(0.257664246944398,-0.966234513897416,0.));
#30820=DIRECTION('ref_axis',(0.966234513897416,0.257664246944398,0.));
#30821=DIRECTION('',(0.,0.,1.));
#30822=DIRECTION('',(0.,0.,1.));
#30823=DIRECTION('center_axis',(-0.707951511576272,0.706261040449544,0.));
#30824=DIRECTION('ref_axis',(-0.706261040449544,-0.707951511576272,0.));
#30825=DIRECTION('',(0.,0.,-1.));
#30826=DIRECTION('center_axis',(0.,0.,1.));
#30827=DIRECTION('ref_axis',(0.939692620785909,0.342020143325669,0.));
#30828=DIRECTION('center_axis',(0.,0.,-1.));
#30829=DIRECTION('ref_axis',(1.,0.,0.));
#30830=DIRECTION('',(-0.818465838146948,-0.574555194725811,0.));
#30831=DIRECTION('',(0.996298167445974,0.0859648855277167,0.));
#30832=DIRECTION('center_axis',(0.0859648855277167,-0.996298167445974,0.));
#30833=DIRECTION('ref_axis',(0.996298167445974,0.0859648855277167,0.));
#30834=DIRECTION('',(0.,0.,1.));
#30835=DIRECTION('',(0.,0.,1.));
#30836=DIRECTION('center_axis',(-0.574555194725811,0.818465838146948,0.));
#30837=DIRECTION('ref_axis',(-0.818465838146948,-0.574555194725811,0.));
#30838=DIRECTION('',(0.,0.,-1.));
#30839=DIRECTION('center_axis',(0.,0.,1.));
#30840=DIRECTION('ref_axis',(0.984807753012208,0.17364817766693,0.));
#30841=DIRECTION('center_axis',(0.,0.,-1.));
#30842=DIRECTION('ref_axis',(1.,0.,0.));
#30843=DIRECTION('',(-0.905801965515955,-0.423701309022563,0.));
#30844=DIRECTION('',(0.996089805327885,-0.0883464754353932,0.));
#30845=DIRECTION('center_axis',(-0.0883464754353933,-0.996089805327885,
0.));
#30846=DIRECTION('ref_axis',(0.996089805327885,-0.0883464754353933,0.));
#30847=DIRECTION('',(0.,0.,1.));
#30848=DIRECTION('',(0.,0.,1.));
#30849=DIRECTION('center_axis',(-0.423701309022563,0.905801965515955,0.));
#30850=DIRECTION('ref_axis',(-0.905801965515954,-0.423701309022563,0.));
#30851=DIRECTION('',(0.,0.,-1.));
#30852=DIRECTION('center_axis',(0.,0.,1.));
#30853=DIRECTION('ref_axis',(1.,0.,0.));
#30854=DIRECTION('center_axis',(0.,0.,1.));
#30855=DIRECTION('ref_axis',(1.,0.,0.));
#30856=DIRECTION('center_axis',(0.,0.,1.));
#30857=DIRECTION('ref_axis',(1.,0.,0.));
#30858=DIRECTION('center_axis',(0.,0.,1.));
#30859=DIRECTION('ref_axis',(1.,0.,0.));
#30860=DIRECTION('center_axis',(0.,0.,1.));
#30861=DIRECTION('ref_axis',(1.,0.,0.));
#30862=DIRECTION('center_axis',(0.,0.,1.));
#30863=DIRECTION('ref_axis',(1.,0.,0.));
#30864=DIRECTION('center_axis',(0.,0.,1.));
#30865=DIRECTION('ref_axis',(1.,0.,0.));
#30866=DIRECTION('center_axis',(0.,0.,1.));
#30867=DIRECTION('ref_axis',(1.,0.,0.));
#30868=DIRECTION('center_axis',(0.,0.,1.));
#30869=DIRECTION('ref_axis',(1.,0.,0.));
#30870=DIRECTION('center_axis',(0.,0.,1.));
#30871=DIRECTION('ref_axis',(1.,0.,0.));
#30872=DIRECTION('center_axis',(0.,0.,1.));
#30873=DIRECTION('ref_axis',(1.,0.,0.));
#30874=DIRECTION('center_axis',(0.,0.,1.));
#30875=DIRECTION('ref_axis',(1.,0.,0.));
#30876=DIRECTION('center_axis',(0.,0.,1.));
#30877=DIRECTION('ref_axis',(1.,0.,0.));
#30878=DIRECTION('center_axis',(0.,0.,1.));
#30879=DIRECTION('ref_axis',(1.,0.,0.));
#30880=DIRECTION('center_axis',(0.,0.,1.));
#30881=DIRECTION('ref_axis',(1.,0.,0.));
#30882=DIRECTION('center_axis',(0.,0.,1.));
#30883=DIRECTION('ref_axis',(1.,0.,0.));
#30884=DIRECTION('center_axis',(0.,0.,1.));
#30885=DIRECTION('ref_axis',(1.,0.,0.));
#30886=DIRECTION('center_axis',(0.,0.,1.));
#30887=DIRECTION('ref_axis',(1.,0.,0.));
#30888=DIRECTION('',(0.,0.,-1.));
#30889=DIRECTION('center_axis',(0.,0.,1.));
#30890=DIRECTION('ref_axis',(1.,0.,0.));
#30891=DIRECTION('center_axis',(0.,0.,1.));
#30892=DIRECTION('ref_axis',(1.,0.,0.));
#30893=DIRECTION('center_axis',(0.,0.,1.));
#30894=DIRECTION('ref_axis',(1.,0.,0.));
#30895=DIRECTION('center_axis',(0.,0.,1.));
#30896=DIRECTION('ref_axis',(1.,0.,0.));
#30897=DIRECTION('center_axis',(0.,0.,1.));
#30898=DIRECTION('ref_axis',(1.,0.,0.));
#30899=DIRECTION('center_axis',(0.,0.,1.));
#30900=DIRECTION('ref_axis',(1.,0.,0.));
#30901=DIRECTION('center_axis',(0.,0.,1.));
#30902=DIRECTION('ref_axis',(1.,0.,0.));
#30903=DIRECTION('center_axis',(0.,0.,1.));
#30904=DIRECTION('ref_axis',(1.,0.,0.));
#30905=DIRECTION('center_axis',(0.,0.,1.));
#30906=DIRECTION('ref_axis',(1.,0.,0.));
#30907=DIRECTION('center_axis',(0.,0.,1.));
#30908=DIRECTION('ref_axis',(1.,0.,0.));
#30909=DIRECTION('center_axis',(0.,0.,1.));
#30910=DIRECTION('ref_axis',(1.,0.,0.));
#30911=DIRECTION('center_axis',(0.,0.,1.));
#30912=DIRECTION('ref_axis',(1.,0.,0.));
#30913=DIRECTION('center_axis',(0.,0.,1.));
#30914=DIRECTION('ref_axis',(1.,0.,0.));
#30915=DIRECTION('center_axis',(0.,0.,1.));
#30916=DIRECTION('ref_axis',(1.,0.,0.));
#30917=DIRECTION('center_axis',(0.,0.,1.));
#30918=DIRECTION('ref_axis',(1.,0.,0.));
#30919=DIRECTION('center_axis',(0.,0.,1.));
#30920=DIRECTION('ref_axis',(1.,0.,0.));
#30921=DIRECTION('center_axis',(0.,0.,1.));
#30922=DIRECTION('ref_axis',(1.,0.,0.));
#30923=DIRECTION('center_axis',(0.,0.,1.));
#30924=DIRECTION('ref_axis',(1.,0.,0.));
#30925=DIRECTION('center_axis',(0.,0.,1.));
#30926=DIRECTION('ref_axis',(1.,0.,0.));
#30927=DIRECTION('',(0.,0.,-1.));
#30928=DIRECTION('center_axis',(0.,0.,-1.));
#30929=DIRECTION('ref_axis',(1.,0.,0.));
#30930=DIRECTION('',(0.,0.,1.));
#30931=DIRECTION('center_axis',(0.,0.,1.));
#30932=DIRECTION('ref_axis',(1.,0.,0.));
#30933=DIRECTION('center_axis',(-0.259973473447872,-0.96561575852067,0.));
#30934=DIRECTION('ref_axis',(0.96561575852067,-0.259973473447872,0.));
#30935=DIRECTION('',(0.96561575852067,-0.259973473447872,0.));
#30936=DIRECTION('',(0.,0.,1.));
#30937=DIRECTION('center_axis',(-0.259973473447872,0.96561575852067,0.));
#30938=DIRECTION('ref_axis',(-0.96561575852067,-0.259973473447872,0.));
#30939=DIRECTION('',(-0.96561575852067,-0.259973473447872,0.));
#30940=DIRECTION('center_axis',(0.,0.,1.));
#30941=DIRECTION('ref_axis',(1.,0.,0.));
#30942=DIRECTION('center_axis',(0.,0.,-1.));
#30943=DIRECTION('ref_axis',(1.,0.,0.));
#30944=DIRECTION('center_axis',(0.,0.,1.));
#30945=DIRECTION('ref_axis',(1.,0.,0.));
#30946=DIRECTION('',(-0.707106781186549,-8.65956056235495E-17,-0.707106781186546));
#30947=DIRECTION('center_axis',(0.,0.,1.));
#30948=DIRECTION('ref_axis',(1.,0.,0.));
#30949=DIRECTION('',(-0.844694227521705,-1.0344520819927E-16,0.535249158795705));
#30950=DIRECTION('center_axis',(0.,0.,-1.));
#30951=DIRECTION('ref_axis',(1.,0.,0.));
#30952=DIRECTION('center_axis',(0.5,0.866025403784439,0.));
#30953=DIRECTION('ref_axis',(0.866025403784439,-0.5,0.));
#30954=DIRECTION('',(0.866025403784439,-0.5,0.));
#30955=DIRECTION('',(0.,0.,-1.));
#30956=DIRECTION('',(0.866025403784439,-0.5,0.));
#30957=DIRECTION('',(0.,0.,-1.));
#30958=DIRECTION('center_axis',(-0.5,0.866025403784439,0.));
#30959=DIRECTION('ref_axis',(0.866025403784439,0.5,0.));
#30960=DIRECTION('',(0.866025403784439,0.5,0.));
#30961=DIRECTION('',(0.,0.,-1.));
#30962=DIRECTION('',(0.866025403784439,0.5,0.));
#30963=DIRECTION('center_axis',(-1.,-1.92296268638356E-16,0.));
#30964=DIRECTION('ref_axis',(-1.92296268638356E-16,1.,0.));
#30965=DIRECTION('',(-1.92296268638356E-16,1.,0.));
#30966=DIRECTION('',(0.,0.,-1.));
#30967=DIRECTION('',(-1.92296268638356E-16,1.,0.));
#30968=DIRECTION('center_axis',(-0.5,-0.866025403784439,0.));
#30969=DIRECTION('ref_axis',(-0.866025403784439,0.5,0.));
#30970=DIRECTION('',(-0.866025403784439,0.5,0.));
#30971=DIRECTION('',(0.,0.,-1.));
#30972=DIRECTION('',(-0.866025403784439,0.5,0.));
#30973=DIRECTION('center_axis',(0.5,-0.866025403784439,0.));
#30974=DIRECTION('ref_axis',(-0.866025403784439,-0.5,0.));
#30975=DIRECTION('',(-0.866025403784439,-0.5,0.));
#30976=DIRECTION('',(0.,0.,-1.));
#30977=DIRECTION('',(-0.866025403784439,-0.5,0.));
#30978=DIRECTION('center_axis',(1.,-3.84592537276713E-16,0.));
#30979=DIRECTION('ref_axis',(-3.84592537276713E-16,-1.,0.));
#30980=DIRECTION('',(-3.84592537276713E-16,-1.,0.));
#30981=DIRECTION('',(-3.84592537276713E-16,-1.,0.));
#30982=DIRECTION('center_axis',(0.,0.,-1.));
#30983=DIRECTION('ref_axis',(-1.,0.,0.));
#30984=DIRECTION('center_axis',(0.,0.,-1.));
#30985=DIRECTION('ref_axis',(-1.,0.,0.));
#30986=DIRECTION('center_axis',(0.,0.,1.));
#30987=DIRECTION('ref_axis',(1.,0.,0.));
#30988=DIRECTION('center_axis',(0.,0.,1.));
#30989=DIRECTION('ref_axis',(1.,0.,0.));
#30990=DIRECTION('',(0.707106781186547,8.65956056235493E-17,-0.707106781186548));
#30991=DIRECTION('center_axis',(0.,0.,1.));
#30992=DIRECTION('ref_axis',(0.952238475886209,-0.30535534225212,0.));
#30993=DIRECTION('center_axis',(0.,0.,1.));
#30994=DIRECTION('ref_axis',(1.,0.,0.));
#30995=DIRECTION('center_axis',(0.,0.,1.));
#30996=DIRECTION('ref_axis',(1.,0.,0.));
#30997=DIRECTION('center_axis',(0.,0.,1.));
#30998=DIRECTION('ref_axis',(1.,0.,0.));
#30999=DIRECTION('',(0.707106781186548,8.65956056235494E-17,-0.707106781186547));
#31000=DIRECTION('center_axis',(0.,0.,-1.));
#31001=DIRECTION('ref_axis',(-1.,0.,0.));
#31002=DIRECTION('center_axis',(0.,0.,1.));
#31003=DIRECTION('ref_axis',(1.,0.,0.));
#31004=DIRECTION('axis',(0.,0.,1.));
#31005=DIRECTION('refdir',(1.,0.,0.));
#31006=DIRECTION('center_axis',(0.,0.,1.));
#31007=DIRECTION('ref_axis',(1.,0.,0.));
#31008=DIRECTION('',(0.,0.,-1.));
#31009=DIRECTION('center_axis',(0.,0.,-1.));
#31010=DIRECTION('ref_axis',(1.,0.,0.));
#31011=DIRECTION('',(0.,0.,-1.));
#31012=DIRECTION('center_axis',(0.,0.,1.));
#31013=DIRECTION('ref_axis',(1.,0.,0.));
#31014=DIRECTION('center_axis',(0.,0.,-1.));
#31015=DIRECTION('ref_axis',(1.,0.,0.));
#31016=DIRECTION('center_axis',(0.,0.,1.));
#31017=DIRECTION('ref_axis',(1.,0.,0.));
#31018=DIRECTION('',(0.,0.,-1.));
#31019=DIRECTION('center_axis',(0.,0.,1.));
#31020=DIRECTION('ref_axis',(1.,0.,0.));
#31021=DIRECTION('',(0.,0.,-1.));
#31022=DIRECTION('center_axis',(0.,0.,1.));
#31023=DIRECTION('ref_axis',(1.,0.,0.));
#31024=DIRECTION('',(0.,0.,-1.));
#31025=DIRECTION('center_axis',(0.,0.,1.));
#31026=DIRECTION('ref_axis',(1.,0.,0.));
#31027=DIRECTION('',(0.,0.,-1.));
#31028=DIRECTION('center_axis',(0.,0.,1.));
#31029=DIRECTION('ref_axis',(1.,0.,0.));
#31030=DIRECTION('',(0.,0.,-1.));
#31031=DIRECTION('center_axis',(0.,0.,1.));
#31032=DIRECTION('ref_axis',(1.,0.,0.));
#31033=DIRECTION('',(0.,0.,-1.));
#31034=DIRECTION('center_axis',(0.,0.,1.));
#31035=DIRECTION('ref_axis',(1.,0.,0.));
#31036=DIRECTION('',(0.,0.,-1.));
#31037=DIRECTION('center_axis',(0.,0.,1.));
#31038=DIRECTION('ref_axis',(1.,0.,0.));
#31039=DIRECTION('',(0.,0.,-1.));
#31040=DIRECTION('center_axis',(0.,0.,1.));
#31041=DIRECTION('ref_axis',(1.,0.,0.));
#31042=DIRECTION('',(0.,0.,-1.));
#31043=DIRECTION('center_axis',(0.,0.,1.));
#31044=DIRECTION('ref_axis',(1.,0.,0.));
#31045=DIRECTION('',(0.,0.,-1.));
#31046=DIRECTION('center_axis',(0.,0.,1.));
#31047=DIRECTION('ref_axis',(1.,0.,0.));
#31048=DIRECTION('',(0.,0.,-1.));
#31049=DIRECTION('center_axis',(0.,0.,1.));
#31050=DIRECTION('ref_axis',(1.,0.,0.));
#31051=DIRECTION('',(0.,0.,-1.));
#31052=DIRECTION('center_axis',(0.,0.,1.));
#31053=DIRECTION('ref_axis',(1.,0.,0.));
#31054=DIRECTION('',(0.,0.,-1.));
#31055=DIRECTION('center_axis',(0.,0.,1.));
#31056=DIRECTION('ref_axis',(1.,0.,0.));
#31057=DIRECTION('',(0.,0.,-1.));
#31058=DIRECTION('center_axis',(0.,0.,1.));
#31059=DIRECTION('ref_axis',(1.,0.,0.));
#31060=DIRECTION('',(0.,0.,-1.));
#31061=DIRECTION('center_axis',(0.,0.,1.));
#31062=DIRECTION('ref_axis',(1.,0.,0.));
#31063=DIRECTION('',(0.,0.,-1.));
#31064=DIRECTION('center_axis',(0.,0.,1.));
#31065=DIRECTION('ref_axis',(1.,0.,0.));
#31066=DIRECTION('',(0.,0.,-1.));
#31067=DIRECTION('center_axis',(0.,0.,1.));
#31068=DIRECTION('ref_axis',(-0.082458823014217,-0.99659447244459,0.));
#31069=DIRECTION('',(0.,0.,1.));
#31070=DIRECTION('center_axis',(0.,0.,1.));
#31071=DIRECTION('ref_axis',(1.,1.20322412993372E-13,0.));
#31072=DIRECTION('center_axis',(0.,0.,1.));
#31073=DIRECTION('ref_axis',(1.,1.20322412993372E-13,0.));
#31074=DIRECTION('',(0.,0.,1.));
#31075=DIRECTION('center_axis',(0.,0.,1.));
#31076=DIRECTION('ref_axis',(1.,1.20322412993372E-13,0.));
#31077=DIRECTION('',(0.,0.,1.));
#31078=DIRECTION('center_axis',(0.,0.,1.));
#31079=DIRECTION('ref_axis',(1.,1.20322412993372E-13,0.));
#31080=DIRECTION('',(0.,0.,1.));
#31081=DIRECTION('center_axis',(0.,0.,1.));
#31082=DIRECTION('ref_axis',(1.,1.20322412993372E-13,0.));
#31083=DIRECTION('',(0.,0.,1.));
#31084=DIRECTION('center_axis',(0.,0.,1.));
#31085=DIRECTION('ref_axis',(1.,1.20322412993372E-13,0.));
#31086=DIRECTION('',(0.,0.,1.));
#31087=DIRECTION('center_axis',(0.,0.,1.));
#31088=DIRECTION('ref_axis',(1.,1.20322412993372E-13,0.));
#31089=DIRECTION('',(0.,0.,1.));
#31090=DIRECTION('center_axis',(0.,0.,1.));
#31091=DIRECTION('ref_axis',(1.,1.20322412993372E-13,0.));
#31092=DIRECTION('',(0.,0.,1.));
#31093=DIRECTION('center_axis',(0.,0.,1.));
#31094=DIRECTION('ref_axis',(1.,1.20322412993372E-13,0.));
#31095=DIRECTION('',(0.,0.,1.));
#31096=DIRECTION('center_axis',(0.,0.,1.));
#31097=DIRECTION('ref_axis',(1.,1.20322412993372E-13,0.));
#31098=DIRECTION('',(0.,0.,1.));
#31099=DIRECTION('center_axis',(0.,0.,1.));
#31100=DIRECTION('ref_axis',(1.,1.20322412993372E-13,0.));
#31101=DIRECTION('',(0.,0.,1.));
#31102=DIRECTION('center_axis',(0.,0.,1.));
#31103=DIRECTION('ref_axis',(1.,1.20322412993372E-13,0.));
#31104=DIRECTION('',(0.,0.,1.));
#31105=DIRECTION('center_axis',(0.,0.,1.));
#31106=DIRECTION('ref_axis',(1.,1.20322412993372E-13,0.));
#31107=DIRECTION('',(0.,0.,1.));
#31108=DIRECTION('center_axis',(0.,0.,1.));
#31109=DIRECTION('ref_axis',(1.,1.20322412993372E-13,0.));
#31110=DIRECTION('',(0.,0.,1.));
#31111=DIRECTION('center_axis',(0.,0.,1.));
#31112=DIRECTION('ref_axis',(1.,1.20322412993372E-13,0.));
#31113=DIRECTION('',(0.,0.,1.));
#31114=DIRECTION('center_axis',(0.,0.,1.));
#31115=DIRECTION('ref_axis',(1.,1.20322412993372E-13,0.));
#31116=DIRECTION('',(0.,0.,1.));
#31117=DIRECTION('center_axis',(0.,0.,1.));
#31118=DIRECTION('ref_axis',(1.,1.20322412993372E-13,0.));
#31119=DIRECTION('',(0.,0.,1.));
#31120=DIRECTION('center_axis',(0.,0.,1.));
#31121=DIRECTION('ref_axis',(1.,1.20322412993372E-13,0.));
#31122=DIRECTION('',(0.,0.,1.));
#31123=DIRECTION('center_axis',(0.,0.,1.));
#31124=DIRECTION('ref_axis',(1.,1.20322412993372E-13,0.));
#31125=DIRECTION('',(0.,0.,1.));
#31126=DIRECTION('center_axis',(0.,0.,1.));
#31127=DIRECTION('ref_axis',(1.,0.,0.));
#31128=DIRECTION('center_axis',(0.,0.,1.));
#31129=DIRECTION('ref_axis',(1.,0.,0.));
#31130=DIRECTION('center_axis',(0.,0.,1.));
#31131=DIRECTION('ref_axis',(1.,0.,0.));
#31132=DIRECTION('center_axis',(0.,0.,1.));
#31133=DIRECTION('ref_axis',(1.,0.,0.));
#31134=DIRECTION('center_axis',(0.,0.,-1.));
#31135=DIRECTION('ref_axis',(1.,1.20322412993372E-13,0.));
#31136=DIRECTION('center_axis',(0.,0.,1.));
#31137=DIRECTION('ref_axis',(-0.0824588795393025,0.996594467767669,0.));
#31138=DIRECTION('center_axis',(0.,0.,1.));
#31139=DIRECTION('ref_axis',(0.984807753012208,-0.17364817766693,0.));
#31140=DIRECTION('center_axis',(0.,0.,-1.));
#31141=DIRECTION('ref_axis',(1.,0.,0.));
#31142=DIRECTION('',(-0.996089805327885,-0.0883464754353937,0.));
#31143=DIRECTION('',(0.905801965515954,-0.423701309022564,0.));
#31144=DIRECTION('center_axis',(-0.423701309022564,-0.905801965515954,0.));
#31145=DIRECTION('ref_axis',(0.905801965515954,-0.423701309022564,0.));
#31146=DIRECTION('',(0.,0.,1.));
#31147=DIRECTION('',(0.,0.,1.));
#31148=DIRECTION('center_axis',(-0.0883464754353937,0.996089805327885,0.));
#31149=DIRECTION('ref_axis',(-0.996089805327885,-0.0883464754353937,0.));
#31150=DIRECTION('',(0.,0.,-1.));
#31151=DIRECTION('center_axis',(0.,0.,1.));
#31152=DIRECTION('ref_axis',(0.939692620785908,-0.342020143325669,0.));
#31153=DIRECTION('center_axis',(0.,0.,-1.));
#31154=DIRECTION('ref_axis',(1.,0.,0.));
#31155=DIRECTION('',(-0.996298167445974,0.0859648855277171,0.));
#31156=DIRECTION('',(0.818465838146947,-0.574555194725812,0.));
#31157=DIRECTION('center_axis',(-0.574555194725812,-0.818465838146947,0.));
#31158=DIRECTION('ref_axis',(0.818465838146947,-0.574555194725812,0.));
#31159=DIRECTION('',(0.,0.,1.));
#31160=DIRECTION('',(0.,0.,1.));
#31161=DIRECTION('center_axis',(0.0859648855277171,0.996298167445974,0.));
#31162=DIRECTION('ref_axis',(-0.996298167445974,0.0859648855277171,0.));
#31163=DIRECTION('',(0.,0.,-1.));
#31164=DIRECTION('center_axis',(0.,0.,1.));
#31165=DIRECTION('ref_axis',(0.866025403784438,-0.5,0.));
#31166=DIRECTION('center_axis',(0.,0.,-1.));
#31167=DIRECTION('ref_axis',(1.,0.,0.));
#31168=DIRECTION('',(-0.966234513897416,0.257664246944398,0.));
#31169=DIRECTION('',(0.706261040449543,-0.707951511576272,0.));
#31170=DIRECTION('center_axis',(-0.707951511576272,-0.706261040449543,0.));
#31171=DIRECTION('ref_axis',(0.706261040449543,-0.707951511576272,0.));
#31172=DIRECTION('',(0.,0.,1.));
#31173=DIRECTION('',(0.,0.,1.));
#31174=DIRECTION('center_axis',(0.257664246944398,0.966234513897416,0.));
#31175=DIRECTION('ref_axis',(-0.966234513897416,0.257664246944398,0.));
#31176=DIRECTION('',(0.,0.,-1.));
#31177=DIRECTION('center_axis',(0.,0.,1.));
#31178=DIRECTION('ref_axis',(0.766044443118978,-0.64278760968654,0.));
#31179=DIRECTION('center_axis',(0.,0.,-1.));
#31180=DIRECTION('ref_axis',(1.,0.,0.));
#31181=DIRECTION('',(-0.906812313582341,0.421534610602074,0.));
#31182=DIRECTION('',(0.57259685842341,-0.819837079988238,0.));
#31183=DIRECTION('center_axis',(-0.819837079988238,-0.57259685842341,0.));
#31184=DIRECTION('ref_axis',(0.57259685842341,-0.819837079988238,0.));
#31185=DIRECTION('',(0.,0.,1.));
#31186=DIRECTION('',(0.,0.,1.));
#31187=DIRECTION('center_axis',(0.421534610602074,0.906812313582341,0.));
#31188=DIRECTION('ref_axis',(-0.906812313582341,0.421534610602074,0.));
#31189=DIRECTION('',(0.,0.,-1.));
#31190=DIRECTION('center_axis',(0.,0.,1.));
#31191=DIRECTION('ref_axis',(0.642787609686539,-0.766044443118978,0.));
#31192=DIRECTION('center_axis',(0.,0.,-1.));
#31193=DIRECTION('ref_axis',(1.,0.,0.));
#31194=DIRECTION('',(-0.819837079988238,0.572596858423411,0.));
#31195=DIRECTION('',(0.421534610602073,-0.906812313582341,0.));
#31196=DIRECTION('center_axis',(-0.906812313582341,-0.421534610602073,0.));
#31197=DIRECTION('ref_axis',(0.421534610602073,-0.906812313582341,0.));
#31198=DIRECTION('',(0.,0.,1.));
#31199=DIRECTION('',(0.,0.,1.));
#31200=DIRECTION('center_axis',(0.572596858423411,0.819837079988238,0.));
#31201=DIRECTION('ref_axis',(-0.819837079988238,0.572596858423411,0.));
#31202=DIRECTION('',(0.,0.,-1.));
#31203=DIRECTION('center_axis',(0.,0.,1.));
#31204=DIRECTION('ref_axis',(0.5,-0.866025403784438,0.));
#31205=DIRECTION('center_axis',(0.,0.,-1.));
#31206=DIRECTION('ref_axis',(1.,0.,0.));
#31207=DIRECTION('',(-0.707951511576272,0.706261040449543,0.));
#31208=DIRECTION('',(0.257664246944398,-0.966234513897416,0.));
#31209=DIRECTION('center_axis',(-0.966234513897416,-0.257664246944398,0.));
#31210=DIRECTION('ref_axis',(0.257664246944398,-0.966234513897416,0.));
#31211=DIRECTION('',(0.,0.,1.));
#31212=DIRECTION('',(0.,0.,1.));
#31213=DIRECTION('center_axis',(0.706261040449543,0.707951511576272,0.));
#31214=DIRECTION('ref_axis',(-0.707951511576272,0.706261040449543,0.));
#31215=DIRECTION('',(0.,0.,-1.));
#31216=DIRECTION('center_axis',(0.,0.,1.));
#31217=DIRECTION('ref_axis',(0.342020143325668,-0.939692620785909,0.));
#31218=DIRECTION('center_axis',(0.,0.,-1.));
#31219=DIRECTION('ref_axis',(1.,0.,0.));
#31220=DIRECTION('',(-0.574555194725811,0.818465838146948,0.));
#31221=DIRECTION('',(0.0859648855277157,-0.996298167445974,0.));
#31222=DIRECTION('center_axis',(-0.996298167445974,-0.0859648855277157,
0.));
#31223=DIRECTION('ref_axis',(0.0859648855277157,-0.996298167445974,0.));
#31224=DIRECTION('',(0.,0.,1.));
#31225=DIRECTION('',(0.,0.,1.));
#31226=DIRECTION('center_axis',(0.818465838146948,0.574555194725811,0.));
#31227=DIRECTION('ref_axis',(-0.574555194725811,0.818465838146948,0.));
#31228=DIRECTION('',(0.,0.,-1.));
#31229=DIRECTION('center_axis',(0.,0.,1.));
#31230=DIRECTION('ref_axis',(0.17364817766693,-0.984807753012208,0.));
#31231=DIRECTION('center_axis',(0.,0.,-1.));
#31232=DIRECTION('ref_axis',(1.,0.,0.));
#31233=DIRECTION('',(-0.423701309022563,0.905801965515955,0.));
#31234=DIRECTION('',(-0.0883464754353941,-0.996089805327885,0.));
#31235=DIRECTION('center_axis',(-0.996089805327885,0.0883464754353941,0.));
#31236=DIRECTION('ref_axis',(-0.0883464754353941,-0.996089805327885,0.));
#31237=DIRECTION('',(0.,0.,1.));
#31238=DIRECTION('',(0.,0.,1.));
#31239=DIRECTION('center_axis',(0.905801965515955,0.423701309022563,0.));
#31240=DIRECTION('ref_axis',(-0.423701309022563,0.905801965515955,0.));
#31241=DIRECTION('',(0.,0.,-1.));
#31242=DIRECTION('center_axis',(0.,0.,1.));
#31243=DIRECTION('ref_axis',(-1.94289029309402E-16,-1.,0.));
#31244=DIRECTION('center_axis',(0.,0.,-1.));
#31245=DIRECTION('ref_axis',(1.,0.,0.));
#31246=DIRECTION('',(-0.259973473447873,0.96561575852067,0.));
#31247=DIRECTION('',(-0.259973473447873,-0.96561575852067,0.));
#31248=DIRECTION('center_axis',(-0.96561575852067,0.259973473447873,0.));
#31249=DIRECTION('ref_axis',(-0.259973473447873,-0.96561575852067,0.));
#31250=DIRECTION('',(0.,0.,1.));
#31251=DIRECTION('',(0.,0.,1.));
#31252=DIRECTION('center_axis',(0.96561575852067,0.259973473447873,0.));
#31253=DIRECTION('ref_axis',(-0.259973473447873,0.96561575852067,0.));
#31254=DIRECTION('',(0.,0.,-1.));
#31255=DIRECTION('center_axis',(0.,0.,1.));
#31256=DIRECTION('ref_axis',(-0.17364817766693,-0.984807753012208,0.));
#31257=DIRECTION('center_axis',(0.,0.,-1.));
#31258=DIRECTION('ref_axis',(1.,0.,0.));
#31259=DIRECTION('',(-0.0883464754353937,0.996089805327885,0.));
#31260=DIRECTION('',(-0.423701309022564,-0.905801965515954,0.));
#31261=DIRECTION('center_axis',(-0.905801965515954,0.423701309022564,0.));
#31262=DIRECTION('ref_axis',(-0.423701309022564,-0.905801965515954,0.));
#31263=DIRECTION('',(0.,0.,1.));
#31264=DIRECTION('',(0.,0.,1.));
#31265=DIRECTION('center_axis',(0.996089805327885,0.0883464754353937,0.));
#31266=DIRECTION('ref_axis',(-0.0883464754353937,0.996089805327885,0.));
#31267=DIRECTION('',(0.,0.,-1.));
#31268=DIRECTION('center_axis',(0.,0.,1.));
#31269=DIRECTION('ref_axis',(-0.342020143325669,-0.939692620785908,0.));
#31270=DIRECTION('center_axis',(0.,0.,-1.));
#31271=DIRECTION('ref_axis',(1.,0.,0.));
#31272=DIRECTION('',(0.0859648855277171,0.996298167445974,0.));
#31273=DIRECTION('',(-0.574555194725812,-0.818465838146947,0.));
#31274=DIRECTION('center_axis',(-0.818465838146947,0.574555194725812,0.));
#31275=DIRECTION('ref_axis',(-0.574555194725812,-0.818465838146947,0.));
#31276=DIRECTION('',(0.,0.,1.));
#31277=DIRECTION('',(0.,0.,1.));
#31278=DIRECTION('center_axis',(0.996298167445974,-0.0859648855277171,0.));
#31279=DIRECTION('ref_axis',(0.0859648855277171,0.996298167445974,0.));
#31280=DIRECTION('',(0.,0.,-1.));
#31281=DIRECTION('center_axis',(0.,0.,1.));
#31282=DIRECTION('ref_axis',(-0.5,-0.866025403784438,0.));
#31283=DIRECTION('center_axis',(0.,0.,-1.));
#31284=DIRECTION('ref_axis',(1.,0.,0.));
#31285=DIRECTION('',(0.257664246944398,0.966234513897416,0.));
#31286=DIRECTION('',(-0.707951511576272,-0.706261040449543,0.));
#31287=DIRECTION('center_axis',(-0.706261040449543,0.707951511576272,0.));
#31288=DIRECTION('ref_axis',(-0.707951511576272,-0.706261040449543,0.));
#31289=DIRECTION('',(0.,0.,1.));
#31290=DIRECTION('',(0.,0.,1.));
#31291=DIRECTION('center_axis',(0.966234513897416,-0.257664246944398,0.));
#31292=DIRECTION('ref_axis',(0.257664246944398,0.966234513897416,0.));
#31293=DIRECTION('',(0.,0.,-1.));
#31294=DIRECTION('center_axis',(0.,0.,1.));
#31295=DIRECTION('ref_axis',(-0.642787609686539,-0.766044443118978,0.));
#31296=DIRECTION('center_axis',(0.,0.,-1.));
#31297=DIRECTION('ref_axis',(1.,0.,0.));
#31298=DIRECTION('',(0.421534610602074,0.906812313582341,0.));
#31299=DIRECTION('',(-0.819837079988238,-0.57259685842341,0.));
#31300=DIRECTION('center_axis',(-0.572596858423411,0.819837079988238,0.));
#31301=DIRECTION('ref_axis',(-0.819837079988238,-0.57259685842341,0.));
#31302=DIRECTION('',(0.,0.,1.));
#31303=DIRECTION('',(0.,0.,1.));
#31304=DIRECTION('center_axis',(0.906812313582341,-0.421534610602074,0.));
#31305=DIRECTION('ref_axis',(0.421534610602074,0.906812313582341,0.));
#31306=DIRECTION('',(0.,0.,-1.));
#31307=DIRECTION('center_axis',(0.,0.,1.));
#31308=DIRECTION('ref_axis',(-0.766044443118978,-0.642787609686539,0.));
#31309=DIRECTION('center_axis',(0.,0.,-1.));
#31310=DIRECTION('ref_axis',(1.,0.,0.));
#31311=DIRECTION('',(0.572596858423411,0.819837079988238,0.));
#31312=DIRECTION('',(-0.906812313582341,-0.421534610602073,0.));
#31313=DIRECTION('center_axis',(-0.421534610602074,0.906812313582341,0.));
#31314=DIRECTION('ref_axis',(-0.906812313582341,-0.421534610602073,0.));
#31315=DIRECTION('',(0.,0.,1.));
#31316=DIRECTION('',(0.,0.,1.));
#31317=DIRECTION('center_axis',(0.819837079988238,-0.572596858423411,0.));
#31318=DIRECTION('ref_axis',(0.572596858423411,0.819837079988238,0.));
#31319=DIRECTION('',(0.,0.,-1.));
#31320=DIRECTION('center_axis',(0.,0.,1.));
#31321=DIRECTION('ref_axis',(-0.866025403784439,-0.5,0.));
#31322=DIRECTION('center_axis',(0.,0.,-1.));
#31323=DIRECTION('ref_axis',(1.,0.,0.));
#31324=DIRECTION('',(0.706261040449544,0.707951511576272,0.));
#31325=DIRECTION('',(-0.966234513897416,-0.257664246944397,0.));
#31326=DIRECTION('center_axis',(-0.257664246944397,0.966234513897416,0.));
#31327=DIRECTION('ref_axis',(-0.966234513897416,-0.257664246944397,0.));
#31328=DIRECTION('',(0.,0.,1.));
#31329=DIRECTION('',(0.,0.,1.));
#31330=DIRECTION('center_axis',(0.707951511576272,-0.706261040449544,0.));
#31331=DIRECTION('ref_axis',(0.706261040449544,0.707951511576272,0.));
#31332=DIRECTION('',(0.,0.,-1.));
#31333=DIRECTION('center_axis',(0.,0.,1.));
#31334=DIRECTION('ref_axis',(-0.939692620785909,-0.342020143325669,0.));
#31335=DIRECTION('center_axis',(0.,0.,-1.));
#31336=DIRECTION('ref_axis',(1.,0.,0.));
#31337=DIRECTION('',(0.818465838146947,0.574555194725811,0.));
#31338=DIRECTION('',(-0.996298167445974,-0.0859648855277162,0.));
#31339=DIRECTION('center_axis',(-0.0859648855277162,0.996298167445974,0.));
#31340=DIRECTION('ref_axis',(-0.996298167445974,-0.0859648855277162,0.));
#31341=DIRECTION('',(0.,0.,1.));
#31342=DIRECTION('',(0.,0.,1.));
#31343=DIRECTION('center_axis',(0.574555194725811,-0.818465838146948,0.));
#31344=DIRECTION('ref_axis',(0.818465838146947,0.574555194725811,0.));
#31345=DIRECTION('',(0.,0.,-1.));
#31346=DIRECTION('center_axis',(0.,0.,1.));
#31347=DIRECTION('ref_axis',(-0.984807753012208,-0.17364817766693,0.));
#31348=DIRECTION('center_axis',(0.,0.,-1.));
#31349=DIRECTION('ref_axis',(1.,0.,0.));
#31350=DIRECTION('',(0.905801965515954,0.423701309022563,0.));
#31351=DIRECTION('',(-0.996089805327885,0.0883464754353941,0.));
#31352=DIRECTION('center_axis',(0.0883464754353941,0.996089805327885,0.));
#31353=DIRECTION('ref_axis',(-0.996089805327885,0.0883464754353941,0.));
#31354=DIRECTION('',(0.,0.,1.));
#31355=DIRECTION('',(0.,0.,1.));
#31356=DIRECTION('center_axis',(0.423701309022563,-0.905801965515954,0.));
#31357=DIRECTION('ref_axis',(0.905801965515954,0.423701309022563,0.));
#31358=DIRECTION('',(0.,0.,-1.));
#31359=DIRECTION('center_axis',(0.,0.,1.));
#31360=DIRECTION('ref_axis',(-1.,1.11022302462516E-16,0.));
#31361=DIRECTION('center_axis',(0.,0.,-1.));
#31362=DIRECTION('ref_axis',(1.,0.,0.));
#31363=DIRECTION('',(0.96561575852067,0.259973473447873,0.));
#31364=DIRECTION('',(-0.96561575852067,0.259973473447873,0.));
#31365=DIRECTION('center_axis',(0.,0.,-1.));
#31366=DIRECTION('ref_axis',(1.,0.,0.));
#31367=DIRECTION('center_axis',(0.259973473447873,0.96561575852067,0.));
#31368=DIRECTION('ref_axis',(-0.96561575852067,0.259973473447873,0.));
#31369=DIRECTION('',(0.,0.,1.));
#31370=DIRECTION('',(0.,0.,1.));
#31371=DIRECTION('center_axis',(0.259973473447873,-0.96561575852067,0.));
#31372=DIRECTION('ref_axis',(0.96561575852067,0.259973473447873,0.));
#31373=DIRECTION('',(0.,0.,-1.));
#31374=DIRECTION('center_axis',(0.,0.,1.));
#31375=DIRECTION('ref_axis',(-0.984807753012208,0.173648177666931,0.));
#31376=DIRECTION('center_axis',(0.,0.,-1.));
#31377=DIRECTION('ref_axis',(1.,0.,0.));
#31378=DIRECTION('',(0.996089805327885,0.0883464754353933,0.));
#31379=DIRECTION('',(-0.905801965515954,0.423701309022564,0.));
#31380=DIRECTION('center_axis',(0.423701309022564,0.905801965515954,0.));
#31381=DIRECTION('ref_axis',(-0.905801965515954,0.423701309022564,0.));
#31382=DIRECTION('',(0.,0.,1.));
#31383=DIRECTION('',(0.,0.,1.));
#31384=DIRECTION('center_axis',(0.0883464754353933,-0.996089805327885,0.));
#31385=DIRECTION('ref_axis',(0.996089805327885,0.0883464754353933,0.));
#31386=DIRECTION('',(0.,0.,-1.));
#31387=DIRECTION('center_axis',(0.,0.,1.));
#31388=DIRECTION('ref_axis',(-0.939692620785908,0.342020143325669,0.));
#31389=DIRECTION('center_axis',(0.,0.,-1.));
#31390=DIRECTION('ref_axis',(1.,0.,0.));
#31391=DIRECTION('',(0.996298167445974,-0.0859648855277165,0.));
#31392=DIRECTION('',(-0.818465838146947,0.574555194725811,0.));
#31393=DIRECTION('center_axis',(0.574555194725811,0.818465838146947,0.));
#31394=DIRECTION('ref_axis',(-0.818465838146947,0.574555194725811,0.));
#31395=DIRECTION('',(0.,0.,1.));
#31396=DIRECTION('',(0.,0.,1.));
#31397=DIRECTION('center_axis',(-0.0859648855277165,-0.996298167445974,
0.));
#31398=DIRECTION('ref_axis',(0.996298167445974,-0.0859648855277165,0.));
#31399=DIRECTION('',(0.,0.,-1.));
#31400=DIRECTION('center_axis',(0.,0.,1.));
#31401=DIRECTION('ref_axis',(-0.866025403784439,0.5,0.));
#31402=DIRECTION('center_axis',(0.,0.,-1.));
#31403=DIRECTION('ref_axis',(1.,0.,0.));
#31404=DIRECTION('',(0.966234513897416,-0.257664246944398,0.));
#31405=DIRECTION('',(-0.706261040449544,0.707951511576272,0.));
#31406=DIRECTION('center_axis',(0.707951511576272,0.706261040449544,0.));
#31407=DIRECTION('ref_axis',(-0.706261040449544,0.707951511576272,0.));
#31408=DIRECTION('',(0.,0.,1.));
#31409=DIRECTION('',(0.,0.,1.));
#31410=DIRECTION('center_axis',(-0.257664246944398,-0.966234513897416,0.));
#31411=DIRECTION('ref_axis',(0.966234513897416,-0.257664246944398,0.));
#31412=DIRECTION('',(0.,0.,-1.));
#31413=DIRECTION('center_axis',(0.,0.,1.));
#31414=DIRECTION('ref_axis',(-0.766044443118978,0.642787609686539,0.));
#31415=DIRECTION('center_axis',(0.,0.,-1.));
#31416=DIRECTION('ref_axis',(1.,0.,0.));
#31417=DIRECTION('',(0.906812313582341,-0.421534610602074,0.));
#31418=DIRECTION('',(-0.57259685842341,0.819837079988238,0.));
#31419=DIRECTION('center_axis',(0.819837079988238,0.572596858423411,0.));
#31420=DIRECTION('ref_axis',(-0.57259685842341,0.819837079988238,0.));
#31421=DIRECTION('',(0.,0.,1.));
#31422=DIRECTION('',(0.,0.,1.));
#31423=DIRECTION('center_axis',(-0.421534610602074,-0.906812313582341,0.));
#31424=DIRECTION('ref_axis',(0.906812313582341,-0.421534610602074,0.));
#31425=DIRECTION('',(0.,0.,-1.));
#31426=DIRECTION('center_axis',(0.,0.,1.));
#31427=DIRECTION('ref_axis',(-0.642787609686539,0.766044443118978,0.));
#31428=DIRECTION('center_axis',(0.,0.,-1.));
#31429=DIRECTION('ref_axis',(1.,0.,0.));
#31430=DIRECTION('',(0.819837079988238,-0.572596858423411,0.));
#31431=DIRECTION('',(-0.421534610602074,0.906812313582341,0.));
#31432=DIRECTION('center_axis',(0.906812313582341,0.421534610602074,0.));
#31433=DIRECTION('ref_axis',(-0.421534610602074,0.906812313582341,0.));
#31434=DIRECTION('',(0.,0.,1.));
#31435=DIRECTION('',(0.,0.,1.));
#31436=DIRECTION('center_axis',(-0.572596858423411,-0.819837079988238,0.));
#31437=DIRECTION('ref_axis',(0.819837079988238,-0.572596858423411,0.));
#31438=DIRECTION('',(0.,0.,-1.));
#31439=DIRECTION('center_axis',(0.,0.,1.));
#31440=DIRECTION('ref_axis',(-0.5,0.866025403784439,0.));
#31441=DIRECTION('center_axis',(0.,0.,-1.));
#31442=DIRECTION('ref_axis',(1.,0.,0.));
#31443=DIRECTION('',(0.707951511576272,-0.706261040449544,0.));
#31444=DIRECTION('',(-0.257664246944397,0.966234513897416,0.));
#31445=DIRECTION('center_axis',(0.966234513897416,0.257664246944397,0.));
#31446=DIRECTION('ref_axis',(-0.257664246944397,0.966234513897416,0.));
#31447=DIRECTION('',(0.,0.,1.));
#31448=DIRECTION('',(0.,0.,1.));
#31449=DIRECTION('center_axis',(-0.706261040449544,-0.707951511576272,0.));
#31450=DIRECTION('ref_axis',(0.707951511576272,-0.706261040449544,0.));
#31451=DIRECTION('',(0.,0.,-1.));
#31452=DIRECTION('center_axis',(0.,0.,1.));
#31453=DIRECTION('ref_axis',(-0.342020143325669,0.939692620785909,0.));
#31454=DIRECTION('center_axis',(0.,0.,-1.));
#31455=DIRECTION('ref_axis',(1.,0.,0.));
#31456=DIRECTION('',(0.574555194725811,-0.818465838146947,0.));
#31457=DIRECTION('',(-0.0859648855277162,0.996298167445974,0.));
#31458=DIRECTION('center_axis',(0.996298167445974,0.0859648855277162,0.));
#31459=DIRECTION('ref_axis',(-0.0859648855277162,0.996298167445974,0.));
#31460=DIRECTION('',(0.,0.,1.));
#31461=DIRECTION('',(0.,0.,1.));
#31462=DIRECTION('center_axis',(-0.818465838146948,-0.574555194725811,0.));
#31463=DIRECTION('ref_axis',(0.574555194725811,-0.818465838146947,0.));
#31464=DIRECTION('',(0.,0.,-1.));
#31465=DIRECTION('center_axis',(0.,0.,1.));
#31466=DIRECTION('ref_axis',(-0.17364817766693,0.984807753012208,0.));
#31467=DIRECTION('center_axis',(0.,0.,-1.));
#31468=DIRECTION('ref_axis',(1.,0.,0.));
#31469=DIRECTION('',(0.423701309022564,-0.905801965515954,0.));
#31470=DIRECTION('',(0.0883464754353937,0.996089805327885,0.));
#31471=DIRECTION('center_axis',(0.996089805327885,-0.0883464754353937,0.));
#31472=DIRECTION('ref_axis',(0.0883464754353937,0.996089805327885,0.));
#31473=DIRECTION('',(0.,0.,1.));
#31474=DIRECTION('',(0.,0.,1.));
#31475=DIRECTION('center_axis',(-0.905801965515954,-0.423701309022564,0.));
#31476=DIRECTION('ref_axis',(0.423701309022564,-0.905801965515954,0.));
#31477=DIRECTION('',(0.,0.,-1.));
#31478=DIRECTION('center_axis',(0.,0.,1.));
#31479=DIRECTION('ref_axis',(5.55111512312578E-17,1.,0.));
#31480=DIRECTION('center_axis',(0.,0.,-1.));
#31481=DIRECTION('ref_axis',(1.,0.,0.));
#31482=DIRECTION('',(0.259973473447873,-0.96561575852067,0.));
#31483=DIRECTION('',(0.259973473447873,0.96561575852067,0.));
#31484=DIRECTION('center_axis',(0.96561575852067,-0.259973473447873,0.));
#31485=DIRECTION('ref_axis',(0.259973473447873,0.96561575852067,0.));
#31486=DIRECTION('',(0.,0.,1.));
#31487=DIRECTION('',(0.,0.,1.));
#31488=DIRECTION('center_axis',(-0.96561575852067,-0.259973473447873,0.));
#31489=DIRECTION('ref_axis',(0.259973473447873,-0.96561575852067,0.));
#31490=DIRECTION('',(0.,0.,-1.));
#31491=DIRECTION('center_axis',(0.,0.,1.));
#31492=DIRECTION('ref_axis',(0.17364817766693,0.984807753012208,0.));
#31493=DIRECTION('center_axis',(0.,0.,-1.));
#31494=DIRECTION('ref_axis',(1.,0.,0.));
#31495=DIRECTION('',(0.0883464754353936,-0.996089805327885,0.));
#31496=DIRECTION('',(0.423701309022564,0.905801965515954,0.));
#31497=DIRECTION('center_axis',(0.905801965515954,-0.423701309022564,0.));
#31498=DIRECTION('ref_axis',(0.423701309022564,0.905801965515954,0.));
#31499=DIRECTION('',(0.,0.,1.));
#31500=DIRECTION('',(0.,0.,1.));
#31501=DIRECTION('center_axis',(-0.996089805327885,-0.0883464754353936,
0.));
#31502=DIRECTION('ref_axis',(0.0883464754353936,-0.996089805327885,0.));
#31503=DIRECTION('',(0.,0.,-1.));
#31504=DIRECTION('center_axis',(0.,0.,1.));
#31505=DIRECTION('ref_axis',(0.342020143325669,0.939692620785908,0.));
#31506=DIRECTION('center_axis',(0.,0.,-1.));
#31507=DIRECTION('ref_axis',(1.,0.,0.));
#31508=DIRECTION('',(-0.0859648855277165,-0.996298167445974,0.));
#31509=DIRECTION('',(0.574555194725811,0.818465838146947,0.));
#31510=DIRECTION('center_axis',(0.818465838146947,-0.574555194725811,0.));
#31511=DIRECTION('ref_axis',(0.574555194725811,0.818465838146947,0.));
#31512=DIRECTION('',(0.,0.,1.));
#31513=DIRECTION('',(0.,0.,1.));
#31514=DIRECTION('center_axis',(-0.996298167445974,0.0859648855277165,0.));
#31515=DIRECTION('ref_axis',(-0.0859648855277165,-0.996298167445974,0.));
#31516=DIRECTION('',(0.,0.,-1.));
#31517=DIRECTION('center_axis',(0.,0.,1.));
#31518=DIRECTION('ref_axis',(0.5,0.866025403784439,0.));
#31519=DIRECTION('center_axis',(0.,0.,-1.));
#31520=DIRECTION('ref_axis',(1.,0.,0.));
#31521=DIRECTION('',(-0.257664246944398,-0.966234513897416,0.));
#31522=DIRECTION('',(0.707951511576272,0.706261040449543,0.));
#31523=DIRECTION('center_axis',(0.706261040449544,-0.707951511576272,0.));
#31524=DIRECTION('ref_axis',(0.707951511576272,0.706261040449543,0.));
#31525=DIRECTION('',(0.,0.,1.));
#31526=DIRECTION('',(0.,0.,1.));
#31527=DIRECTION('center_axis',(-0.966234513897416,0.257664246944398,0.));
#31528=DIRECTION('ref_axis',(-0.257664246944398,-0.966234513897416,0.));
#31529=DIRECTION('',(0.,0.,-1.));
#31530=DIRECTION('center_axis',(0.,0.,1.));
#31531=DIRECTION('ref_axis',(0.642787609686539,0.766044443118978,0.));
#31532=DIRECTION('center_axis',(0.,0.,-1.));
#31533=DIRECTION('ref_axis',(1.,0.,0.));
#31534=DIRECTION('',(-0.421534610602074,-0.906812313582341,0.));
#31535=DIRECTION('',(0.819837079988238,0.572596858423411,0.));
#31536=DIRECTION('center_axis',(0.572596858423411,-0.819837079988238,0.));
#31537=DIRECTION('ref_axis',(0.819837079988238,0.572596858423411,0.));
#31538=DIRECTION('',(0.,0.,1.));
#31539=DIRECTION('',(0.,0.,1.));
#31540=DIRECTION('center_axis',(-0.906812313582341,0.421534610602074,0.));
#31541=DIRECTION('ref_axis',(-0.421534610602074,-0.906812313582341,0.));
#31542=DIRECTION('',(0.,0.,-1.));
#31543=DIRECTION('center_axis',(0.,0.,1.));
#31544=DIRECTION('ref_axis',(0.766044443118978,0.642787609686539,0.));
#31545=DIRECTION('center_axis',(0.,0.,-1.));
#31546=DIRECTION('ref_axis',(1.,0.,0.));
#31547=DIRECTION('',(-0.572596858423411,-0.819837079988238,0.));
#31548=DIRECTION('',(0.906812313582341,0.421534610602073,0.));
#31549=DIRECTION('center_axis',(0.421534610602074,-0.906812313582341,0.));
#31550=DIRECTION('ref_axis',(0.906812313582341,0.421534610602073,0.));
#31551=DIRECTION('',(0.,0.,1.));
#31552=DIRECTION('',(0.,0.,1.));
#31553=DIRECTION('center_axis',(-0.819837079988238,0.572596858423411,0.));
#31554=DIRECTION('ref_axis',(-0.572596858423411,-0.819837079988238,0.));
#31555=DIRECTION('',(0.,0.,-1.));
#31556=DIRECTION('center_axis',(0.,0.,1.));
#31557=DIRECTION('ref_axis',(0.866025403784439,0.5,0.));
#31558=DIRECTION('center_axis',(0.,0.,-1.));
#31559=DIRECTION('ref_axis',(1.,0.,0.));
#31560=DIRECTION('',(-0.706261040449544,-0.707951511576272,0.));
#31561=DIRECTION('',(0.966234513897416,0.257664246944398,0.));
#31562=DIRECTION('center_axis',(0.257664246944398,-0.966234513897416,0.));
#31563=DIRECTION('ref_axis',(0.966234513897416,0.257664246944398,0.));
#31564=DIRECTION('',(0.,0.,1.));
#31565=DIRECTION('',(0.,0.,1.));
#31566=DIRECTION('center_axis',(-0.707951511576272,0.706261040449544,0.));
#31567=DIRECTION('ref_axis',(-0.706261040449544,-0.707951511576272,0.));
#31568=DIRECTION('',(0.,0.,-1.));
#31569=DIRECTION('center_axis',(0.,0.,1.));
#31570=DIRECTION('ref_axis',(0.939692620785909,0.342020143325669,0.));
#31571=DIRECTION('center_axis',(0.,0.,-1.));
#31572=DIRECTION('ref_axis',(1.,0.,0.));
#31573=DIRECTION('',(-0.818465838146947,-0.574555194725811,0.));
#31574=DIRECTION('',(0.996298167445974,0.0859648855277162,0.));
#31575=DIRECTION('center_axis',(0.0859648855277162,-0.996298167445974,0.));
#31576=DIRECTION('ref_axis',(0.996298167445974,0.0859648855277162,0.));
#31577=DIRECTION('',(0.,0.,1.));
#31578=DIRECTION('',(0.,0.,1.));
#31579=DIRECTION('center_axis',(-0.574555194725811,0.818465838146948,0.));
#31580=DIRECTION('ref_axis',(-0.818465838146947,-0.574555194725811,0.));
#31581=DIRECTION('',(0.,0.,-1.));
#31582=DIRECTION('center_axis',(0.,0.,1.));
#31583=DIRECTION('ref_axis',(0.984807753012208,0.17364817766693,0.));
#31584=DIRECTION('center_axis',(0.,0.,-1.));
#31585=DIRECTION('ref_axis',(1.,0.,0.));
#31586=DIRECTION('',(-0.905801965515954,-0.423701309022564,0.));
#31587=DIRECTION('',(0.996089805327885,-0.0883464754353937,0.));
#31588=DIRECTION('center_axis',(-0.0883464754353937,-0.996089805327885,
0.));
#31589=DIRECTION('ref_axis',(0.996089805327885,-0.0883464754353937,0.));
#31590=DIRECTION('',(0.,0.,1.));
#31591=DIRECTION('',(0.,0.,1.));
#31592=DIRECTION('center_axis',(-0.423701309022564,0.905801965515954,0.));
#31593=DIRECTION('ref_axis',(-0.905801965515954,-0.423701309022564,0.));
#31594=DIRECTION('',(0.,0.,-1.));
#31595=DIRECTION('center_axis',(0.,0.,1.));
#31596=DIRECTION('ref_axis',(1.,0.,0.));
#31597=DIRECTION('center_axis',(0.,0.,1.));
#31598=DIRECTION('ref_axis',(1.,0.,0.));
#31599=DIRECTION('center_axis',(0.,0.,1.));
#31600=DIRECTION('ref_axis',(1.,0.,0.));
#31601=DIRECTION('center_axis',(0.,0.,1.));
#31602=DIRECTION('ref_axis',(1.,0.,0.));
#31603=DIRECTION('center_axis',(0.,0.,1.));
#31604=DIRECTION('ref_axis',(1.,0.,0.));
#31605=DIRECTION('center_axis',(0.,0.,1.));
#31606=DIRECTION('ref_axis',(1.,0.,0.));
#31607=DIRECTION('center_axis',(0.,0.,1.));
#31608=DIRECTION('ref_axis',(1.,0.,0.));
#31609=DIRECTION('center_axis',(0.,0.,1.));
#31610=DIRECTION('ref_axis',(1.,0.,0.));
#31611=DIRECTION('center_axis',(0.,0.,1.));
#31612=DIRECTION('ref_axis',(1.,0.,0.));
#31613=DIRECTION('center_axis',(0.,0.,1.));
#31614=DIRECTION('ref_axis',(1.,0.,0.));
#31615=DIRECTION('center_axis',(0.,0.,1.));
#31616=DIRECTION('ref_axis',(1.,0.,0.));
#31617=DIRECTION('center_axis',(0.,0.,1.));
#31618=DIRECTION('ref_axis',(1.,0.,0.));
#31619=DIRECTION('center_axis',(0.,0.,1.));
#31620=DIRECTION('ref_axis',(1.,0.,0.));
#31621=DIRECTION('center_axis',(0.,0.,1.));
#31622=DIRECTION('ref_axis',(1.,0.,0.));
#31623=DIRECTION('center_axis',(0.,0.,1.));
#31624=DIRECTION('ref_axis',(1.,0.,0.));
#31625=DIRECTION('center_axis',(0.,0.,1.));
#31626=DIRECTION('ref_axis',(1.,0.,0.));
#31627=DIRECTION('center_axis',(0.,0.,1.));
#31628=DIRECTION('ref_axis',(1.,0.,0.));
#31629=DIRECTION('center_axis',(0.,0.,1.));
#31630=DIRECTION('ref_axis',(1.,0.,0.));
#31631=DIRECTION('',(0.,0.,-1.));
#31632=DIRECTION('center_axis',(0.,0.,1.));
#31633=DIRECTION('ref_axis',(1.,0.,0.));
#31634=DIRECTION('center_axis',(0.,0.,1.));
#31635=DIRECTION('ref_axis',(1.,0.,0.));
#31636=DIRECTION('center_axis',(0.,0.,1.));
#31637=DIRECTION('ref_axis',(1.,0.,0.));
#31638=DIRECTION('center_axis',(0.,0.,1.));
#31639=DIRECTION('ref_axis',(1.,0.,0.));
#31640=DIRECTION('center_axis',(0.,0.,1.));
#31641=DIRECTION('ref_axis',(1.,0.,0.));
#31642=DIRECTION('center_axis',(0.,0.,1.));
#31643=DIRECTION('ref_axis',(1.,0.,0.));
#31644=DIRECTION('center_axis',(0.,0.,1.));
#31645=DIRECTION('ref_axis',(1.,0.,0.));
#31646=DIRECTION('center_axis',(0.,0.,1.));
#31647=DIRECTION('ref_axis',(1.,0.,0.));
#31648=DIRECTION('center_axis',(0.,0.,1.));
#31649=DIRECTION('ref_axis',(1.,0.,0.));
#31650=DIRECTION('center_axis',(0.,0.,1.));
#31651=DIRECTION('ref_axis',(1.,0.,0.));
#31652=DIRECTION('center_axis',(0.,0.,1.));
#31653=DIRECTION('ref_axis',(1.,0.,0.));
#31654=DIRECTION('center_axis',(0.,0.,1.));
#31655=DIRECTION('ref_axis',(1.,0.,0.));
#31656=DIRECTION('center_axis',(0.,0.,1.));
#31657=DIRECTION('ref_axis',(1.,0.,0.));
#31658=DIRECTION('center_axis',(0.,0.,1.));
#31659=DIRECTION('ref_axis',(1.,0.,0.));
#31660=DIRECTION('center_axis',(0.,0.,1.));
#31661=DIRECTION('ref_axis',(1.,0.,0.));
#31662=DIRECTION('center_axis',(0.,0.,1.));
#31663=DIRECTION('ref_axis',(1.,0.,0.));
#31664=DIRECTION('center_axis',(0.,0.,1.));
#31665=DIRECTION('ref_axis',(1.,0.,0.));
#31666=DIRECTION('center_axis',(0.,0.,1.));
#31667=DIRECTION('ref_axis',(1.,0.,0.));
#31668=DIRECTION('center_axis',(0.,0.,1.));
#31669=DIRECTION('ref_axis',(1.,0.,0.));
#31670=DIRECTION('',(0.,0.,-1.));
#31671=DIRECTION('center_axis',(0.,0.,-1.));
#31672=DIRECTION('ref_axis',(1.,0.,0.));
#31673=DIRECTION('',(0.,0.,1.));
#31674=DIRECTION('center_axis',(0.,0.,1.));
#31675=DIRECTION('ref_axis',(1.,0.,0.));
#31676=DIRECTION('center_axis',(-0.259973473447873,-0.96561575852067,0.));
#31677=DIRECTION('ref_axis',(0.96561575852067,-0.259973473447873,0.));
#31678=DIRECTION('',(0.96561575852067,-0.259973473447873,0.));
#31679=DIRECTION('',(0.,0.,1.));
#31680=DIRECTION('center_axis',(-0.259973473447873,0.96561575852067,0.));
#31681=DIRECTION('ref_axis',(-0.96561575852067,-0.259973473447873,0.));
#31682=DIRECTION('',(-0.96561575852067,-0.259973473447873,0.));
#31683=DIRECTION('center_axis',(0.,0.,1.));
#31684=DIRECTION('ref_axis',(1.,0.,0.));
#31685=DIRECTION('center_axis',(0.,0.,-1.));
#31686=DIRECTION('ref_axis',(1.,0.,0.));
#31687=DIRECTION('center_axis',(0.,0.,1.));
#31688=DIRECTION('ref_axis',(1.,0.,0.));
#31689=DIRECTION('',(-0.707106781186548,-8.65956056235493E-17,-0.707106781186548));
#31690=DIRECTION('center_axis',(0.,0.,1.));
#31691=DIRECTION('ref_axis',(1.,0.,0.));
#31692=DIRECTION('',(-0.845934045579678,-1.03597042120892E-16,0.533287530821037));
#31693=DIRECTION('center_axis',(0.,0.,-1.));
#31694=DIRECTION('ref_axis',(1.,0.,0.));
#31695=DIRECTION('center_axis',(0.5,0.866025403784439,0.));
#31696=DIRECTION('ref_axis',(0.866025403784439,-0.5,0.));
#31697=DIRECTION('',(0.866025403784439,-0.5,0.));
#31698=DIRECTION('',(0.,0.,-1.));
#31699=DIRECTION('',(0.866025403784439,-0.5,0.));
#31700=DIRECTION('',(0.,0.,-1.));
#31701=DIRECTION('center_axis',(-0.5,0.866025403784439,0.));
#31702=DIRECTION('ref_axis',(0.866025403784439,0.5,0.));
#31703=DIRECTION('',(0.866025403784439,0.5,0.));
#31704=DIRECTION('',(0.,0.,-1.));
#31705=DIRECTION('',(0.866025403784439,0.5,0.));
#31706=DIRECTION('center_axis',(-1.,-1.20185167898973E-16,0.));
#31707=DIRECTION('ref_axis',(-1.20185167898973E-16,1.,0.));
#31708=DIRECTION('',(-1.20185167898973E-16,1.,0.));
#31709=DIRECTION('',(0.,0.,-1.));
#31710=DIRECTION('',(-1.20185167898973E-16,1.,0.));
#31711=DIRECTION('center_axis',(-0.5,-0.866025403784439,0.));
#31712=DIRECTION('ref_axis',(-0.866025403784439,0.5,0.));
#31713=DIRECTION('',(-0.866025403784439,0.5,0.));
#31714=DIRECTION('',(0.,0.,-1.));
#31715=DIRECTION('',(-0.866025403784439,0.5,0.));
#31716=DIRECTION('center_axis',(0.5,-0.866025403784439,0.));
#31717=DIRECTION('ref_axis',(-0.866025403784439,-0.5,0.));
#31718=DIRECTION('',(-0.866025403784439,-0.5,0.));
#31719=DIRECTION('',(0.,0.,-1.));
#31720=DIRECTION('',(-0.866025403784439,-0.5,0.));
#31721=DIRECTION('center_axis',(1.,-3.60555503696918E-16,0.));
#31722=DIRECTION('ref_axis',(-3.60555503696918E-16,-1.,0.));
#31723=DIRECTION('',(-3.60555503696918E-16,-1.,0.));
#31724=DIRECTION('',(-3.60555503696918E-16,-1.,0.));
#31725=DIRECTION('center_axis',(0.,0.,-1.));
#31726=DIRECTION('ref_axis',(-1.,0.,0.));
#31727=DIRECTION('center_axis',(0.,0.,-1.));
#31728=DIRECTION('ref_axis',(-1.,0.,0.));
#31729=DIRECTION('center_axis',(0.,0.,1.));
#31730=DIRECTION('ref_axis',(1.,0.,0.));
#31731=DIRECTION('center_axis',(0.,0.,1.));
#31732=DIRECTION('ref_axis',(1.,0.,0.));
#31733=DIRECTION('',(0.707106781186547,8.65956056235493E-17,-0.707106781186548));
#31734=DIRECTION('center_axis',(0.,0.,1.));
#31735=DIRECTION('ref_axis',(1.,0.,0.));
#31736=DIRECTION('center_axis',(0.,0.,1.));
#31737=DIRECTION('ref_axis',(1.,0.,0.));
#31738=DIRECTION('center_axis',(0.,0.,1.));
#31739=DIRECTION('ref_axis',(1.,0.,0.));
#31740=DIRECTION('center_axis',(0.,0.,1.));
#31741=DIRECTION('ref_axis',(1.,0.,0.));
#31742=DIRECTION('',(0.707106781186548,8.65956056235494E-17,-0.707106781186547));
#31743=DIRECTION('center_axis',(0.,0.,-1.));
#31744=DIRECTION('ref_axis',(-1.,0.,0.));
#31745=DIRECTION('center_axis',(0.,0.,1.));
#31746=DIRECTION('ref_axis',(1.,0.,0.));
#31747=DIRECTION('',(0.,0.,1.));
#31748=DIRECTION('',(1.,0.,0.));
#31749=DIRECTION('',(0.,0.,1.));
#31750=DIRECTION('',(1.,0.,0.));
#31751=DIRECTION('',(0.,0.,1.));
#31752=DIRECTION('',(1.,0.,0.));
#31753=DIRECTION('',(0.,-1.,0.));
#31754=DIRECTION('',(1.,0.,0.));
#31755=DIRECTION('',(0.,-1.,0.));
#31756=DIRECTION('',(1.,0.,0.));
#31757=DIRECTION('',(0.,-1.,0.));
#31758=DIRECTION('',(1.,0.,0.));
#31759=DIRECTION('',(0.,1.,0.));
#31760=DIRECTION('',(1.,0.,0.));
#31761=DIRECTION('',(0.,-1.,0.));
#31762=DIRECTION('',(1.,0.,0.));
#31763=DIRECTION('',(0.,-1.,0.));
#31764=DIRECTION('',(0.707106781186548,0.,0.707106781186548));
#31765=DIRECTION('',(0.,-1.,0.));
#31766=DIRECTION('',(1.,0.,0.));
#31767=DIRECTION('',(0.,-1.,0.));
#31768=DIRECTION('',(1.,0.,0.));
#31769=DIRECTION('',(0.,1.,0.));
#31770=DIRECTION('',(1.,0.,0.));
#31771=DIRECTION('',(0.,0.,1.));
#31772=DIRECTION('',(1.,0.,0.));
#31773=DIRECTION('',(0.,1.,0.));
#31774=DIRECTION('',(1.,0.,0.));
#31775=DIRECTION('',(0.,1.,0.));
#31776=DIRECTION('',(1.,0.,0.));
#31777=DIRECTION('',(0.,0.,-1.));
#31778=DIRECTION('',(1.,0.,0.));
#31779=DIRECTION('',(0.,1.,0.));
#31780=DIRECTION('',(1.,0.,0.));
#31781=DIRECTION('',(0.,-1.,0.));
#31782=DIRECTION('',(1.,0.,0.));
#31783=DIRECTION('',(0.,-1.,0.));
#31784=DIRECTION('',(1.,0.,0.));
#31785=DIRECTION('',(0.,1.,0.));
#31786=DIRECTION('',(1.,0.,0.));
#31787=DIRECTION('',(0.,1.,0.));
#31788=DIRECTION('',(1.,0.,0.));
#31789=DIRECTION('',(0.,1.,0.));
#31790=DIRECTION('',(1.,0.,0.));
#31791=DIRECTION('',(0.,-1.,0.));
#31792=DIRECTION('',(-0.707106781186547,0.,0.707106781186548));
#31793=DIRECTION('',(0.,-1.,0.));
#31794=DIRECTION('',(-1.83697019872103E-16,0.,-1.));
#31795=DIRECTION('',(0.,-1.,0.));
#31796=DIRECTION('',(1.,0.,0.));
#31797=DIRECTION('',(0.,-1.,0.));
#31798=DIRECTION('',(1.,0.,0.));
#31799=DIRECTION('',(0.,-1.,0.));
#31800=DIRECTION('',(1.,0.,0.));
#31801=DIRECTION('',(0.,-1.,0.));
#31802=DIRECTION('',(1.,0.,0.));
#31803=DIRECTION('',(0.,1.,0.));
#31804=DIRECTION('',(1.,0.,0.));
#31805=DIRECTION('',(0.,1.,0.));
#31806=DIRECTION('',(1.,0.,0.));
#31807=DIRECTION('',(0.,1.,0.));
#31808=DIRECTION('',(1.,0.,0.));
#31809=DIRECTION('',(0.,1.,0.));
#31810=DIRECTION('',(1.,0.,0.));
#31811=DIRECTION('',(0.,0.,-1.));
#31812=DIRECTION('',(1.,0.,0.));
#31813=DIRECTION('',(0.,0.,-1.));
#31814=DIRECTION('',(1.,0.,0.));
#31815=CARTESIAN_POINT('',(0.,0.,0.));
#31816=CARTESIAN_POINT('',(0.,0.,0.));
#31817=CARTESIAN_POINT('Origin',(-5.9,-4.15,1.1893933982822));
#31818=CARTESIAN_POINT('',(-6.37,-4.15,1.2));
#31819=CARTESIAN_POINT('',(-6.4212132034356,-4.15,1.1787867965644));
#31820=CARTESIAN_POINT('',(-6.37,-4.15,1.2));
#31821=CARTESIAN_POINT('',(-5.9,-4.6712132034356,1.1787867965644));
#31822=CARTESIAN_POINT('Origin',(-5.9,-4.15,1.1787867965644));
#31823=CARTESIAN_POINT('',(-5.9,-4.62,1.2));
#31824=CARTESIAN_POINT('',(-5.9,-4.6712132034356,1.1787867965644));
#31825=CARTESIAN_POINT('Origin',(-5.9,-4.15,1.2));
#31826=CARTESIAN_POINT('Origin',(-6.3956066017178,1.1875,1.1893933982822));
#31827=CARTESIAN_POINT('',(-6.37,4.15,1.2));
#31828=CARTESIAN_POINT('',(-6.4212132034356,4.15,1.1787867965644));
#31829=CARTESIAN_POINT('',(-6.37,4.15,1.2));
#31830=CARTESIAN_POINT('',(-6.4212132034356,1.1875,1.1787867965644));
#31831=CARTESIAN_POINT('',(-6.37,1.1875,1.2));
#31832=CARTESIAN_POINT('Origin',(-5.9,4.15,1.1893933982822));
#31833=CARTESIAN_POINT('',(-5.9,4.62,1.2));
#31834=CARTESIAN_POINT('',(-5.9,4.6712132034356,1.1787867965644));
#31835=CARTESIAN_POINT('',(-5.9,4.62,1.2));
#31836=CARTESIAN_POINT('Origin',(-5.9,4.15,1.1787867965644));
#31837=CARTESIAN_POINT('Origin',(-5.9,4.15,1.2));
#31838=CARTESIAN_POINT('Origin',(1.625,4.6456066017178,1.1893933982822));
#31839=CARTESIAN_POINT('',(5.9,4.62,1.2));
#31840=CARTESIAN_POINT('',(5.9,4.6712132034356,1.1787867965644));
#31841=CARTESIAN_POINT('',(5.9,4.62,1.2));
#31842=CARTESIAN_POINT('',(1.625,4.6712132034356,1.1787867965644));
#31843=CARTESIAN_POINT('',(1.625,4.62,1.2));
#31844=CARTESIAN_POINT('Origin',(5.9,4.15,1.1893933982822));
#31845=CARTESIAN_POINT('',(6.37,4.15,1.2));
#31846=CARTESIAN_POINT('',(6.4212132034356,4.15,1.1787867965644));
#31847=CARTESIAN_POINT('',(6.37,4.15,1.2));
#31848=CARTESIAN_POINT('Origin',(5.9,4.15,1.1787867965644));
#31849=CARTESIAN_POINT('Origin',(5.9,4.15,1.2));
#31850=CARTESIAN_POINT('Origin',(6.3956066017178,-1.1875,1.1893933982822));
#31851=CARTESIAN_POINT('',(6.37,-4.15,1.2));
#31852=CARTESIAN_POINT('',(6.4212132034356,-4.15,1.1787867965644));
#31853=CARTESIAN_POINT('',(6.37,-4.15,1.2));
#31854=CARTESIAN_POINT('',(6.4212132034356,-1.1875,1.1787867965644));
#31855=CARTESIAN_POINT('',(6.37,-1.1875,1.2));
#31856=CARTESIAN_POINT('Origin',(5.9,-4.15,1.1893933982822));
#31857=CARTESIAN_POINT('',(5.9,-4.62,1.2));
#31858=CARTESIAN_POINT('',(5.9,-4.6712132034356,1.1787867965644));
#31859=CARTESIAN_POINT('',(5.9,-4.62,1.2));
#31860=CARTESIAN_POINT('Origin',(5.9,-4.15,1.1787867965644));
#31861=CARTESIAN_POINT('Origin',(5.9,-4.15,1.2));
#31862=CARTESIAN_POINT('Origin',(-1.625,-4.6456066017178,1.1893933982822));
#31863=CARTESIAN_POINT('',(-1.625,-4.6712132034356,1.1787867965644));
#31864=CARTESIAN_POINT('',(-1.625,-4.62,1.2));
#31865=CARTESIAN_POINT('Origin',(6.45,-2.375,1.15));
#31866=CARTESIAN_POINT('',(6.4787867965644,-4.15,1.1212132034356));
#31867=CARTESIAN_POINT('',(6.4,-4.15,1.2));
#31868=CARTESIAN_POINT('',(6.4787867965644,4.15,1.1212132034356));
#31869=CARTESIAN_POINT('',(6.4787867965644,-3.5625,1.1212132034356));
#31870=CARTESIAN_POINT('',(6.4,4.15,1.2));
#31871=CARTESIAN_POINT('Origin',(5.9,-4.15,1.15));
#31872=CARTESIAN_POINT('',(5.9,-4.7287867965644,1.1212132034356));
#31873=CARTESIAN_POINT('',(5.9,-4.65,1.2));
#31874=CARTESIAN_POINT('Origin',(5.9,-4.15,1.1212132034356));
#31875=CARTESIAN_POINT('Origin',(-3.25,-4.7,1.15));
#31876=CARTESIAN_POINT('',(-5.9,-4.7287867965644,1.1212132034356));
#31877=CARTESIAN_POINT('',(-5.9,-4.75,1.1));
#31878=CARTESIAN_POINT('',(-4.875,-4.7287867965644,1.1212132034356));
#31879=CARTESIAN_POINT('Origin',(-5.9,-4.15,1.15));
#31880=CARTESIAN_POINT('',(-6.4787867965644,-4.15,1.1212132034356));
#31881=CARTESIAN_POINT('',(-6.4,-4.15,1.2));
#31882=CARTESIAN_POINT('Origin',(-5.9,-4.15,1.1212132034356));
#31883=CARTESIAN_POINT('Origin',(0.,0.,1.2));
#31884=CARTESIAN_POINT('',(-4.92,-3.75,1.2));
#31885=CARTESIAN_POINT('Origin',(-5.5,-3.75,1.2));
#31886=CARTESIAN_POINT('',(-4.92,3.9,1.2));
#31887=CARTESIAN_POINT('Origin',(-5.5,3.9,1.2));
#31888=CARTESIAN_POINT('',(-4.21666666666667,2.3,1.2));
#31889=CARTESIAN_POINT('Origin',(-4.5,2.3,1.2));
#31890=CARTESIAN_POINT('',(0.283333333333333,2.3,1.2));
#31891=CARTESIAN_POINT('Origin',(0.,2.3,1.2));
#31892=CARTESIAN_POINT('',(4.78333333333333,2.3,1.2));
#31893=CARTESIAN_POINT('Origin',(4.5,2.3,1.2));
#31894=CARTESIAN_POINT('',(6.08,3.9,1.2));
#31895=CARTESIAN_POINT('Origin',(5.5,3.9,1.2));
#31896=CARTESIAN_POINT('',(6.08,-3.75,1.2));
#31897=CARTESIAN_POINT('Origin',(5.5,-3.75,1.2));
#31898=CARTESIAN_POINT('Origin',(-5.9,-4.15,1.0956066017178));
#31899=CARTESIAN_POINT('',(-5.9,-4.75,1.07));
#31900=CARTESIAN_POINT('',(-5.9,-4.75,1.07));
#31901=CARTESIAN_POINT('',(-6.5,-4.15,1.07));
#31902=CARTESIAN_POINT('',(-6.4787867965644,-4.15,1.1212132034356));
#31903=CARTESIAN_POINT('Origin',(-5.9,-4.15,1.07));
#31904=CARTESIAN_POINT('Origin',(-4.875,-4.7393933982822,1.0956066017178));
#31905=CARTESIAN_POINT('',(5.9,-4.75,1.07));
#31906=CARTESIAN_POINT('',(5.9,-4.75,1.07));
#31907=CARTESIAN_POINT('',(-4.875,-4.75,1.07));
#31908=CARTESIAN_POINT('Origin',(5.9,-4.15,1.0956066017178));
#31909=CARTESIAN_POINT('',(6.5,-4.15,1.07));
#31910=CARTESIAN_POINT('',(6.5,-4.15,1.07));
#31911=CARTESIAN_POINT('Origin',(5.9,-4.15,1.07));
#31912=CARTESIAN_POINT('Origin',(6.4893933982822,-3.5625,1.0956066017178));
#31913=CARTESIAN_POINT('',(6.5,4.15,1.07));
#31914=CARTESIAN_POINT('',(6.5,4.15,1.07));
#31915=CARTESIAN_POINT('',(6.5,-3.5625,1.07));
#31916=CARTESIAN_POINT('Origin',(5.9,4.15,1.0956066017178));
#31917=CARTESIAN_POINT('',(5.9,4.75,1.07));
#31918=CARTESIAN_POINT('',(5.9,4.7287867965644,1.1212132034356));
#31919=CARTESIAN_POINT('',(5.9,4.75,1.07));
#31920=CARTESIAN_POINT('Origin',(5.9,4.15,1.1212132034356));
#31921=CARTESIAN_POINT('Origin',(5.9,4.15,1.07));
#31922=CARTESIAN_POINT('Origin',(4.875,4.7393933982822,1.0956066017178));
#31923=CARTESIAN_POINT('',(-5.9,4.75,1.07));
#31924=CARTESIAN_POINT('',(-5.9,4.7287867965644,1.1212132034356));
#31925=CARTESIAN_POINT('',(-5.9,4.75,1.07));
#31926=CARTESIAN_POINT('',(4.875,4.7287867965644,1.1212132034356));
#31927=CARTESIAN_POINT('',(4.875,4.75,1.07));
#31928=CARTESIAN_POINT('Origin',(-5.9,4.15,1.0956066017178));
#31929=CARTESIAN_POINT('',(-6.5,4.15,1.07));
#31930=CARTESIAN_POINT('',(-6.4787867965644,4.15,1.1212132034356));
#31931=CARTESIAN_POINT('',(-6.5,4.15,1.07));
#31932=CARTESIAN_POINT('Origin',(-5.9,4.15,1.1212132034356));
#31933=CARTESIAN_POINT('Origin',(-5.9,4.15,1.07));
#31934=CARTESIAN_POINT('Origin',(-6.4893933982822,3.5625,1.0956066017178));
#31935=CARTESIAN_POINT('',(-6.4787867965644,3.5625,1.1212132034356));
#31936=CARTESIAN_POINT('',(-6.5,3.5625,1.07));
#31937=CARTESIAN_POINT('Origin',(6.5,-4.75,0.));
#31938=CARTESIAN_POINT('',(6.5,-4.15,0.0800000000000016));
#31939=CARTESIAN_POINT('',(6.5,-4.15,0.));
#31940=CARTESIAN_POINT('',(6.5,4.15,0.0800000000000016));
#31941=CARTESIAN_POINT('',(6.5,-3.5625,0.0800000000000016));
#31942=CARTESIAN_POINT('',(6.5,4.15,0.));
#31943=CARTESIAN_POINT('Origin',(5.9,-4.15,0.));
#31944=CARTESIAN_POINT('',(5.9,-4.75,0.08));
#31945=CARTESIAN_POINT('',(5.9,-4.75,0.));
#31946=CARTESIAN_POINT('Origin',(5.9,-4.15,0.08));
#31947=CARTESIAN_POINT('Origin',(-6.5,-4.75,0.));
#31948=CARTESIAN_POINT('',(-5.9,-4.75,0.0800000000000016));
#31949=CARTESIAN_POINT('',(-5.9,-4.75,0.));
#31950=CARTESIAN_POINT('',(-4.875,-4.75,0.0800000000000016));
#31951=CARTESIAN_POINT('Origin',(-5.9,-4.15,0.));
#31952=CARTESIAN_POINT('',(-6.5,-4.15,0.08));
#31953=CARTESIAN_POINT('',(-6.5,-4.15,0.));
#31954=CARTESIAN_POINT('Origin',(-5.9,-4.15,0.08));
#31955=CARTESIAN_POINT('Origin',(3.25,4.7,1.15));
#31956=CARTESIAN_POINT('',(5.9,4.65,1.2));
#31957=CARTESIAN_POINT('',(-5.9,4.65,1.2));
#31958=CARTESIAN_POINT('Origin',(-5.9,4.15,1.15));
#31959=CARTESIAN_POINT('',(-6.4,4.15,1.2));
#31960=CARTESIAN_POINT('Origin',(-6.45,2.375,1.15));
#31961=CARTESIAN_POINT('Origin',(6.4456066017178,-1.1875,0.0106066017177982));
#31962=CARTESIAN_POINT('',(6.42,4.15,0.));
#31963=CARTESIAN_POINT('',(6.4712132034356,4.15,0.0212132034355961));
#31964=CARTESIAN_POINT('',(6.42,4.15,0.));
#31965=CARTESIAN_POINT('',(6.4712132034356,-4.15,0.0212132034355961));
#31966=CARTESIAN_POINT('',(6.4712132034356,-1.1875,0.0212132034355963));
#31967=CARTESIAN_POINT('',(6.42,-4.15,0.));
#31968=CARTESIAN_POINT('',(6.4712132034356,-4.15,0.0212132034355961));
#31969=CARTESIAN_POINT('',(6.42,-1.1875,0.));
#31970=CARTESIAN_POINT('Origin',(5.9,4.15,0.0106066017177981));
#31971=CARTESIAN_POINT('',(5.9,4.67,0.));
#31972=CARTESIAN_POINT('',(5.9,4.7212132034356,0.0212132034355954));
#31973=CARTESIAN_POINT('',(5.9,4.67,0.));
#31974=CARTESIAN_POINT('Origin',(5.9,4.15,0.0212132034355961));
#31975=CARTESIAN_POINT('Origin',(5.9,4.15,0.));
#31976=CARTESIAN_POINT('Origin',(1.625,4.6956066017178,0.0106066017177982));
#31977=CARTESIAN_POINT('',(-5.9,4.67,0.));
#31978=CARTESIAN_POINT('',(-5.9,4.7212132034356,0.0212132034355962));
#31979=CARTESIAN_POINT('',(-5.9,4.67,0.));
#31980=CARTESIAN_POINT('',(1.625,4.7212132034356,0.0212132034355964));
#31981=CARTESIAN_POINT('',(1.625,4.67,0.));
#31982=CARTESIAN_POINT('Origin',(-5.9,4.15,0.0106066017177981));
#31983=CARTESIAN_POINT('',(-6.42,4.15,0.));
#31984=CARTESIAN_POINT('',(-6.4712132034356,4.15,0.0212132034355954));
#31985=CARTESIAN_POINT('',(-6.42,4.15,0.));
#31986=CARTESIAN_POINT('Origin',(-5.9,4.15,0.0212132034355961));
#31987=CARTESIAN_POINT('Origin',(-5.9,4.15,0.));
#31988=CARTESIAN_POINT('Origin',(-6.4456066017178,1.1875,0.0106066017177982));
#31989=CARTESIAN_POINT('',(-6.42,-4.15,0.));
#31990=CARTESIAN_POINT('',(-6.4712132034356,-4.15,0.0212132034355961));
#31991=CARTESIAN_POINT('',(-6.42,-4.15,0.));
#31992=CARTESIAN_POINT('',(-6.4712132034356,1.1875,0.0212132034355963));
#31993=CARTESIAN_POINT('',(-6.42,1.1875,0.));
#31994=CARTESIAN_POINT('Origin',(-5.9,-4.15,0.0106066017177981));
#31995=CARTESIAN_POINT('',(-5.9,-4.67,0.));
#31996=CARTESIAN_POINT('',(-5.9,-4.7212132034356,0.0212132034355954));
#31997=CARTESIAN_POINT('',(-5.9,-4.67,0.));
#31998=CARTESIAN_POINT('Origin',(-5.9,-4.15,0.0212132034355961));
#31999=CARTESIAN_POINT('Origin',(-5.9,-4.15,0.));
#32000=CARTESIAN_POINT('Origin',(-1.625,-4.6956066017178,0.0106066017177982));
#32001=CARTESIAN_POINT('',(5.9,-4.67,0.));
#32002=CARTESIAN_POINT('',(5.9,-4.7212132034356,0.0212132034355962));
#32003=CARTESIAN_POINT('',(5.9,-4.67,0.));
#32004=CARTESIAN_POINT('',(-1.625,-4.7212132034356,0.0212132034355964));
#32005=CARTESIAN_POINT('',(-1.625,-4.67,0.));
#32006=CARTESIAN_POINT('Origin',(5.9,-4.15,0.0106066017177981));
#32007=CARTESIAN_POINT('Origin',(5.9,-4.15,0.0212132034355961));
#32008=CARTESIAN_POINT('Origin',(5.9,-4.15,0.));
#32009=CARTESIAN_POINT('Origin',(-5.9,-4.15,0.025));
#32010=CARTESIAN_POINT('',(-5.9,-4.72878679656441,0.0287867965644042));
#32011=CARTESIAN_POINT('',(-5.9,-4.7,0.));
#32012=CARTESIAN_POINT('',(-6.4787867965644,-4.15,0.0287867965644041));
#32013=CARTESIAN_POINT('Origin',(-5.9,-4.15,0.0287867965644037));
#32014=CARTESIAN_POINT('',(-6.45,-4.15,0.));
#32015=CARTESIAN_POINT('Origin',(-3.25,-4.725,0.025));
#32016=CARTESIAN_POINT('',(5.9,-4.7287867965644,0.0287867965644041));
#32017=CARTESIAN_POINT('',(5.9,-4.7,0.));
#32018=CARTESIAN_POINT('',(-4.875,-4.7287867965644,0.0287867965644046));
#32019=CARTESIAN_POINT('Origin',(5.9,-4.15,0.025));
#32020=CARTESIAN_POINT('',(6.4787867965644,-4.15,0.0287867965644044));
#32021=CARTESIAN_POINT('',(6.5,-4.15,0.05));
#32022=CARTESIAN_POINT('Origin',(5.9,-4.15,0.0287867965644037));
#32023=CARTESIAN_POINT('Origin',(6.475,-2.375,0.025));
#32024=CARTESIAN_POINT('',(6.4787867965644,4.15,0.0287867965644044));
#32025=CARTESIAN_POINT('',(6.45,4.15,0.));
#32026=CARTESIAN_POINT('',(6.4787867965644,-3.5625,0.0287867965644046));
#32027=CARTESIAN_POINT('Origin',(0.,0.,0.));
#32028=CARTESIAN_POINT('',(-5.03,2.3,0.));
#32029=CARTESIAN_POINT('Origin',(-4.5,2.3,0.));
#32030=CARTESIAN_POINT('',(3.97,2.3,0.));
#32031=CARTESIAN_POINT('Origin',(4.5,2.3,0.));
#32032=CARTESIAN_POINT('',(5.16166666666667,3.9,0.));
#32033=CARTESIAN_POINT('Origin',(5.5,3.9,0.));
#32034=CARTESIAN_POINT('',(-5.83833333333333,3.9,0.));
#32035=CARTESIAN_POINT('Origin',(-5.5,3.9,0.));
#32036=CARTESIAN_POINT('',(5.16166666666667,-3.75,0.));
#32037=CARTESIAN_POINT('Origin',(5.5,-3.75,0.));
#32038=CARTESIAN_POINT('',(-5.83833333333333,-3.75,0.));
#32039=CARTESIAN_POINT('Origin',(-5.5,-3.75,0.));
#32040=CARTESIAN_POINT('',(-0.53,2.3,0.));
#32041=CARTESIAN_POINT('Origin',(0.,2.3,0.));
#32042=CARTESIAN_POINT('Origin',(6.4893933982822,-3.5625,0.0543933982822031));
#32043=CARTESIAN_POINT('',(6.5,-4.15,0.0800000000000016));
#32044=CARTESIAN_POINT('',(6.4787867965644,4.15,0.0287867965644044));
#32045=CARTESIAN_POINT('Origin',(5.9,-4.15,0.0543933982822019));
#32046=CARTESIAN_POINT('',(5.9,-4.75,0.08));
#32047=CARTESIAN_POINT('Origin',(-4.875,-4.7393933982822,0.0543933982822031));
#32048=CARTESIAN_POINT('',(-5.9,-4.75,0.0800000000000016));
#32049=CARTESIAN_POINT('Origin',(-5.9,-4.15,0.0543933982822019));
#32050=CARTESIAN_POINT('',(-6.5,-4.15,0.08));
#32051=CARTESIAN_POINT('Origin',(-6.4893933982822,3.5625,0.0543933982822031));
#32052=CARTESIAN_POINT('',(-6.5,4.15,0.0800000000000016));
#32053=CARTESIAN_POINT('',(-6.47878679656441,4.15,0.0287867965644042));
#32054=CARTESIAN_POINT('',(-6.5,4.15,0.0800000000000016));
#32055=CARTESIAN_POINT('',(-6.4787867965644,3.5625,0.0287867965644046));
#32056=CARTESIAN_POINT('',(-6.5,3.5625,0.0800000000000016));
#32057=CARTESIAN_POINT('Origin',(-5.9,4.15,0.0543933982822019));
#32058=CARTESIAN_POINT('',(-5.9,4.75,0.08));
#32059=CARTESIAN_POINT('',(-5.9,4.7287867965644,0.0287867965644041));
#32060=CARTESIAN_POINT('',(-5.9,4.75,0.08));
#32061=CARTESIAN_POINT('Origin',(-5.9,4.15,0.0287867965644037));
#32062=CARTESIAN_POINT('Origin',(-5.9,4.15,0.08));
#32063=CARTESIAN_POINT('Origin',(4.875,4.7393933982822,0.0543933982822031));
#32064=CARTESIAN_POINT('',(5.9,4.75,0.0800000000000016));
#32065=CARTESIAN_POINT('',(5.9,4.72878679656441,0.0287867965644042));
#32066=CARTESIAN_POINT('',(5.9,4.75,0.0800000000000016));
#32067=CARTESIAN_POINT('',(4.875,4.7287867965644,0.0287867965644046));
#32068=CARTESIAN_POINT('',(4.875,4.75,0.0800000000000016));
#32069=CARTESIAN_POINT('Origin',(5.9,4.15,0.0543933982822019));
#32070=CARTESIAN_POINT('Origin',(5.9,4.15,0.0287867965644037));
#32071=CARTESIAN_POINT('Origin',(5.9,4.15,0.08));
#32072=CARTESIAN_POINT('Origin',(-5.9,4.15,0.025));
#32073=CARTESIAN_POINT('',(-6.45,4.15,0.));
#32074=CARTESIAN_POINT('',(-5.9,4.7,0.));
#32075=CARTESIAN_POINT('Origin',(3.25,4.725,0.025));
#32076=CARTESIAN_POINT('',(5.9,4.7,0.));
#32077=CARTESIAN_POINT('Origin',(5.9,4.15,0.025));
#32078=CARTESIAN_POINT('Origin',(-5.5,-3.75,1.185));
#32079=CARTESIAN_POINT('',(-4.95,-3.75,1.17));
#32080=CARTESIAN_POINT('',(-4.935,-3.75,1.185));
#32081=CARTESIAN_POINT('',(-6.05,-3.75,1.17));
#32082=CARTESIAN_POINT('Origin',(-5.5,-3.75,1.17));
#32083=CARTESIAN_POINT('Origin',(-5.5,-3.75,1.17));
#32084=CARTESIAN_POINT('Origin',(-5.5,-3.75,0.875));
#32085=CARTESIAN_POINT('',(-6.05,-3.75,0.55));
#32086=CARTESIAN_POINT('Origin',(-5.5,-3.75,0.55));
#32087=CARTESIAN_POINT('',(-6.05,-3.75,0.875));
#32088=CARTESIAN_POINT('Origin',(5.5,-3.75,1.185));
#32089=CARTESIAN_POINT('',(6.05,-3.75,1.17));
#32090=CARTESIAN_POINT('',(6.065,-3.75,1.185));
#32091=CARTESIAN_POINT('',(4.95,-3.75,1.17));
#32092=CARTESIAN_POINT('Origin',(5.5,-3.75,1.17));
#32093=CARTESIAN_POINT('Origin',(5.5,-3.75,1.17));
#32094=CARTESIAN_POINT('Origin',(5.5,-3.75,0.875));
#32095=CARTESIAN_POINT('',(4.95,-3.75,0.55));
#32096=CARTESIAN_POINT('Origin',(5.5,-3.75,0.55));
#32097=CARTESIAN_POINT('',(4.95,-3.75,0.875));
#32098=CARTESIAN_POINT('Origin',(-5.5,3.9,1.185));
#32099=CARTESIAN_POINT('',(-4.95,3.9,1.17));
#32100=CARTESIAN_POINT('',(-4.935,3.9,1.185));
#32101=CARTESIAN_POINT('',(-6.05,3.9,1.17));
#32102=CARTESIAN_POINT('Origin',(-5.5,3.9,1.17));
#32103=CARTESIAN_POINT('Origin',(-5.5,3.9,1.17));
#32104=CARTESIAN_POINT('Origin',(-5.5,3.9,0.875));
#32105=CARTESIAN_POINT('',(-6.05,3.9,0.55));
#32106=CARTESIAN_POINT('Origin',(-5.5,3.9,0.55));
#32107=CARTESIAN_POINT('',(-6.05,3.9,0.875));
#32108=CARTESIAN_POINT('Origin',(5.5,3.9,1.185));
#32109=CARTESIAN_POINT('',(6.05,3.9,1.17));
#32110=CARTESIAN_POINT('',(6.065,3.9,1.185));
#32111=CARTESIAN_POINT('',(4.95,3.9,1.17));
#32112=CARTESIAN_POINT('Origin',(5.5,3.9,1.17));
#32113=CARTESIAN_POINT('Origin',(5.5,3.9,1.17));
#32114=CARTESIAN_POINT('Origin',(5.5,3.9,0.875));
#32115=CARTESIAN_POINT('',(4.95,3.9,0.55));
#32116=CARTESIAN_POINT('Origin',(5.5,3.9,0.55));
#32117=CARTESIAN_POINT('',(4.95,3.9,0.875));
#32118=CARTESIAN_POINT('Origin',(-4.5,2.3,0.015));
#32119=CARTESIAN_POINT('',(-5.,2.3,0.03));
#32120=CARTESIAN_POINT('',(-5.015,2.3,0.015));
#32121=CARTESIAN_POINT('',(-4.,2.3,0.03));
#32122=CARTESIAN_POINT('Origin',(-4.5,2.3,0.03));
#32123=CARTESIAN_POINT('Origin',(-4.5,2.3,0.03));
#32124=CARTESIAN_POINT('Origin',(-4.5,2.3,0.275));
#32125=CARTESIAN_POINT('',(-4.,2.3,0.55));
#32126=CARTESIAN_POINT('Origin',(-4.5,2.3,0.55));
#32127=CARTESIAN_POINT('',(-4.,2.3,0.275));
#32128=CARTESIAN_POINT('Origin',(0.,2.3,0.015));
#32129=CARTESIAN_POINT('',(-0.5,2.3,0.03));
#32130=CARTESIAN_POINT('',(-0.515,2.3,0.015));
#32131=CARTESIAN_POINT('',(0.5,2.3,0.03));
#32132=CARTESIAN_POINT('Origin',(0.,2.3,0.03));
#32133=CARTESIAN_POINT('Origin',(0.,2.3,0.03));
#32134=CARTESIAN_POINT('Origin',(0.,2.3,0.275));
#32135=CARTESIAN_POINT('',(0.5,2.3,0.55));
#32136=CARTESIAN_POINT('Origin',(0.,2.3,0.55));
#32137=CARTESIAN_POINT('',(0.5,2.3,0.275));
#32138=CARTESIAN_POINT('Origin',(4.5,2.3,0.015));
#32139=CARTESIAN_POINT('',(4.,2.3,0.03));
#32140=CARTESIAN_POINT('',(3.985,2.3,0.015));
#32141=CARTESIAN_POINT('',(5.,2.3,0.03));
#32142=CARTESIAN_POINT('Origin',(4.5,2.3,0.03));
#32143=CARTESIAN_POINT('Origin',(4.5,2.3,0.03));
#32144=CARTESIAN_POINT('Origin',(4.5,2.3,0.275));
#32145=CARTESIAN_POINT('',(5.,2.3,0.55));
#32146=CARTESIAN_POINT('Origin',(4.5,2.3,0.55));
#32147=CARTESIAN_POINT('',(5.,2.3,0.275));
#32148=CARTESIAN_POINT('Origin',(4.5,2.3,1.2125));
#32149=CARTESIAN_POINT('',(4.775,2.3,1.175));
#32150=CARTESIAN_POINT('',(4.7875,2.3,1.2125));
#32151=CARTESIAN_POINT('Origin',(4.5,2.3,1.175));
#32152=CARTESIAN_POINT('Origin',(4.5,2.3,0.875));
#32153=CARTESIAN_POINT('',(4.775,2.3,0.575));
#32154=CARTESIAN_POINT('',(4.775,2.3,0.875));
#32155=CARTESIAN_POINT('Origin',(4.5,2.3,0.575));
#32156=CARTESIAN_POINT('Origin',(4.5,2.3,0.5625));
#32157=CARTESIAN_POINT('',(4.8,2.3,0.55));
#32158=CARTESIAN_POINT('',(4.7875,2.3,0.5625));
#32159=CARTESIAN_POINT('Origin',(4.5,2.3,0.55));
#32160=CARTESIAN_POINT('Origin',(4.,2.3,0.55));
#32161=CARTESIAN_POINT('Origin',(0.,2.3,1.2125));
#32162=CARTESIAN_POINT('',(0.275,2.3,1.175));
#32163=CARTESIAN_POINT('',(0.2875,2.3,1.2125));
#32164=CARTESIAN_POINT('Origin',(0.,2.3,1.175));
#32165=CARTESIAN_POINT('Origin',(0.,2.3,0.875));
#32166=CARTESIAN_POINT('',(0.275,2.3,0.575));
#32167=CARTESIAN_POINT('',(0.275,2.3,0.875));
#32168=CARTESIAN_POINT('Origin',(0.,2.3,0.575));
#32169=CARTESIAN_POINT('Origin',(0.,2.3,0.5625));
#32170=CARTESIAN_POINT('',(0.3,2.3,0.55));
#32171=CARTESIAN_POINT('',(0.2875,2.3,0.5625));
#32172=CARTESIAN_POINT('Origin',(0.,2.3,0.55));
#32173=CARTESIAN_POINT('Origin',(-0.5,2.3,0.55));
#32174=CARTESIAN_POINT('Origin',(-4.5,2.3,1.2125));
#32175=CARTESIAN_POINT('',(-4.225,2.3,1.175));
#32176=CARTESIAN_POINT('',(-4.2125,2.3,1.2125));
#32177=CARTESIAN_POINT('Origin',(-4.5,2.3,1.175));
#32178=CARTESIAN_POINT('Origin',(-4.5,2.3,0.875));
#32179=CARTESIAN_POINT('',(-4.225,2.3,0.575));
#32180=CARTESIAN_POINT('',(-4.225,2.3,0.875));
#32181=CARTESIAN_POINT('Origin',(-4.5,2.3,0.575));
#32182=CARTESIAN_POINT('Origin',(-4.5,2.3,0.5625));
#32183=CARTESIAN_POINT('',(-4.2,2.3,0.55));
#32184=CARTESIAN_POINT('',(-4.2125,2.3,0.5625));
#32185=CARTESIAN_POINT('Origin',(-4.5,2.3,0.55));
#32186=CARTESIAN_POINT('Origin',(-5.,2.3,0.55));
#32187=CARTESIAN_POINT('Origin',(5.5,3.9,-0.0125));
#32188=CARTESIAN_POINT('',(5.17,3.9,0.0249999999999998));
#32189=CARTESIAN_POINT('',(5.1575,3.9,-0.0125));
#32190=CARTESIAN_POINT('Origin',(5.5,3.9,0.0249999999999999));
#32191=CARTESIAN_POINT('Origin',(5.5,3.9,0.275));
#32192=CARTESIAN_POINT('',(5.17,3.9,0.525));
#32193=CARTESIAN_POINT('',(5.17,3.9,0.275));
#32194=CARTESIAN_POINT('Origin',(5.5,3.9,0.525));
#32195=CARTESIAN_POINT('Origin',(5.5,3.9,0.5375));
#32196=CARTESIAN_POINT('',(5.145,3.9,0.55));
#32197=CARTESIAN_POINT('',(5.1575,3.9,0.5375));
#32198=CARTESIAN_POINT('Origin',(5.5,3.9,0.55));
#32199=CARTESIAN_POINT('Origin',(6.05,3.9,0.55));
#32200=CARTESIAN_POINT('Origin',(-5.5,3.9,-0.0125));
#32201=CARTESIAN_POINT('',(-5.83,3.9,0.0249999999999998));
#32202=CARTESIAN_POINT('',(-5.8425,3.9,-0.0125));
#32203=CARTESIAN_POINT('Origin',(-5.5,3.9,0.0249999999999999));
#32204=CARTESIAN_POINT('Origin',(-5.5,3.9,0.275));
#32205=CARTESIAN_POINT('',(-5.83,3.9,0.525));
#32206=CARTESIAN_POINT('',(-5.83,3.9,0.275));
#32207=CARTESIAN_POINT('Origin',(-5.5,3.9,0.525));
#32208=CARTESIAN_POINT('Origin',(-5.5,3.9,0.5375));
#32209=CARTESIAN_POINT('',(-5.855,3.9,0.55));
#32210=CARTESIAN_POINT('',(-5.8425,3.9,0.5375));
#32211=CARTESIAN_POINT('Origin',(-5.5,3.9,0.55));
#32212=CARTESIAN_POINT('Origin',(-4.95,3.9,0.55));
#32213=CARTESIAN_POINT('Origin',(5.5,-3.75,-0.0125));
#32214=CARTESIAN_POINT('',(5.17,-3.75,0.0249999999999998));
#32215=CARTESIAN_POINT('',(5.1575,-3.75,-0.0125));
#32216=CARTESIAN_POINT('Origin',(5.5,-3.75,0.0249999999999999));
#32217=CARTESIAN_POINT('Origin',(5.5,-3.75,0.275));
#32218=CARTESIAN_POINT('',(5.17,-3.75,0.525));
#32219=CARTESIAN_POINT('',(5.17,-3.75,0.275));
#32220=CARTESIAN_POINT('Origin',(5.5,-3.75,0.525));
#32221=CARTESIAN_POINT('Origin',(5.5,-3.75,0.5375));
#32222=CARTESIAN_POINT('',(5.145,-3.75,0.55));
#32223=CARTESIAN_POINT('',(5.1575,-3.75,0.5375));
#32224=CARTESIAN_POINT('Origin',(5.5,-3.75,0.55));
#32225=CARTESIAN_POINT('Origin',(6.05,-3.75,0.55));
#32226=CARTESIAN_POINT('Origin',(-5.5,-3.75,-0.0125));
#32227=CARTESIAN_POINT('',(-5.83,-3.75,0.0249999999999998));
#32228=CARTESIAN_POINT('',(-5.8425,-3.75,-0.0125));
#32229=CARTESIAN_POINT('Origin',(-5.5,-3.75,0.0249999999999999));
#32230=CARTESIAN_POINT('Origin',(-5.5,-3.75,0.275));
#32231=CARTESIAN_POINT('',(-5.83,-3.75,0.525));
#32232=CARTESIAN_POINT('',(-5.83,-3.75,0.275));
#32233=CARTESIAN_POINT('Origin',(-5.5,-3.75,0.525));
#32234=CARTESIAN_POINT('Origin',(-5.5,-3.75,0.5375));
#32235=CARTESIAN_POINT('',(-5.855,-3.75,0.55));
#32236=CARTESIAN_POINT('',(-5.8425,-3.75,0.5375));
#32237=CARTESIAN_POINT('Origin',(-5.5,-3.75,0.55));
#32238=CARTESIAN_POINT('Origin',(-4.95,-3.75,0.55));
#32239=CARTESIAN_POINT('Origin',(-6.475,2.375,0.025));
#32240=CARTESIAN_POINT('Origin',(5.9,4.15,1.15));
#32241=CARTESIAN_POINT('Origin',(-6.5,4.75,0.));
#32242=CARTESIAN_POINT('',(-6.5,4.15,0.));
#32243=CARTESIAN_POINT('Origin',(5.9,4.15,0.));
#32244=CARTESIAN_POINT('',(5.9,4.75,0.));
#32245=CARTESIAN_POINT('Origin',(-5.9,4.15,0.));
#32246=CARTESIAN_POINT('',(-5.9,4.75,0.));
#32247=CARTESIAN_POINT('Origin',(6.5,4.75,0.));
#32248=CARTESIAN_POINT('',(0.,0.,0.));
#32249=CARTESIAN_POINT('Origin',(1.55,1.4106066017178,1.2843933982822));
#32250=CARTESIAN_POINT('',(6.09,1.4,1.31));
#32251=CARTESIAN_POINT('',(-6.09,1.4,1.31));
#32252=CARTESIAN_POINT('',(1.55,1.4,1.31));
#32253=CARTESIAN_POINT('',(-6.1412132034356,1.4212132034356,1.2587867965644));
#32254=CARTESIAN_POINT('',(-6.09,1.4,1.31));
#32255=CARTESIAN_POINT('',(6.1412132034356,1.4212132034356,1.2587867965644));
#32256=CARTESIAN_POINT('',(1.55,1.4212132034356,1.2587867965644));
#32257=CARTESIAN_POINT('',(6.1412132034356,1.4212132034356,1.2587867965644));
#32258=CARTESIAN_POINT('Origin',(-6.1156066017178,1.4106066017178,6.825));
#32259=CARTESIAN_POINT('',(-6.09,1.4,15.6));
#32260=CARTESIAN_POINT('',(-6.09,1.4,6.825));
#32261=CARTESIAN_POINT('',(-6.1412132034356,1.4212132034356,15.6));
#32262=CARTESIAN_POINT('',(-6.09,1.4,15.6));
#32263=CARTESIAN_POINT('',(-6.1412132034356,1.4212132034356,6.825));
#32264=CARTESIAN_POINT('Origin',(-5.6,1.4106066017178,15.6));
#32265=CARTESIAN_POINT('',(-5.6,1.4,16.09));
#32266=CARTESIAN_POINT('',(-5.6,1.4212132034356,16.1412132034356));
#32267=CARTESIAN_POINT('',(-5.6,1.4,16.09));
#32268=CARTESIAN_POINT('Origin',(-5.6,1.4212132034356,15.6));
#32269=CARTESIAN_POINT('Origin',(-5.6,1.4,15.6));
#32270=CARTESIAN_POINT('Origin',(-1.55,1.4106066017178,16.1156066017178));
#32271=CARTESIAN_POINT('',(5.6,1.4,16.09));
#32272=CARTESIAN_POINT('',(5.6,1.4212132034356,16.1412132034356));
#32273=CARTESIAN_POINT('',(5.6,1.4,16.09));
#32274=CARTESIAN_POINT('',(-1.55,1.4212132034356,16.1412132034356));
#32275=CARTESIAN_POINT('',(-1.55,1.4,16.09));
#32276=CARTESIAN_POINT('Origin',(5.6,1.4106066017178,15.6));
#32277=CARTESIAN_POINT('',(6.09,1.4,15.6));
#32278=CARTESIAN_POINT('',(6.1412132034356,1.42121320343559,15.6));
#32279=CARTESIAN_POINT('',(6.09,1.4,15.6));
#32280=CARTESIAN_POINT('Origin',(5.6,1.4212132034356,15.6));
#32281=CARTESIAN_POINT('Origin',(5.6,1.4,15.6));
#32282=CARTESIAN_POINT('Origin',(6.1156066017178,1.4106066017178,10.575));
#32283=CARTESIAN_POINT('',(6.1412132034356,1.4212132034356,10.575));
#32284=CARTESIAN_POINT('',(6.09,1.4,10.575));
#32285=CARTESIAN_POINT('Origin',(5.6,1.44,15.6));
#32286=CARTESIAN_POINT('',(6.1787867965644,1.4587867965644,15.6));
#32287=CARTESIAN_POINT('',(6.2,1.48,15.6));
#32288=CARTESIAN_POINT('',(5.6,1.4587867965644,16.1787867965644));
#32289=CARTESIAN_POINT('Origin',(5.6,1.4587867965644,15.6));
#32290=CARTESIAN_POINT('',(5.6,1.48,16.2));
#32291=CARTESIAN_POINT('Origin',(6.16,1.44,12.45));
#32292=CARTESIAN_POINT('',(6.1787867965644,1.4587867965644,1.2212132034356));
#32293=CARTESIAN_POINT('',(6.12,1.4,1.28));
#32294=CARTESIAN_POINT('',(6.1787867965644,1.4587867965644,14.325));
#32295=CARTESIAN_POINT('Origin',(3.1,1.44,1.24));
#32296=CARTESIAN_POINT('',(-6.1787867965644,1.4587867965644,1.2212132034356));
#32297=CARTESIAN_POINT('',(-6.12,1.4,1.28));
#32298=CARTESIAN_POINT('',(4.65,1.4587867965644,1.2212132034356));
#32299=CARTESIAN_POINT('Origin',(0.,1.4,8.7));
#32300=CARTESIAN_POINT('',(3.33,1.4,8.5));
#32301=CARTESIAN_POINT('Origin',(0.,1.4,8.5));
#32302=CARTESIAN_POINT('',(-4.2,1.4,8.5));
#32303=CARTESIAN_POINT('Origin',(-4.4,1.4,8.5));
#32304=CARTESIAN_POINT('',(5.06823591024675,1.4,11.175));
#32305=CARTESIAN_POINT('Origin',(4.63323591024675,1.4,11.175));
#32306=CARTESIAN_POINT('',(0.434999999999999,1.4,3.15));
#32307=CARTESIAN_POINT('Origin',(-9.82779056315751E-16,1.4,3.15));
#32308=CARTESIAN_POINT('',(-4.19823591024675,1.4,11.175));
#32309=CARTESIAN_POINT('Origin',(-4.63323591024675,1.4,11.175));
#32310=CARTESIAN_POINT('',(2.4,1.4,4.68948822334847));
#32311=CARTESIAN_POINT('Origin',(2.2,1.4,4.68948822334847));
#32312=CARTESIAN_POINT('',(2.4,1.4,12.3105117766515));
#32313=CARTESIAN_POINT('Origin',(2.2,1.4,12.3105117766515));
#32314=CARTESIAN_POINT('Origin',(4.65,1.4843933982822,1.2106066017178));
#32315=CARTESIAN_POINT('',(6.185,1.4737867965644,1.215));
#32316=CARTESIAN_POINT('',(5.25345910630655,-0.775151862895448,2.14654089369344));
#32317=CARTESIAN_POINT('',(-6.185,1.4737867965644,1.215));
#32318=CARTESIAN_POINT('',(-5.3780051976814,-0.474470999957732,2.02199480231859));
#32319=CARTESIAN_POINT('',(-6.17,1.51,1.2));
#32320=CARTESIAN_POINT('',(-5.50243230506491,3.12165098291439,0.532432305064926));
#32321=CARTESIAN_POINT('',(6.17,1.51,1.2));
#32322=CARTESIAN_POINT('',(4.65,1.51,1.2));
#32323=CARTESIAN_POINT('',(6.09642135623731,1.6876345596729,1.12642135623731));
#32324=CARTESIAN_POINT('Origin',(6.2,1.4,1.2));
#32325=CARTESIAN_POINT('',(-6.17,3.09,1.2));
#32326=CARTESIAN_POINT('',(-6.17,1.4,1.2));
#32327=CARTESIAN_POINT('',(6.17,3.09,1.2));
#32328=CARTESIAN_POINT('',(4.65,3.09,1.2));
#32329=CARTESIAN_POINT('',(6.17,1.4,1.2));
#32330=CARTESIAN_POINT('',(-4.195,2.3,1.2));
#32331=CARTESIAN_POINT('Origin',(-4.5,2.3,1.2));
#32332=CARTESIAN_POINT('',(0.305,2.3,1.2));
#32333=CARTESIAN_POINT('Origin',(0.,2.3,1.2));
#32334=CARTESIAN_POINT('',(4.805,2.3,1.2));
#32335=CARTESIAN_POINT('Origin',(4.5,2.3,1.2));
#32336=CARTESIAN_POINT('Origin',(-6.185,1.4,1.215));
#32337=CARTESIAN_POINT('',(-6.2,1.51,1.23));
#32338=CARTESIAN_POINT('',(-6.2943363256585,1.73774803682919,1.3243363256585));
#32339=CARTESIAN_POINT('',(-6.2,3.09,1.23));
#32340=CARTESIAN_POINT('',(-6.2,1.4,1.23));
#32341=CARTESIAN_POINT('',(-6.185,3.1262132034356,1.215));
#32342=CARTESIAN_POINT('',(-6.57188789144717,2.19218320878592,1.60188789144716));
#32343=CARTESIAN_POINT('',(-5.22488073927622,0.808280262700718,0.254880739276242));
#32344=CARTESIAN_POINT('Origin',(-6.1893933982822,1.4843933982822,3.075));
#32345=CARTESIAN_POINT('',(-6.1787867965644,1.4587867965644,15.6));
#32346=CARTESIAN_POINT('',(-6.1787867965644,1.4587867965644,3.075));
#32347=CARTESIAN_POINT('',(-6.2,1.51,15.6));
#32348=CARTESIAN_POINT('',(-6.2,1.51,15.6));
#32349=CARTESIAN_POINT('',(-6.2,1.51,3.075));
#32350=CARTESIAN_POINT('Origin',(6.1893933982822,1.4843933982822,14.325));
#32351=CARTESIAN_POINT('',(6.2,1.51,1.23));
#32352=CARTESIAN_POINT('',(7.01287146820574,3.47244532300839,2.04287146820574));
#32353=CARTESIAN_POINT('',(6.2,1.51,15.6));
#32354=CARTESIAN_POINT('',(6.2,1.51,14.325));
#32355=CARTESIAN_POINT('',(6.2,1.51,15.6));
#32356=CARTESIAN_POINT('Origin',(5.6,1.4843933982822,15.6));
#32357=CARTESIAN_POINT('',(5.6,1.51,16.2));
#32358=CARTESIAN_POINT('',(5.6,1.51,16.2));
#32359=CARTESIAN_POINT('Origin',(5.6,1.51,15.6));
#32360=CARTESIAN_POINT('Origin',(-4.65,1.4843933982822,16.1893933982822));
#32361=CARTESIAN_POINT('',(-5.6,1.51,16.2));
#32362=CARTESIAN_POINT('',(-5.6,1.4587867965644,16.1787867965644));
#32363=CARTESIAN_POINT('',(-5.6,1.51,16.2));
#32364=CARTESIAN_POINT('',(-4.65,1.4587867965644,16.1787867965644));
#32365=CARTESIAN_POINT('',(-4.65,1.51,16.2));
#32366=CARTESIAN_POINT('Origin',(-5.6,1.4843933982822,15.6));
#32367=CARTESIAN_POINT('Origin',(-5.6,1.4587867965644,15.6));
#32368=CARTESIAN_POINT('Origin',(-5.6,1.51,15.6));
#32369=CARTESIAN_POINT('Origin',(-3.1,1.44,16.16));
#32370=CARTESIAN_POINT('',(-5.6,1.48,16.2));
#32371=CARTESIAN_POINT('Origin',(-5.6,1.44,15.6));
#32372=CARTESIAN_POINT('',(-6.2,1.48,15.6));
#32373=CARTESIAN_POINT('Origin',(-6.16,1.44,4.95));
#32374=CARTESIAN_POINT('Origin',(4.65,3.1156066017178,1.2106066017178));
#32375=CARTESIAN_POINT('',(-6.1787867965644,3.1412132034356,1.2212132034356));
#32376=CARTESIAN_POINT('',(-6.2,3.09,1.2));
#32377=CARTESIAN_POINT('',(6.1787867965644,3.1412132034356,1.2212132034356));
#32378=CARTESIAN_POINT('',(4.65,3.1412132034356,1.2212132034356));
#32379=CARTESIAN_POINT('',(6.185,3.1262132034356,1.215));
#32380=CARTESIAN_POINT('',(6.1787867965644,3.1412132034356,1.2212132034356));
#32381=CARTESIAN_POINT('',(5.81886979044864,2.24229668594221,0.848869790448636));
#32382=CARTESIAN_POINT('Origin',(6.185,1.4,1.215));
#32383=CARTESIAN_POINT('',(6.2,3.09,1.23));
#32384=CARTESIAN_POINT('',(7.29042303399442,0.457485922606718,2.32042303399443));
#32385=CARTESIAN_POINT('',(6.2,1.4,1.23));
#32386=CARTESIAN_POINT('Origin',(6.2,1.4,16.2));
#32387=CARTESIAN_POINT('',(6.2,3.09,15.6));
#32388=CARTESIAN_POINT('',(6.2,3.09,14.325));
#32389=CARTESIAN_POINT('',(6.2,1.4,15.6));
#32390=CARTESIAN_POINT('Origin',(6.1893933982822,3.1156066017178,14.325));
#32391=CARTESIAN_POINT('',(6.1787867965644,3.1412132034356,15.6));
#32392=CARTESIAN_POINT('',(6.1787867965644,3.1412132034356,14.325));
#32393=CARTESIAN_POINT('',(6.2,3.09,15.6));
#32394=CARTESIAN_POINT('Origin',(-6.1893933982822,3.1156066017178,3.075));
#32395=CARTESIAN_POINT('',(-6.2,3.09,15.6));
#32396=CARTESIAN_POINT('',(-6.2,3.09,3.075));
#32397=CARTESIAN_POINT('',(-6.1787867965644,3.1412132034356,15.6));
#32398=CARTESIAN_POINT('',(-6.2,3.09,15.6));
#32399=CARTESIAN_POINT('',(-6.1787867965644,3.1412132034356,3.075));
#32400=CARTESIAN_POINT('Origin',(-5.6,3.1156066017178,15.6));
#32401=CARTESIAN_POINT('',(-5.6,3.09,16.2));
#32402=CARTESIAN_POINT('',(-5.6,3.1412132034356,16.1787867965644));
#32403=CARTESIAN_POINT('',(-5.6,3.09,16.2));
#32404=CARTESIAN_POINT('Origin',(-5.6,3.1412132034356,15.6));
#32405=CARTESIAN_POINT('Origin',(-5.6,3.09,15.6));
#32406=CARTESIAN_POINT('Origin',(-4.65,3.1156066017178,16.1893933982822));
#32407=CARTESIAN_POINT('',(5.6,3.09,16.2));
#32408=CARTESIAN_POINT('',(5.6,3.1412132034356,16.1787867965644));
#32409=CARTESIAN_POINT('',(5.6,3.09,16.2));
#32410=CARTESIAN_POINT('',(-4.65,3.1412132034356,16.1787867965644));
#32411=CARTESIAN_POINT('',(-4.65,3.09,16.2));
#32412=CARTESIAN_POINT('Origin',(5.6,3.1156066017178,15.6));
#32413=CARTESIAN_POINT('Origin',(5.6,3.1412132034356,15.6));
#32414=CARTESIAN_POINT('Origin',(5.6,3.09,15.6));
#32415=CARTESIAN_POINT('Origin',(5.6,3.16,15.6));
#32416=CARTESIAN_POINT('',(6.1412132034356,3.1787867965644,15.6));
#32417=CARTESIAN_POINT('',(6.2,3.12,15.6));
#32418=CARTESIAN_POINT('',(5.6,3.17878679656441,16.1412132034356));
#32419=CARTESIAN_POINT('Origin',(5.6,3.1787867965644,15.6));
#32420=CARTESIAN_POINT('',(5.6,3.12,16.2));
#32421=CARTESIAN_POINT('Origin',(6.16,3.16,12.45));
#32422=CARTESIAN_POINT('',(6.1412132034356,3.1787867965644,1.2587867965644));
#32423=CARTESIAN_POINT('',(6.12,3.2,1.28));
#32424=CARTESIAN_POINT('',(6.1412132034356,3.1787867965644,10.575));
#32425=CARTESIAN_POINT('Origin',(3.1,3.16,1.24));
#32426=CARTESIAN_POINT('',(-6.1412132034356,3.1787867965644,1.2587867965644));
#32427=CARTESIAN_POINT('',(-6.12,3.2,1.28));
#32428=CARTESIAN_POINT('',(1.55,3.1787867965644,1.2587867965644));
#32429=CARTESIAN_POINT('Origin',(-5.6,1.4,15.6));
#32430=CARTESIAN_POINT('',(-5.6,1.4,16.2));
#32431=CARTESIAN_POINT('',(-6.2,1.4,15.6));
#32432=CARTESIAN_POINT('Origin',(-6.2,1.4,1.2));
#32433=CARTESIAN_POINT('Origin',(1.55,3.1893933982822,1.2843933982822));
#32434=CARTESIAN_POINT('',(-6.09,3.2,1.31));
#32435=CARTESIAN_POINT('',(6.09,3.2,1.31));
#32436=CARTESIAN_POINT('',(1.55,3.2,1.31));
#32437=CARTESIAN_POINT('',(6.09,3.2,1.31));
#32438=CARTESIAN_POINT('',(-6.1412132034356,3.1787867965644,1.2587867965644));
#32439=CARTESIAN_POINT('Origin',(6.1156066017178,3.1893933982822,10.575));
#32440=CARTESIAN_POINT('',(6.09,3.2,15.6));
#32441=CARTESIAN_POINT('',(6.09,3.2,10.575));
#32442=CARTESIAN_POINT('',(6.09,3.2,15.6));
#32443=CARTESIAN_POINT('Origin',(5.6,3.1893933982822,15.6));
#32444=CARTESIAN_POINT('',(5.6,3.2,16.09));
#32445=CARTESIAN_POINT('',(5.6,3.2,16.09));
#32446=CARTESIAN_POINT('Origin',(5.6,3.2,15.6));
#32447=CARTESIAN_POINT('Origin',(-1.55,3.1893933982822,16.1156066017178));
#32448=CARTESIAN_POINT('',(-5.6,3.2,16.09));
#32449=CARTESIAN_POINT('',(-5.6,3.1787867965644,16.1412132034356));
#32450=CARTESIAN_POINT('',(-5.6,3.2,16.09));
#32451=CARTESIAN_POINT('',(-1.55,3.1787867965644,16.1412132034356));
#32452=CARTESIAN_POINT('',(-1.55,3.2,16.09));
#32453=CARTESIAN_POINT('Origin',(-5.6,3.1893933982822,15.6));
#32454=CARTESIAN_POINT('',(-6.09,3.2,15.6));
#32455=CARTESIAN_POINT('',(-6.1412132034356,3.1787867965644,15.6));
#32456=CARTESIAN_POINT('',(-6.09,3.2,15.6));
#32457=CARTESIAN_POINT('Origin',(-5.6,3.1787867965644,15.6));
#32458=CARTESIAN_POINT('Origin',(-5.6,3.2,15.6));
#32459=CARTESIAN_POINT('Origin',(-6.1156066017178,3.1893933982822,6.825));
#32460=CARTESIAN_POINT('',(-6.1412132034356,3.1787867965644,6.825));
#32461=CARTESIAN_POINT('',(-6.09,3.2,6.825));
#32462=CARTESIAN_POINT('Origin',(-5.6,3.16,15.6));
#32463=CARTESIAN_POINT('',(-5.6,3.12,16.2));
#32464=CARTESIAN_POINT('',(-6.2,3.12,15.6));
#32465=CARTESIAN_POINT('Origin',(-6.16,3.16,4.95));
#32466=CARTESIAN_POINT('Origin',(0.,3.2,8.7));
#32467=CARTESIAN_POINT('',(-3.805,3.2,8.5));
#32468=CARTESIAN_POINT('Origin',(0.,3.2,8.5));
#32469=CARTESIAN_POINT('',(-4.6,3.2,8.5));
#32470=CARTESIAN_POINT('Origin',(-4.4,3.2,8.5));
#32471=CARTESIAN_POINT('',(0.423749999999999,3.2,3.15));
#32472=CARTESIAN_POINT('Origin',(-9.82779056315751E-16,3.2,3.15));
#32473=CARTESIAN_POINT('',(5.05698591024675,3.2,11.175));
#32474=CARTESIAN_POINT('Origin',(4.63323591024675,3.2,11.175));
#32475=CARTESIAN_POINT('',(-1.995,3.2,4.68948822334847));
#32476=CARTESIAN_POINT('Origin',(-2.2,3.2,4.68948822334847));
#32477=CARTESIAN_POINT('',(-1.995,3.2,12.3105117766515));
#32478=CARTESIAN_POINT('Origin',(-2.2,3.2,12.3105117766515));
#32479=CARTESIAN_POINT('',(4.605,3.2,8.5));
#32480=CARTESIAN_POINT('Origin',(4.4,3.2,8.5));
#32481=CARTESIAN_POINT('',(-4.20948591024675,3.2,11.175));
#32482=CARTESIAN_POINT('Origin',(-4.63323591024675,3.2,11.175));
#32483=CARTESIAN_POINT('',(2.,3.2,4.68948822334847));
#32484=CARTESIAN_POINT('Origin',(2.2,3.2,4.68948822334847));
#32485=CARTESIAN_POINT('',(2.,3.2,12.3105117766515));
#32486=CARTESIAN_POINT('Origin',(2.2,3.2,12.3105117766515));
#32487=CARTESIAN_POINT('Origin',(0.,1.415,8.5));
#32488=CARTESIAN_POINT('',(3.3,1.43,8.5));
#32489=CARTESIAN_POINT('',(3.315,1.415,8.5));
#32490=CARTESIAN_POINT('Origin',(0.,1.43,8.5));
#32491=CARTESIAN_POINT('Origin',(0.,2.3,8.5));
#32492=CARTESIAN_POINT('',(3.3,1.87,8.5));
#32493=CARTESIAN_POINT('',(3.3,2.3,8.5));
#32494=CARTESIAN_POINT('Origin',(0.,1.87,8.5));
#32495=CARTESIAN_POINT('Origin',(0.,3.185,8.5));
#32496=CARTESIAN_POINT('',(-3.775,3.17,8.5));
#32497=CARTESIAN_POINT('',(-3.79,3.185,8.5));
#32498=CARTESIAN_POINT('',(3.775,3.17,8.5));
#32499=CARTESIAN_POINT('Origin',(0.,3.17,8.5));
#32500=CARTESIAN_POINT('Origin',(0.,3.17,8.5));
#32501=CARTESIAN_POINT('Origin',(0.,2.55,8.5));
#32502=CARTESIAN_POINT('',(3.775,1.9,8.5));
#32503=CARTESIAN_POINT('Origin',(0.,1.9,8.5));
#32504=CARTESIAN_POINT('',(3.775,2.55,8.5));
#32505=CARTESIAN_POINT('Origin',(0.,1.885,8.5));
#32506=CARTESIAN_POINT('',(3.33,1.9,8.5));
#32507=CARTESIAN_POINT('',(3.315,1.885,8.5));
#32508=CARTESIAN_POINT('Origin',(0.,1.9,8.5));
#32509=CARTESIAN_POINT('Origin',(-3.775,1.9,8.5));
#32510=CARTESIAN_POINT('Origin',(2.2,3.185,12.3105117766515));
#32511=CARTESIAN_POINT('',(2.03,3.17,12.3105117766515));
#32512=CARTESIAN_POINT('',(2.015,3.185,12.3105117766515));
#32513=CARTESIAN_POINT('',(2.37,3.17,12.3105117766515));
#32514=CARTESIAN_POINT('Origin',(2.2,3.17,12.3105117766515));
#32515=CARTESIAN_POINT('Origin',(2.2,3.17,12.3105117766515));
#32516=CARTESIAN_POINT('Origin',(2.2,2.275,12.3105117766515));
#32517=CARTESIAN_POINT('',(2.37,1.43,12.3105117766515));
#32518=CARTESIAN_POINT('Origin',(2.2,1.43,12.3105117766515));
#32519=CARTESIAN_POINT('',(2.37,2.275,12.3105117766515));
#32520=CARTESIAN_POINT('Origin',(2.2,1.415,12.3105117766515));
#32521=CARTESIAN_POINT('',(2.385,1.415,12.3105117766515));
#32522=CARTESIAN_POINT('Origin',(-4.4,3.185,8.5));
#32523=CARTESIAN_POINT('',(-4.57,3.17,8.5));
#32524=CARTESIAN_POINT('',(-4.585,3.185,8.5));
#32525=CARTESIAN_POINT('',(-4.23,3.17,8.5));
#32526=CARTESIAN_POINT('Origin',(-4.4,3.17,8.5));
#32527=CARTESIAN_POINT('Origin',(-4.4,3.17,8.5));
#32528=CARTESIAN_POINT('Origin',(-4.4,2.275,8.5));
#32529=CARTESIAN_POINT('',(-4.23,1.43,8.5));
#32530=CARTESIAN_POINT('Origin',(-4.4,1.43,8.5));
#32531=CARTESIAN_POINT('',(-4.23,2.275,8.5));
#32532=CARTESIAN_POINT('Origin',(-4.4,1.415,8.5));
#32533=CARTESIAN_POINT('',(-4.215,1.415,8.5));
#32534=CARTESIAN_POINT('Origin',(2.2,3.185,4.68948822334847));
#32535=CARTESIAN_POINT('',(2.03,3.17,4.68948822334847));
#32536=CARTESIAN_POINT('',(2.015,3.185,4.68948822334847));
#32537=CARTESIAN_POINT('',(2.37,3.17,4.68948822334847));
#32538=CARTESIAN_POINT('Origin',(2.2,3.17,4.68948822334847));
#32539=CARTESIAN_POINT('Origin',(2.2,3.17,4.68948822334847));
#32540=CARTESIAN_POINT('Origin',(2.2,2.275,4.68948822334847));
#32541=CARTESIAN_POINT('',(2.37,1.43,4.68948822334847));
#32542=CARTESIAN_POINT('Origin',(2.2,1.43,4.68948822334847));
#32543=CARTESIAN_POINT('',(2.37,2.275,4.68948822334847));
#32544=CARTESIAN_POINT('Origin',(2.2,1.415,4.68948822334847));
#32545=CARTESIAN_POINT('',(2.385,1.415,4.68948822334847));
#32546=CARTESIAN_POINT('Origin',(4.63323591024675,1.415,11.175));
#32547=CARTESIAN_POINT('',(5.03823591024675,1.43,11.175));
#32548=CARTESIAN_POINT('',(5.05323591024675,1.415,11.175));
#32549=CARTESIAN_POINT('Origin',(4.63323591024675,1.43,11.175));
#32550=CARTESIAN_POINT('Origin',(4.63323591024675,2.26,11.175));
#32551=CARTESIAN_POINT('',(5.03823591024675,3.17,11.175));
#32552=CARTESIAN_POINT('',(5.03823591024675,2.26,11.175));
#32553=CARTESIAN_POINT('Origin',(4.63323591024675,3.17,11.175));
#32554=CARTESIAN_POINT('Origin',(-4.63323591024675,1.415,11.175));
#32555=CARTESIAN_POINT('',(-4.22823591024675,1.43,11.175));
#32556=CARTESIAN_POINT('',(-4.21323591024675,1.415,11.175));
#32557=CARTESIAN_POINT('Origin',(-4.63323591024675,1.43,11.175));
#32558=CARTESIAN_POINT('Origin',(-4.63323591024675,2.26,11.175));
#32559=CARTESIAN_POINT('',(-4.22823591024675,3.17,11.175));
#32560=CARTESIAN_POINT('',(-4.22823591024675,2.26,11.175));
#32561=CARTESIAN_POINT('Origin',(-4.63323591024675,3.17,11.175));
#32562=CARTESIAN_POINT('Origin',(-9.82779056315751E-16,1.415,3.15));
#32563=CARTESIAN_POINT('',(0.404999999999999,1.43,3.15));
#32564=CARTESIAN_POINT('',(0.419999999999999,1.415,3.15));
#32565=CARTESIAN_POINT('Origin',(-9.82779056315751E-16,1.43,3.15));
#32566=CARTESIAN_POINT('Origin',(-9.82779056315751E-16,2.26,3.15));
#32567=CARTESIAN_POINT('',(0.404999999999999,3.17,3.15));
#32568=CARTESIAN_POINT('',(0.404999999999999,2.26,3.15));
#32569=CARTESIAN_POINT('Origin',(-9.82779056315751E-16,3.17,3.15));
#32570=CARTESIAN_POINT('Origin',(3.5,2.3,16.1893933982822));
#32571=CARTESIAN_POINT('',(3.015,2.3,16.2));
#32572=CARTESIAN_POINT('Origin',(3.5,2.3,16.2));
#32573=CARTESIAN_POINT('',(3.0662132034356,2.3,16.1787867965644));
#32574=CARTESIAN_POINT('',(3.0406066017178,2.3,16.1893933982822));
#32575=CARTESIAN_POINT('Origin',(3.5,2.3,16.1787867965644));
#32576=CARTESIAN_POINT('Origin',(3.5,2.3,16.2));
#32577=CARTESIAN_POINT('',(3.9262132034356,2.3,16.1712132034356));
#32578=CARTESIAN_POINT('',(3.0737867965644,2.3,16.1712132034356));
#32579=CARTESIAN_POINT('Origin',(3.5,2.3,16.1712132034356));
#32580=CARTESIAN_POINT('Origin',(3.5,2.3,16.1712132034356));
#32581=CARTESIAN_POINT('',(3.045,2.3,16.2));
#32582=CARTESIAN_POINT('Origin',(-6.2,1.4,16.2));
#32583=CARTESIAN_POINT('',(5.6,1.4,16.2));
#32584=CARTESIAN_POINT('Origin',(3.5,2.3,16.1456066017178));
#32585=CARTESIAN_POINT('',(3.905,2.3,16.12));
#32586=CARTESIAN_POINT('',(3.095,2.3,16.12));
#32587=CARTESIAN_POINT('Origin',(3.5,2.3,16.12));
#32588=CARTESIAN_POINT('Origin',(3.5,2.3,16.12));
#32589=CARTESIAN_POINT('',(3.9156066017178,2.3,16.1456066017178));
#32590=CARTESIAN_POINT('Origin',(3.5,2.3,15.675));
#32591=CARTESIAN_POINT('',(3.095,2.3,15.2));
#32592=CARTESIAN_POINT('Origin',(3.5,2.3,15.2));
#32593=CARTESIAN_POINT('',(3.095,2.3,15.675));
#32594=CARTESIAN_POINT('Origin',(3.5,2.3,15.0783257246469));
#32595=CARTESIAN_POINT('',(3.5,2.3,14.9566514492938));
#32596=CARTESIAN_POINT('',(3.2975,2.3,15.0783257246469));
#32597=CARTESIAN_POINT('Origin',(4.5,2.3,2.27660972892601));
#32598=CARTESIAN_POINT('',(4.5,2.3,2.35321945785203));
#32599=CARTESIAN_POINT('',(4.755,2.3,2.2));
#32600=CARTESIAN_POINT('',(4.6275,2.3,2.27660972892601));
#32601=CARTESIAN_POINT('Origin',(4.5,2.3,2.2));
#32602=CARTESIAN_POINT('Origin',(4.5,2.3,1.725));
#32603=CARTESIAN_POINT('',(4.755,2.3,1.25));
#32604=CARTESIAN_POINT('',(4.755,2.3,1.725));
#32605=CARTESIAN_POINT('Origin',(4.5,2.3,1.25));
#32606=CARTESIAN_POINT('Origin',(4.5,2.3,1.2));
#32607=CARTESIAN_POINT('',(4.805,2.3,1.2));
#32608=CARTESIAN_POINT('Origin',(0.,2.3,2.27660972892601));
#32609=CARTESIAN_POINT('',(0.,2.3,2.35321945785203));
#32610=CARTESIAN_POINT('',(0.255,2.3,2.2));
#32611=CARTESIAN_POINT('',(0.1275,2.3,2.27660972892601));
#32612=CARTESIAN_POINT('Origin',(0.,2.3,2.2));
#32613=CARTESIAN_POINT('Origin',(0.,2.3,1.725));
#32614=CARTESIAN_POINT('',(0.255,2.3,1.25));
#32615=CARTESIAN_POINT('',(0.255,2.3,1.725));
#32616=CARTESIAN_POINT('Origin',(0.,2.3,1.25));
#32617=CARTESIAN_POINT('Origin',(0.,2.3,1.2));
#32618=CARTESIAN_POINT('',(0.305,2.3,1.2));
#32619=CARTESIAN_POINT('Origin',(-4.5,2.3,2.27660972892601));
#32620=CARTESIAN_POINT('',(-4.5,2.3,2.35321945785203));
#32621=CARTESIAN_POINT('',(-4.245,2.3,2.2));
#32622=CARTESIAN_POINT('',(-4.3725,2.3,2.27660972892601));
#32623=CARTESIAN_POINT('Origin',(-4.5,2.3,2.2));
#32624=CARTESIAN_POINT('Origin',(-4.5,2.3,1.725));
#32625=CARTESIAN_POINT('',(-4.245,2.3,1.25));
#32626=CARTESIAN_POINT('',(-4.245,2.3,1.725));
#32627=CARTESIAN_POINT('Origin',(-4.5,2.3,1.25));
#32628=CARTESIAN_POINT('Origin',(-4.5,2.3,1.2));
#32629=CARTESIAN_POINT('',(-4.195,2.3,1.2));
#32630=CARTESIAN_POINT('Origin',(-9.82779056315751E-16,3.21,3.15));
#32631=CARTESIAN_POINT('',(0.429999999999999,3.21,3.15));
#32632=CARTESIAN_POINT('Origin',(-4.63323591024675,3.21,11.175));
#32633=CARTESIAN_POINT('',(-4.20323591024675,3.21,11.175));
#32634=CARTESIAN_POINT('Origin',(4.63323591024675,3.21,11.175));
#32635=CARTESIAN_POINT('',(5.06323591024675,3.21,11.175));
#32636=CARTESIAN_POINT('Origin',(-2.2,2.45343330202536,4.68948822334847));
#32637=CARTESIAN_POINT('',(-2.2,2.40686660405073,4.68948822334847));
#32638=CARTESIAN_POINT('',(-2.045,2.5,4.68948822334847));
#32639=CARTESIAN_POINT('',(-2.1225,2.45343330202536,4.68948822334847));
#32640=CARTESIAN_POINT('Origin',(-2.2,2.5,4.68948822334847));
#32641=CARTESIAN_POINT('Origin',(-2.2,2.825,4.68948822334847));
#32642=CARTESIAN_POINT('',(-2.045,3.15,4.68948822334847));
#32643=CARTESIAN_POINT('',(-2.045,2.825,4.68948822334847));
#32644=CARTESIAN_POINT('Origin',(-2.2,3.15,4.68948822334847));
#32645=CARTESIAN_POINT('Origin',(-2.2,3.2,4.68948822334847));
#32646=CARTESIAN_POINT('',(-1.995,3.2,4.68948822334847));
#32647=CARTESIAN_POINT('Origin',(-2.2,2.45343330202536,12.3105117766515));
#32648=CARTESIAN_POINT('',(-2.2,2.40686660405073,12.3105117766515));
#32649=CARTESIAN_POINT('',(-2.045,2.5,12.3105117766515));
#32650=CARTESIAN_POINT('',(-2.1225,2.45343330202536,12.3105117766515));
#32651=CARTESIAN_POINT('Origin',(-2.2,2.5,12.3105117766515));
#32652=CARTESIAN_POINT('Origin',(-2.2,2.825,12.3105117766515));
#32653=CARTESIAN_POINT('',(-2.045,3.15,12.3105117766515));
#32654=CARTESIAN_POINT('',(-2.045,2.825,12.3105117766515));
#32655=CARTESIAN_POINT('Origin',(-2.2,3.15,12.3105117766515));
#32656=CARTESIAN_POINT('Origin',(-2.2,3.2,12.3105117766515));
#32657=CARTESIAN_POINT('',(-1.995,3.2,12.3105117766515));
#32658=CARTESIAN_POINT('Origin',(4.4,2.45343330202536,8.5));
#32659=CARTESIAN_POINT('',(4.4,2.40686660405073,8.5));
#32660=CARTESIAN_POINT('',(4.555,2.5,8.5));
#32661=CARTESIAN_POINT('',(4.4775,2.45343330202536,8.5));
#32662=CARTESIAN_POINT('Origin',(4.4,2.5,8.5));
#32663=CARTESIAN_POINT('Origin',(4.4,2.825,8.5));
#32664=CARTESIAN_POINT('',(4.555,3.15,8.5));
#32665=CARTESIAN_POINT('',(4.555,2.825,8.5));
#32666=CARTESIAN_POINT('Origin',(4.4,3.15,8.5));
#32667=CARTESIAN_POINT('Origin',(4.4,3.2,8.5));
#32668=CARTESIAN_POINT('',(4.605,3.2,8.5));
#32669=CARTESIAN_POINT('Origin',(-3.1,3.16,16.16));
#32670=CARTESIAN_POINT('Origin',(5.6,1.4,15.6));
#32671=CARTESIAN_POINT('',(0.,0.,0.));
#32672=CARTESIAN_POINT('Origin',(5.4,-3.3893933982822,13.9));
#32673=CARTESIAN_POINT('',(5.89,-3.4,13.9));
#32674=CARTESIAN_POINT('',(5.9412132034356,-3.3787867965644,13.9));
#32675=CARTESIAN_POINT('',(5.89,-3.4,13.9));
#32676=CARTESIAN_POINT('',(5.4,-3.3787867965644,14.4412132034356));
#32677=CARTESIAN_POINT('Origin',(5.4,-3.3787867965644,13.9));
#32678=CARTESIAN_POINT('',(5.4,-3.4,14.39));
#32679=CARTESIAN_POINT('',(5.4,-3.3787867965644,14.4412132034356));
#32680=CARTESIAN_POINT('Origin',(5.4,-3.4,13.9));
#32681=CARTESIAN_POINT('Origin',(5.9156066017178,-3.3893933982822,10.));
#32682=CARTESIAN_POINT('',(5.89,-3.4,3.1));
#32683=CARTESIAN_POINT('',(5.9412132034356,-3.3787867965644,3.1));
#32684=CARTESIAN_POINT('',(5.89,-3.4,3.1));
#32685=CARTESIAN_POINT('',(5.9412132034356,-3.3787867965644,10.));
#32686=CARTESIAN_POINT('',(5.89,-3.4,10.));
#32687=CARTESIAN_POINT('Origin',(5.4,-3.3893933982822,3.1));
#32688=CARTESIAN_POINT('',(5.4,-3.4,2.61));
#32689=CARTESIAN_POINT('',(5.4,-3.3787867965644,2.5587867965644));
#32690=CARTESIAN_POINT('',(5.4,-3.4,2.61));
#32691=CARTESIAN_POINT('Origin',(5.4,-3.3787867965644,3.1));
#32692=CARTESIAN_POINT('Origin',(5.4,-3.4,3.1));
#32693=CARTESIAN_POINT('Origin',(1.5,-3.3893933982822,2.5843933982822));
#32694=CARTESIAN_POINT('',(-5.4,-3.4,2.61));
#32695=CARTESIAN_POINT('',(-5.4,-3.3787867965644,2.5587867965644));
#32696=CARTESIAN_POINT('',(-5.4,-3.4,2.61));
#32697=CARTESIAN_POINT('',(1.5,-3.3787867965644,2.5587867965644));
#32698=CARTESIAN_POINT('',(1.5,-3.4,2.61));
#32699=CARTESIAN_POINT('Origin',(-5.4,-3.3893933982822,3.1));
#32700=CARTESIAN_POINT('',(-5.89,-3.4,3.1));
#32701=CARTESIAN_POINT('',(-5.9412132034356,-3.3787867965644,3.1));
#32702=CARTESIAN_POINT('',(-5.89,-3.4,3.1));
#32703=CARTESIAN_POINT('Origin',(-5.4,-3.3787867965644,3.1));
#32704=CARTESIAN_POINT('Origin',(-5.4,-3.4,3.1));
#32705=CARTESIAN_POINT('Origin',(-5.9156066017178,-3.3893933982822,7.));
#32706=CARTESIAN_POINT('',(-5.89,-3.4,13.9));
#32707=CARTESIAN_POINT('',(-5.9412132034356,-3.3787867965644,13.9));
#32708=CARTESIAN_POINT('',(-5.89,-3.4,13.9));
#32709=CARTESIAN_POINT('',(-5.9412132034356,-3.3787867965644,7.));
#32710=CARTESIAN_POINT('',(-5.89,-3.4,7.));
#32711=CARTESIAN_POINT('Origin',(-5.4,-3.3893933982822,13.9));
#32712=CARTESIAN_POINT('',(-5.4,-3.4,14.39));
#32713=CARTESIAN_POINT('',(-5.4,-3.3787867965644,14.4412132034356));
#32714=CARTESIAN_POINT('',(-5.4,-3.4,14.39));
#32715=CARTESIAN_POINT('Origin',(-5.4,-3.3787867965644,13.9));
#32716=CARTESIAN_POINT('Origin',(-5.4,-3.4,13.9));
#32717=CARTESIAN_POINT('Origin',(-1.5,-3.3893933982822,14.4156066017178));
#32718=CARTESIAN_POINT('',(-1.5,-3.3787867965644,14.4412132034356));
#32719=CARTESIAN_POINT('',(-1.5,-3.4,14.39));
#32720=CARTESIAN_POINT('Origin',(-5.96,-3.36,5.5));
#32721=CARTESIAN_POINT('',(-5.9787867965644,-3.3412132034356,13.9));
#32722=CARTESIAN_POINT('',(-5.92,-3.4,13.9));
#32723=CARTESIAN_POINT('',(-5.9787867965644,-3.3412132034356,3.1));
#32724=CARTESIAN_POINT('',(-5.9787867965644,-3.3412132034356,4.));
#32725=CARTESIAN_POINT('',(-5.92,-3.4,3.1));
#32726=CARTESIAN_POINT('Origin',(-5.4,-3.36,13.9));
#32727=CARTESIAN_POINT('',(-5.4,-3.3412132034356,14.4787867965644));
#32728=CARTESIAN_POINT('',(-5.4,-3.4,14.42));
#32729=CARTESIAN_POINT('Origin',(-5.4,-3.3412132034356,13.9));
#32730=CARTESIAN_POINT('Origin',(-3.,-3.36,14.46));
#32731=CARTESIAN_POINT('',(5.4,-3.3412132034356,14.4787867965644));
#32732=CARTESIAN_POINT('',(5.4,-3.32,14.5));
#32733=CARTESIAN_POINT('',(-4.5,-3.3412132034356,14.4787867965644));
#32734=CARTESIAN_POINT('Origin',(5.4,-3.36,13.9));
#32735=CARTESIAN_POINT('',(5.9787867965644,-3.3412132034356,13.9));
#32736=CARTESIAN_POINT('',(5.92,-3.4,13.9));
#32737=CARTESIAN_POINT('Origin',(5.4,-3.3412132034356,13.9));
#32738=CARTESIAN_POINT('Origin',(0.,-3.4,8.5));
#32739=CARTESIAN_POINT('',(3.805,-3.4,8.5));
#32740=CARTESIAN_POINT('Origin',(0.,-3.4,8.5));
#32741=CARTESIAN_POINT('',(-0.255000000000001,-3.4,3.9));
#32742=CARTESIAN_POINT('Origin',(-8.45006291411674E-16,-3.4,3.9));
#32743=CARTESIAN_POINT('',(-3.50769119345812,-3.4,11.7526911934581));
#32744=CARTESIAN_POINT('Origin',(-3.25269119345812,-3.4,11.7526911934581));
#32745=CARTESIAN_POINT('',(2.99769119345812,-3.4,11.7526911934581));
#32746=CARTESIAN_POINT('Origin',(3.25269119345812,-3.4,11.7526911934581));
#32747=CARTESIAN_POINT('Origin',(4.5,-3.3156066017178,2.5106066017178));
#32748=CARTESIAN_POINT('',(5.4,-3.29,2.5));
#32749=CARTESIAN_POINT('',(5.4,-3.3412132034356,2.5212132034356));
#32750=CARTESIAN_POINT('',(5.4,-3.29,2.5));
#32751=CARTESIAN_POINT('',(-5.4,-3.3412132034356,2.5212132034356));
#32752=CARTESIAN_POINT('',(4.5,-3.3412132034356,2.5212132034356));
#32753=CARTESIAN_POINT('',(-5.4,-3.29,2.5));
#32754=CARTESIAN_POINT('',(-5.4,-3.3412132034356,2.5212132034356));
#32755=CARTESIAN_POINT('',(4.5,-3.29,2.5));
#32756=CARTESIAN_POINT('Origin',(5.4,-3.3156066017178,3.1));
#32757=CARTESIAN_POINT('',(6.,-3.29,3.1));
#32758=CARTESIAN_POINT('',(5.9787867965644,-3.3412132034356,3.1));
#32759=CARTESIAN_POINT('',(6.,-3.29,3.1));
#32760=CARTESIAN_POINT('Origin',(5.4,-3.3412132034356,3.1));
#32761=CARTESIAN_POINT('Origin',(5.4,-3.29,3.1));
#32762=CARTESIAN_POINT('Origin',(5.9893933982822,-3.3156066017178,13.));
#32763=CARTESIAN_POINT('',(6.,-3.29,13.9));
#32764=CARTESIAN_POINT('',(6.,-3.29,13.9));
#32765=CARTESIAN_POINT('',(5.9787867965644,-3.3412132034356,13.));
#32766=CARTESIAN_POINT('',(6.,-3.29,13.));
#32767=CARTESIAN_POINT('Origin',(5.4,-3.3156066017178,13.9));
#32768=CARTESIAN_POINT('',(5.4,-3.29,14.5));
#32769=CARTESIAN_POINT('',(5.4,-3.29,14.5));
#32770=CARTESIAN_POINT('Origin',(5.4,-3.29,13.9));
#32771=CARTESIAN_POINT('Origin',(-4.5,-3.3156066017178,14.4893933982822));
#32772=CARTESIAN_POINT('',(-5.4,-3.29,14.5));
#32773=CARTESIAN_POINT('',(-5.4,-3.29,14.5));
#32774=CARTESIAN_POINT('',(-4.5,-3.29,14.5));
#32775=CARTESIAN_POINT('Origin',(-5.4,-3.3156066017178,13.9));
#32776=CARTESIAN_POINT('',(-6.,-3.29,13.9));
#32777=CARTESIAN_POINT('',(-6.,-3.29,13.9));
#32778=CARTESIAN_POINT('Origin',(-5.4,-3.29,13.9));
#32779=CARTESIAN_POINT('Origin',(-5.9893933982822,-3.3156066017178,4.));
#32780=CARTESIAN_POINT('',(-6.,-3.29,3.1));
#32781=CARTESIAN_POINT('',(-6.,-3.29,3.1));
#32782=CARTESIAN_POINT('',(-6.,-3.29,4.));
#32783=CARTESIAN_POINT('Origin',(-5.4,-3.3156066017178,3.1));
#32784=CARTESIAN_POINT('Origin',(-5.4,-3.3412132034356,3.1));
#32785=CARTESIAN_POINT('Origin',(-5.4,-3.29,3.1));
#32786=CARTESIAN_POINT('Origin',(5.4,-3.4,13.9));
#32787=CARTESIAN_POINT('',(6.,-1.71,13.9));
#32788=CARTESIAN_POINT('',(6.,-3.4,13.9));
#32789=CARTESIAN_POINT('',(5.4,-1.71,14.5));
#32790=CARTESIAN_POINT('Origin',(5.4,-1.71,13.9));
#32791=CARTESIAN_POINT('',(5.4,-3.4,14.5));
#32792=CARTESIAN_POINT('Origin',(6.,-3.4,14.5));
#32793=CARTESIAN_POINT('',(6.,-1.71,3.1));
#32794=CARTESIAN_POINT('',(6.,-3.4,3.1));
#32795=CARTESIAN_POINT('',(6.,-1.71,13.));
#32796=CARTESIAN_POINT('Origin',(5.4,-3.4,3.1));
#32797=CARTESIAN_POINT('',(5.4,-1.71,2.5));
#32798=CARTESIAN_POINT('',(5.4,-3.4,2.5));
#32799=CARTESIAN_POINT('Origin',(5.4,-1.71,3.1));
#32800=CARTESIAN_POINT('Origin',(6.,-3.4,2.5));
#32801=CARTESIAN_POINT('',(-5.4,-1.71,2.5));
#32802=CARTESIAN_POINT('',(-5.4,-3.4,2.5));
#32803=CARTESIAN_POINT('',(4.5,-1.71,2.5));
#32804=CARTESIAN_POINT('Origin',(-5.4,-3.36,3.1));
#32805=CARTESIAN_POINT('',(-5.4,-3.4,2.58));
#32806=CARTESIAN_POINT('Origin',(3.,-3.36,2.54));
#32807=CARTESIAN_POINT('',(5.4,-3.4,2.58));
#32808=CARTESIAN_POINT('Origin',(5.4,-1.6843933982822,13.9));
#32809=CARTESIAN_POINT('',(5.9787867965644,-1.6587867965644,13.9));
#32810=CARTESIAN_POINT('',(6.,-1.71,13.9));
#32811=CARTESIAN_POINT('',(5.4,-1.6587867965644,14.4787867965644));
#32812=CARTESIAN_POINT('Origin',(5.4,-1.6587867965644,13.9));
#32813=CARTESIAN_POINT('',(5.4,-1.6587867965644,14.4787867965644));
#32814=CARTESIAN_POINT('Origin',(5.9893933982822,-1.6843933982822,13.));
#32815=CARTESIAN_POINT('',(5.9787867965644,-1.6587867965644,3.1));
#32816=CARTESIAN_POINT('',(6.,-1.71,3.1));
#32817=CARTESIAN_POINT('',(5.9787867965644,-1.6587867965644,13.));
#32818=CARTESIAN_POINT('Origin',(5.4,-1.6843933982822,3.1));
#32819=CARTESIAN_POINT('',(5.4,-1.6587867965644,2.5212132034356));
#32820=CARTESIAN_POINT('',(5.4,-1.71,2.5));
#32821=CARTESIAN_POINT('Origin',(5.4,-1.6587867965644,3.1));
#32822=CARTESIAN_POINT('Origin',(4.5,-1.6843933982822,2.5106066017178));
#32823=CARTESIAN_POINT('',(-5.4,-1.6587867965644,2.5212132034356));
#32824=CARTESIAN_POINT('',(-5.4,-1.71,2.5));
#32825=CARTESIAN_POINT('',(4.5,-1.6587867965644,2.5212132034356));
#32826=CARTESIAN_POINT('Origin',(-5.4,-1.6843933982822,3.1));
#32827=CARTESIAN_POINT('',(-6.,-1.71,3.1));
#32828=CARTESIAN_POINT('',(-5.9787867965644,-1.6587867965644,3.1));
#32829=CARTESIAN_POINT('',(-6.,-1.71,3.1));
#32830=CARTESIAN_POINT('Origin',(-5.4,-1.6587867965644,3.1));
#32831=CARTESIAN_POINT('Origin',(-5.4,-1.71,3.1));
#32832=CARTESIAN_POINT('Origin',(-5.9893933982822,-1.6843933982822,4.));
#32833=CARTESIAN_POINT('',(-6.,-1.71,13.9));
#32834=CARTESIAN_POINT('',(-5.9787867965644,-1.6587867965644,13.9));
#32835=CARTESIAN_POINT('',(-6.,-1.71,13.9));
#32836=CARTESIAN_POINT('',(-5.9787867965644,-1.6587867965644,4.));
#32837=CARTESIAN_POINT('',(-6.,-1.71,4.));
#32838=CARTESIAN_POINT('Origin',(-5.4,-1.6843933982822,13.9));
#32839=CARTESIAN_POINT('',(-5.4,-1.71,14.5));
#32840=CARTESIAN_POINT('',(-5.4,-1.65878679656441,14.4787867965644));
#32841=CARTESIAN_POINT('',(-5.4,-1.71,14.5));
#32842=CARTESIAN_POINT('Origin',(-5.4,-1.6587867965644,13.9));
#32843=CARTESIAN_POINT('Origin',(-5.4,-1.71,13.9));
#32844=CARTESIAN_POINT('Origin',(-4.5,-1.6843933982822,14.4893933982822));
#32845=CARTESIAN_POINT('',(-4.5,-1.6587867965644,14.4787867965644));
#32846=CARTESIAN_POINT('',(-4.5,-1.71,14.5));
#32847=CARTESIAN_POINT('Origin',(-5.96,-1.64,5.5));
#32848=CARTESIAN_POINT('',(-5.9412132034356,-1.6212132034356,13.9));
#32849=CARTESIAN_POINT('',(-5.92,-1.6,13.9));
#32850=CARTESIAN_POINT('',(-5.9412132034356,-1.6212132034356,3.1));
#32851=CARTESIAN_POINT('',(-5.9412132034356,-1.6212132034356,7.));
#32852=CARTESIAN_POINT('',(-5.92,-1.6,3.1));
#32853=CARTESIAN_POINT('Origin',(-5.4,-1.64,13.9));
#32854=CARTESIAN_POINT('',(-5.4,-1.6212132034356,14.4412132034356));
#32855=CARTESIAN_POINT('',(-5.4,-1.6,14.42));
#32856=CARTESIAN_POINT('Origin',(-5.4,-1.6212132034356,13.9));
#32857=CARTESIAN_POINT('Origin',(-3.,-1.64,14.46));
#32858=CARTESIAN_POINT('',(5.4,-1.62121320343559,14.4412132034356));
#32859=CARTESIAN_POINT('',(5.4,-1.6,14.42));
#32860=CARTESIAN_POINT('',(-1.5,-1.6212132034356,14.4412132034356));
#32861=CARTESIAN_POINT('Origin',(5.4,-1.64,13.9));
#32862=CARTESIAN_POINT('',(5.9412132034356,-1.6212132034356,13.9));
#32863=CARTESIAN_POINT('',(6.,-1.68,13.9));
#32864=CARTESIAN_POINT('Origin',(5.4,-1.6212132034356,13.9));
#32865=CARTESIAN_POINT('Origin',(0.,-3.385,8.5));
#32866=CARTESIAN_POINT('',(3.775,-3.37,8.5));
#32867=CARTESIAN_POINT('',(3.79,-3.385,8.5));
#32868=CARTESIAN_POINT('',(-3.775,-3.37,8.5));
#32869=CARTESIAN_POINT('Origin',(0.,-3.37,8.5));
#32870=CARTESIAN_POINT('Origin',(0.,-3.37,8.5));
#32871=CARTESIAN_POINT('Origin',(0.,-2.8,8.5));
#32872=CARTESIAN_POINT('',(-3.775,-2.2,8.5));
#32873=CARTESIAN_POINT('Origin',(0.,-2.2,8.5));
#32874=CARTESIAN_POINT('',(-3.775,-2.8,8.5));
#32875=CARTESIAN_POINT('Origin',(5.4,-1.6106066017178,13.9));
#32876=CARTESIAN_POINT('',(5.4,-1.6,14.39));
#32877=CARTESIAN_POINT('',(5.4,-1.6,14.39));
#32878=CARTESIAN_POINT('',(5.89,-1.6,13.9));
#32879=CARTESIAN_POINT('',(5.9412132034356,-1.6212132034356,13.9));
#32880=CARTESIAN_POINT('Origin',(5.4,-1.6,13.9));
#32881=CARTESIAN_POINT('Origin',(-1.5,-1.6106066017178,14.4156066017178));
#32882=CARTESIAN_POINT('',(-5.4,-1.6,14.39));
#32883=CARTESIAN_POINT('',(-5.4,-1.6,14.39));
#32884=CARTESIAN_POINT('',(-1.5,-1.6,14.39));
#32885=CARTESIAN_POINT('Origin',(-5.4,-1.6106066017178,13.9));
#32886=CARTESIAN_POINT('',(-5.89,-1.6,13.9));
#32887=CARTESIAN_POINT('',(-5.89,-1.6,13.9));
#32888=CARTESIAN_POINT('Origin',(-5.4,-1.6,13.9));
#32889=CARTESIAN_POINT('Origin',(-5.9156066017178,-1.6106066017178,7.));
#32890=CARTESIAN_POINT('',(-5.89,-1.6,3.1));
#32891=CARTESIAN_POINT('',(-5.89,-1.6,3.1));
#32892=CARTESIAN_POINT('',(-5.89,-1.6,7.));
#32893=CARTESIAN_POINT('Origin',(-5.4,-1.6106066017178,3.1));
#32894=CARTESIAN_POINT('',(-5.4,-1.6,2.61));
#32895=CARTESIAN_POINT('',(-5.4,-1.6212132034356,2.5587867965644));
#32896=CARTESIAN_POINT('',(-5.4,-1.6,2.61));
#32897=CARTESIAN_POINT('Origin',(-5.4,-1.6212132034356,3.1));
#32898=CARTESIAN_POINT('Origin',(-5.4,-1.6,3.1));
#32899=CARTESIAN_POINT('Origin',(1.5,-1.6106066017178,2.5843933982822));
#32900=CARTESIAN_POINT('',(5.4,-1.6,2.61));
#32901=CARTESIAN_POINT('',(5.4,-1.6212132034356,2.5587867965644));
#32902=CARTESIAN_POINT('',(5.4,-1.6,2.61));
#32903=CARTESIAN_POINT('',(1.5,-1.6212132034356,2.5587867965644));
#32904=CARTESIAN_POINT('',(1.5,-1.6,2.61));
#32905=CARTESIAN_POINT('Origin',(5.4,-1.6106066017178,3.1));
#32906=CARTESIAN_POINT('',(5.89,-1.6,3.1));
#32907=CARTESIAN_POINT('',(5.9412132034356,-1.6212132034356,3.1));
#32908=CARTESIAN_POINT('',(5.89,-1.6,3.1));
#32909=CARTESIAN_POINT('Origin',(5.4,-1.6212132034356,3.1));
#32910=CARTESIAN_POINT('Origin',(5.4,-1.6,3.1));
#32911=CARTESIAN_POINT('Origin',(5.9156066017178,-1.6106066017178,10.));
#32912=CARTESIAN_POINT('',(5.9412132034356,-1.6212132034356,10.));
#32913=CARTESIAN_POINT('',(5.89,-1.6,10.));
#32914=CARTESIAN_POINT('Origin',(3.,-1.64,2.54));
#32915=CARTESIAN_POINT('',(-5.4,-1.6,2.58));
#32916=CARTESIAN_POINT('',(5.4,-1.6,2.58));
#32917=CARTESIAN_POINT('Origin',(5.4,-1.64,3.1));
#32918=CARTESIAN_POINT('',(5.92,-1.6,3.1));
#32919=CARTESIAN_POINT('Origin',(5.96,-1.64,11.5));
#32920=CARTESIAN_POINT('Origin',(0.,-1.6,8.5));
#32921=CARTESIAN_POINT('',(-3.38,-1.6,8.5));
#32922=CARTESIAN_POINT('Origin',(0.,-1.6,8.5));
#32923=CARTESIAN_POINT('Origin',(0.,-2.185,8.5));
#32924=CARTESIAN_POINT('',(-3.3,-2.17,8.5));
#32925=CARTESIAN_POINT('Origin',(0.,-2.17,8.5));
#32926=CARTESIAN_POINT('',(-3.33,-2.2,8.5));
#32927=CARTESIAN_POINT('',(-3.315,-2.185,8.5));
#32928=CARTESIAN_POINT('Origin',(0.,-2.2,8.5));
#32929=CARTESIAN_POINT('Origin',(0.,-2.5,8.5));
#32930=CARTESIAN_POINT('',(-3.3,-1.68,8.5));
#32931=CARTESIAN_POINT('Origin',(0.,-1.68,8.5));
#32932=CARTESIAN_POINT('',(-3.3,-2.5,8.5));
#32933=CARTESIAN_POINT('Origin',(3.775,-2.2,8.5));
#32934=CARTESIAN_POINT('Origin',(0.,-1.6106066017178,8.5));
#32935=CARTESIAN_POINT('',(-3.3287867965644,-1.6212132034356,8.5));
#32936=CARTESIAN_POINT('Origin',(0.,-1.6212132034356,8.5));
#32937=CARTESIAN_POINT('',(-3.3543933982822,-1.6106066017178,8.5));
#32938=CARTESIAN_POINT('Origin',(0.,-1.625,8.5));
#32939=CARTESIAN_POINT('',(-3.3212132034356,-1.6287867965644,8.5));
#32940=CARTESIAN_POINT('',(-3.325,-1.625,8.5));
#32941=CARTESIAN_POINT('Origin',(0.,-1.6287867965644,8.5));
#32942=CARTESIAN_POINT('Origin',(0.,-1.6543933982822,8.5));
#32943=CARTESIAN_POINT('',(-3.3106066017178,-1.6543933982822,8.5));
#32944=CARTESIAN_POINT('Origin',(-8.45006291411674E-16,-2.33841178654967,
3.9));
#32945=CARTESIAN_POINT('',(-8.45006291411674E-16,-2.27682357309935,3.9));
#32946=CARTESIAN_POINT('',(-0.205000000000001,-2.4,3.9));
#32947=CARTESIAN_POINT('',(-0.102500000000001,-2.33841178654967,3.9));
#32948=CARTESIAN_POINT('Origin',(-8.45006291411674E-16,-2.4,3.9));
#32949=CARTESIAN_POINT('Origin',(-8.45006291411674E-16,-2.875,3.9));
#32950=CARTESIAN_POINT('',(-0.205000000000001,-3.35,3.9));
#32951=CARTESIAN_POINT('',(-0.205000000000001,-2.875,3.9));
#32952=CARTESIAN_POINT('Origin',(-8.45006291411674E-16,-3.35,3.9));
#32953=CARTESIAN_POINT('Origin',(-8.45006291411674E-16,-3.4,3.9));
#32954=CARTESIAN_POINT('',(-0.255000000000001,-3.4,3.9));
#32955=CARTESIAN_POINT('Origin',(-3.25269119345812,-2.33841178654967,11.7526911934581));
#32956=CARTESIAN_POINT('',(-3.25269119345812,-2.27682357309935,11.7526911934581));
#32957=CARTESIAN_POINT('',(-3.45769119345812,-2.4,11.7526911934581));
#32958=CARTESIAN_POINT('',(-3.35519119345812,-2.33841178654967,11.7526911934581));
#32959=CARTESIAN_POINT('Origin',(-3.25269119345812,-2.4,11.7526911934581));
#32960=CARTESIAN_POINT('Origin',(-3.25269119345812,-2.875,11.7526911934581));
#32961=CARTESIAN_POINT('',(-3.45769119345812,-3.35,11.7526911934581));
#32962=CARTESIAN_POINT('',(-3.45769119345812,-2.875,11.7526911934581));
#32963=CARTESIAN_POINT('Origin',(-3.25269119345812,-3.35,11.7526911934581));
#32964=CARTESIAN_POINT('Origin',(-3.25269119345812,-3.4,11.7526911934581));
#32965=CARTESIAN_POINT('',(-3.50769119345812,-3.4,11.7526911934581));
#32966=CARTESIAN_POINT('Origin',(3.25269119345812,-2.33841178654967,11.7526911934581));
#32967=CARTESIAN_POINT('',(3.25269119345812,-2.27682357309935,11.7526911934581));
#32968=CARTESIAN_POINT('',(3.04769119345812,-2.4,11.7526911934581));
#32969=CARTESIAN_POINT('',(3.15019119345812,-2.33841178654967,11.7526911934581));
#32970=CARTESIAN_POINT('Origin',(3.25269119345812,-2.4,11.7526911934581));
#32971=CARTESIAN_POINT('Origin',(3.25269119345812,-2.875,11.7526911934581));
#32972=CARTESIAN_POINT('',(3.04769119345812,-3.35,11.7526911934581));
#32973=CARTESIAN_POINT('',(3.04769119345812,-2.875,11.7526911934581));
#32974=CARTESIAN_POINT('Origin',(3.25269119345812,-3.35,11.7526911934581));
#32975=CARTESIAN_POINT('Origin',(3.25269119345812,-3.4,11.7526911934581));
#32976=CARTESIAN_POINT('',(2.99769119345812,-3.4,11.7526911934581));
#32977=CARTESIAN_POINT('Origin',(-5.4,-1.64,3.1));
#32978=CARTESIAN_POINT('Origin',(5.96,-3.36,11.5));
#32979=CARTESIAN_POINT('',(5.92,-3.4,3.1));
#32980=CARTESIAN_POINT('Origin',(5.4,-3.36,3.1));
#32981=CARTESIAN_POINT('Origin',(-6.,-3.4,2.5));
#32982=CARTESIAN_POINT('',(-6.,-3.4,13.9));
#32983=CARTESIAN_POINT('',(-6.,-3.4,3.1));
#32984=CARTESIAN_POINT('Origin',(-5.4,-3.4,13.9));
#32985=CARTESIAN_POINT('',(-5.4,-3.4,14.5));
#32986=CARTESIAN_POINT('Origin',(-6.,-3.4,14.5));
#32987=CARTESIAN_POINT('Origin',(-5.4,-3.4,3.1));
#32988=CARTESIAN_POINT('',(0.,0.,0.));
#32989=CARTESIAN_POINT('Origin',(0.,-1.23114146956912E-16,1.3456066017178));
#32990=CARTESIAN_POINT('',(4.0212132034356,0.,1.3712132034356));
#32991=CARTESIAN_POINT('Origin',(0.,-2.46228293913824E-16,1.3712132034356));
#32992=CARTESIAN_POINT('',(4.,-4.89858719658941E-16,1.32));
#32993=CARTESIAN_POINT('',(4.0106066017178,2.44929359829471E-16,1.3456066017178));
#32994=CARTESIAN_POINT('',(-4.,-4.89858719658941E-16,1.32));
#32995=CARTESIAN_POINT('Origin',(0.,0.,1.32));
#32996=CARTESIAN_POINT('Origin',(0.,0.,1.32));
#32997=CARTESIAN_POINT('Origin',(0.,0.,0.7));
#32998=CARTESIAN_POINT('',(-4.,-4.89858719658941E-16,0.08));
#32999=CARTESIAN_POINT('',(-4.,-4.89858719658941E-16,0.7));
#33000=CARTESIAN_POINT('',(4.,4.89858719658941E-16,0.08));
#33001=CARTESIAN_POINT('Origin',(0.,0.,0.08));
#33002=CARTESIAN_POINT('Origin',(0.,0.,0.08));
#33003=CARTESIAN_POINT('Origin',(0.,0.,1.375));
#33004=CARTESIAN_POINT('',(4.0287867965644,-9.86768170971943E-16,1.3787867965644));
#33005=CARTESIAN_POINT('',(4.025,-4.9292033665681E-16,1.375));
#33006=CARTESIAN_POINT('Origin',(0.,-2.46692042742986E-16,1.3787867965644));
#33007=CARTESIAN_POINT('Origin',(0.,-1.23114146956912E-16,0.0543933982822017));
#33008=CARTESIAN_POINT('',(4.0212132034356,-9.84913175655296E-16,0.0287867965644034));
#33009=CARTESIAN_POINT('Origin',(0.,-2.46228293913824E-16,0.0287867965644034));
#33010=CARTESIAN_POINT('',(4.0106066017178,-7.37385947657118E-16,0.0543933982822017));
#33011=CARTESIAN_POINT('Origin',(0.,0.,0.025));
#33012=CARTESIAN_POINT('',(4.0287867965644,0.,0.0212132034355969));
#33013=CARTESIAN_POINT('Origin',(0.,-2.46692042742986E-16,0.0212132034355969));
#33014=CARTESIAN_POINT('',(4.025,-4.9292033665681E-16,0.025));
#33015=CARTESIAN_POINT('Origin',(0.,-1.23346021371493E-16,0.0106066017177984));
#33016=CARTESIAN_POINT('',(4.08,-4.9965589405212E-16,0.));
#33017=CARTESIAN_POINT('',(4.0543933982822,2.4982794702606E-16,0.0106066017177984));
#33018=CARTESIAN_POINT('Origin',(0.,0.,0.));
#33019=CARTESIAN_POINT('Origin',(4.8,0.,0.));
#33020=CARTESIAN_POINT('',(4.72,5.78033289197551E-16,0.));
#33021=CARTESIAN_POINT('Origin',(0.,0.,0.));
#33022=CARTESIAN_POINT('',(2.405,-3.81051177665153,0.));
#33023=CARTESIAN_POINT('Origin',(2.2,-3.81051177665153,0.));
#33024=CARTESIAN_POINT('',(-4.195,5.63949851007356E-16,0.));
#33025=CARTESIAN_POINT('Origin',(-4.4,5.38844591624835E-16,0.));
#33026=CARTESIAN_POINT('',(2.405,3.81051177665153,0.));
#33027=CARTESIAN_POINT('Origin',(2.2,3.81051177665153,0.));
#33028=CARTESIAN_POINT('Origin',(0.,1.46076274440925E-16,0.0106066017177982));
#33029=CARTESIAN_POINT('',(4.7712132034356,0.,0.0212132034355964));
#33030=CARTESIAN_POINT('Origin',(0.,2.9215254888185E-16,0.0212132034355964));
#33031=CARTESIAN_POINT('',(4.7456066017178,8.73321742362474E-16,0.0106066017177982));
#33032=CARTESIAN_POINT('Origin',(0.,0.,0.025));
#33033=CARTESIAN_POINT('',(4.7787867965644,1.17046519084405E-15,0.0287867965644034));
#33034=CARTESIAN_POINT('Origin',(0.,2.92616297711012E-16,0.0287867965644034));
#33035=CARTESIAN_POINT('',(4.775,5.84768846592861E-16,0.025));
#33036=CARTESIAN_POINT('Origin',(0.,-1.23346021371493E-16,1.3893933982822));
#33037=CARTESIAN_POINT('',(4.08,4.9965589405212E-16,1.4));
#33038=CARTESIAN_POINT('',(4.0543933982822,-7.43212032512032E-16,1.3893933982822));
#33039=CARTESIAN_POINT('Origin',(0.,0.,1.4));
#33040=CARTESIAN_POINT('Origin',(4.,0.,1.4));
#33041=CARTESIAN_POINT('',(4.72,-5.78033289197551E-16,1.4));
#33042=CARTESIAN_POINT('Origin',(0.,0.,1.4));
#33043=CARTESIAN_POINT('Origin',(0.,1.46308148855506E-16,0.0543933982822016));
#33044=CARTESIAN_POINT('',(4.8,-5.8783046359073E-16,0.0799999999999998));
#33045=CARTESIAN_POINT('',(4.7893933982822,-2.93915231795365E-16,0.0543933982822016));
#33046=CARTESIAN_POINT('',(-4.8,-5.8783046359073E-16,0.0799999999999997));
#33047=CARTESIAN_POINT('Origin',(0.,0.,0.0799999999999998));
#33048=CARTESIAN_POINT('Origin',(0.,0.,0.0799999999999998));
#33049=CARTESIAN_POINT('Origin',(0.,0.,0.7));
#33050=CARTESIAN_POINT('',(4.8,5.8783046359073E-16,1.32));
#33051=CARTESIAN_POINT('',(-4.8,-5.8783046359073E-16,1.32));
#33052=CARTESIAN_POINT('Origin',(0.,0.,1.32));
#33053=CARTESIAN_POINT('Origin',(0.,0.,1.32));
#33054=CARTESIAN_POINT('',(-4.8,-5.8783046359073E-16,0.7));
#33055=CARTESIAN_POINT('Origin',(0.,1.46076274440925E-16,1.3893933982822));
#33056=CARTESIAN_POINT('',(4.7712132034356,1.1686101955274E-15,1.3787867965644));
#33057=CARTESIAN_POINT('Origin',(0.,2.9215254888185E-16,1.3787867965644));
#33058=CARTESIAN_POINT('',(4.7456066017178,-2.89016644598775E-16,1.3893933982822));
#33059=CARTESIAN_POINT('Origin',(0.,0.,1.375));
#33060=CARTESIAN_POINT('',(4.7787867965644,0.,1.3712132034356));
#33061=CARTESIAN_POINT('',(4.775,5.84768846592861E-16,1.375));
#33062=CARTESIAN_POINT('Origin',(0.,2.92616297711012E-16,1.3712132034356));
#33063=CARTESIAN_POINT('Origin',(0.,1.46308148855506E-16,1.3456066017178));
#33064=CARTESIAN_POINT('',(4.7893933982822,8.79147827217388E-16,1.3456066017178));
#33065=CARTESIAN_POINT('Origin',(2.2,-3.81051177665153,1.04656669797464));
#33066=CARTESIAN_POINT('',(2.2,-3.81051177665153,1.09313339594927));
#33067=CARTESIAN_POINT('',(2.355,-3.81051177665153,1.));
#33068=CARTESIAN_POINT('',(2.2775,-3.81051177665153,1.04656669797464));
#33069=CARTESIAN_POINT('Origin',(2.2,-3.81051177665153,1.));
#33070=CARTESIAN_POINT('Origin',(2.2,-3.81051177665153,0.525));
#33071=CARTESIAN_POINT('',(2.355,-3.81051177665153,0.05));
#33072=CARTESIAN_POINT('',(2.355,-3.81051177665153,0.525));
#33073=CARTESIAN_POINT('Origin',(2.2,-3.81051177665153,0.05));
#33074=CARTESIAN_POINT('Origin',(2.2,-3.81051177665153,-6.93889390390723E-18));
#33075=CARTESIAN_POINT('',(2.405,-3.81051177665153,-6.93889390390723E-18));
#33076=CARTESIAN_POINT('Origin',(-4.4,5.38844591624835E-16,1.04656669797464));
#33077=CARTESIAN_POINT('',(-4.4,5.38844591624835E-16,1.09313339594927));
#33078=CARTESIAN_POINT('',(-4.245,5.19862566238052E-16,1.));
#33079=CARTESIAN_POINT('',(-4.3225,5.29353578931443E-16,1.04656669797464));
#33080=CARTESIAN_POINT('Origin',(-4.4,5.38844591624835E-16,1.));
#33081=CARTESIAN_POINT('Origin',(-4.4,5.38844591624835E-16,0.525));
#33082=CARTESIAN_POINT('',(-4.245,5.19862566238051E-16,0.05));
#33083=CARTESIAN_POINT('',(-4.245,5.19862566238051E-16,0.525));
#33084=CARTESIAN_POINT('Origin',(-4.4,5.38844591624835E-16,0.05));
#33085=CARTESIAN_POINT('Origin',(-4.4,5.38844591624835E-16,0.));
#33086=CARTESIAN_POINT('',(-4.195,5.13739332242315E-16,0.));
#33087=CARTESIAN_POINT('Origin',(2.2,3.81051177665153,1.04656669797464));
#33088=CARTESIAN_POINT('',(2.2,3.81051177665153,1.09313339594927));
#33089=CARTESIAN_POINT('',(2.355,3.81051177665153,1.));
#33090=CARTESIAN_POINT('',(2.2775,3.81051177665153,1.04656669797464));
#33091=CARTESIAN_POINT('Origin',(2.2,3.81051177665153,1.));
#33092=CARTESIAN_POINT('Origin',(2.2,3.81051177665153,0.525));
#33093=CARTESIAN_POINT('',(2.355,3.81051177665153,0.05));
#33094=CARTESIAN_POINT('',(2.355,3.81051177665153,0.525));
#33095=CARTESIAN_POINT('Origin',(2.2,3.81051177665153,0.05));
#33096=CARTESIAN_POINT('Origin',(2.2,3.81051177665153,-6.93889390390723E-18));
#33097=CARTESIAN_POINT('',(2.405,3.81051177665153,-6.93889390390723E-18));
#33098=CARTESIAN_POINT('',(0.,0.,0.));
#33099=CARTESIAN_POINT('Origin',(4.4,0.,0.385));
#33100=CARTESIAN_POINT('',(4.6,2.44929359829471E-17,0.4));
#33101=CARTESIAN_POINT('Origin',(4.4,0.,0.4));
#33102=CARTESIAN_POINT('',(4.57,-2.0818995585505E-17,0.37));
#33103=CARTESIAN_POINT('',(4.585,2.2655965784226E-17,0.385));
#33104=CARTESIAN_POINT('',(4.23,-2.0818995585505E-17,0.37));
#33105=CARTESIAN_POINT('Origin',(4.4,0.,0.37));
#33106=CARTESIAN_POINT('Origin',(4.4,0.,0.37));
#33107=CARTESIAN_POINT('Origin',(4.4,0.,0.175));
#33108=CARTESIAN_POINT('',(4.23,-2.0818995585505E-17,0.03));
#33109=CARTESIAN_POINT('Origin',(4.4,0.,0.03));
#33110=CARTESIAN_POINT('',(4.23,-2.0818995585505E-17,0.175));
#33111=CARTESIAN_POINT('Origin',(3.3,0.,0.4));
#33112=CARTESIAN_POINT('',(4.66,-5.70685408402667E-16,0.4));
#33113=CARTESIAN_POINT('Origin',(0.,0.,0.4));
#33114=CARTESIAN_POINT('',(2.4,3.81051177665153,0.4));
#33115=CARTESIAN_POINT('Origin',(2.2,3.81051177665153,0.4));
#33116=CARTESIAN_POINT('',(-4.2,5.63337527607783E-16,0.4));
#33117=CARTESIAN_POINT('Origin',(-4.4,5.38844591624835E-16,0.4));
#33118=CARTESIAN_POINT('',(2.4,-3.81051177665153,0.4));
#33119=CARTESIAN_POINT('Origin',(2.2,-3.81051177665153,0.4));
#33120=CARTESIAN_POINT('',(3.34,4.09032030915216E-16,0.4));
#33121=CARTESIAN_POINT('Origin',(0.,0.,0.4));
#33122=CARTESIAN_POINT('',(-2.,-3.81051177665153,0.4));
#33123=CARTESIAN_POINT('Origin',(-2.2,-3.81051177665153,0.4));
#33124=CARTESIAN_POINT('',(-2.,3.81051177665153,0.4));
#33125=CARTESIAN_POINT('Origin',(-2.2,3.81051177665153,0.4));
#33126=CARTESIAN_POINT('Origin',(4.4,0.,0.015));
#33127=CARTESIAN_POINT('',(4.2,2.44929359829471E-17,0.));
#33128=CARTESIAN_POINT('Origin',(4.4,0.,0.));
#33129=CARTESIAN_POINT('',(4.215,2.2655965784226E-17,0.015));
#33130=CARTESIAN_POINT('Origin',(4.7,0.,0.));
#33131=CARTESIAN_POINT('',(4.66,5.70685408402667E-16,0.));
#33132=CARTESIAN_POINT('Origin',(0.,0.,0.));
#33133=CARTESIAN_POINT('',(2.,3.81051177665153,0.));
#33134=CARTESIAN_POINT('Origin',(2.2,3.81051177665153,0.));
#33135=CARTESIAN_POINT('',(-4.6,5.63337527607783E-16,0.));
#33136=CARTESIAN_POINT('Origin',(-4.4,5.38844591624835E-16,0.));
#33137=CARTESIAN_POINT('',(2.,-3.81051177665153,0.));
#33138=CARTESIAN_POINT('Origin',(2.2,-3.81051177665153,0.));
#33139=CARTESIAN_POINT('',(3.34,-4.09032030915216E-16,0.));
#33140=CARTESIAN_POINT('Origin',(0.,0.,0.));
#33141=CARTESIAN_POINT('',(-2.4,-3.81051177665153,0.));
#33142=CARTESIAN_POINT('Origin',(-2.2,-3.81051177665153,0.));
#33143=CARTESIAN_POINT('',(-2.4,3.81051177665153,0.));
#33144=CARTESIAN_POINT('Origin',(-2.2,3.81051177665153,0.));
#33145=CARTESIAN_POINT('Origin',(2.2,3.81051177665153,0.385));
#33146=CARTESIAN_POINT('',(2.37,3.81051177665153,0.37));
#33147=CARTESIAN_POINT('',(2.385,3.81051177665153,0.385));
#33148=CARTESIAN_POINT('',(2.03,3.81051177665153,0.37));
#33149=CARTESIAN_POINT('Origin',(2.2,3.81051177665153,0.37));
#33150=CARTESIAN_POINT('Origin',(2.2,3.81051177665153,0.37));
#33151=CARTESIAN_POINT('Origin',(2.2,3.81051177665153,0.175));
#33152=CARTESIAN_POINT('',(2.03,3.81051177665153,0.03));
#33153=CARTESIAN_POINT('Origin',(2.2,3.81051177665153,0.03));
#33154=CARTESIAN_POINT('',(2.03,3.81051177665153,0.175));
#33155=CARTESIAN_POINT('Origin',(2.2,3.81051177665153,0.015));
#33156=CARTESIAN_POINT('',(2.015,3.81051177665153,0.015));
#33157=CARTESIAN_POINT('Origin',(-2.2,3.81051177665153,0.385));
#33158=CARTESIAN_POINT('',(-2.03,3.81051177665153,0.37));
#33159=CARTESIAN_POINT('',(-2.015,3.81051177665153,0.385));
#33160=CARTESIAN_POINT('',(-2.37,3.81051177665153,0.37));
#33161=CARTESIAN_POINT('Origin',(-2.2,3.81051177665153,0.37));
#33162=CARTESIAN_POINT('Origin',(-2.2,3.81051177665153,0.37));
#33163=CARTESIAN_POINT('Origin',(-2.2,3.81051177665153,0.175));
#33164=CARTESIAN_POINT('',(-2.37,3.81051177665153,0.03));
#33165=CARTESIAN_POINT('Origin',(-2.2,3.81051177665153,0.03));
#33166=CARTESIAN_POINT('',(-2.37,3.81051177665153,0.175));
#33167=CARTESIAN_POINT('Origin',(-2.2,3.81051177665153,0.015));
#33168=CARTESIAN_POINT('',(-2.385,3.81051177665153,0.015));
#33169=CARTESIAN_POINT('Origin',(-4.4,5.38844591624835E-16,0.385));
#33170=CARTESIAN_POINT('',(-4.23,5.1802559603933E-16,0.37));
#33171=CARTESIAN_POINT('',(-4.215,5.61500557409062E-16,0.385));
#33172=CARTESIAN_POINT('',(-4.57,5.1802559603933E-16,0.37));
#33173=CARTESIAN_POINT('Origin',(-4.4,5.38844591624835E-16,0.37));
#33174=CARTESIAN_POINT('Origin',(-4.4,5.38844591624835E-16,0.37));
#33175=CARTESIAN_POINT('Origin',(-4.4,5.38844591624835E-16,0.175));
#33176=CARTESIAN_POINT('',(-4.57,5.1802559603933E-16,0.03));
#33177=CARTESIAN_POINT('Origin',(-4.4,5.38844591624835E-16,0.03));
#33178=CARTESIAN_POINT('',(-4.57,5.1802559603933E-16,0.175));
#33179=CARTESIAN_POINT('Origin',(-4.4,5.38844591624835E-16,0.015));
#33180=CARTESIAN_POINT('',(-4.585,5.61500557409062E-16,0.015));
#33181=CARTESIAN_POINT('Origin',(-2.2,-3.81051177665153,0.385));
#33182=CARTESIAN_POINT('',(-2.03,-3.81051177665153,0.37));
#33183=CARTESIAN_POINT('',(-2.015,-3.81051177665153,0.385));
#33184=CARTESIAN_POINT('',(-2.37,-3.81051177665153,0.37));
#33185=CARTESIAN_POINT('Origin',(-2.2,-3.81051177665153,0.37));
#33186=CARTESIAN_POINT('Origin',(-2.2,-3.81051177665153,0.37));
#33187=CARTESIAN_POINT('Origin',(-2.2,-3.81051177665153,0.175));
#33188=CARTESIAN_POINT('',(-2.37,-3.81051177665153,0.03));
#33189=CARTESIAN_POINT('Origin',(-2.2,-3.81051177665153,0.03));
#33190=CARTESIAN_POINT('',(-2.37,-3.81051177665153,0.175));
#33191=CARTESIAN_POINT('Origin',(-2.2,-3.81051177665153,0.015));
#33192=CARTESIAN_POINT('',(-2.385,-3.81051177665153,0.015));
#33193=CARTESIAN_POINT('Origin',(2.2,-3.81051177665153,0.385));
#33194=CARTESIAN_POINT('',(2.37,-3.81051177665153,0.37));
#33195=CARTESIAN_POINT('',(2.385,-3.81051177665153,0.385));
#33196=CARTESIAN_POINT('',(2.03,-3.81051177665153,0.37));
#33197=CARTESIAN_POINT('Origin',(2.2,-3.81051177665153,0.37));
#33198=CARTESIAN_POINT('Origin',(2.2,-3.81051177665153,0.37));
#33199=CARTESIAN_POINT('Origin',(2.2,-3.81051177665153,0.175));
#33200=CARTESIAN_POINT('',(2.03,-3.81051177665153,0.03));
#33201=CARTESIAN_POINT('Origin',(2.2,-3.81051177665153,0.03));
#33202=CARTESIAN_POINT('',(2.03,-3.81051177665153,0.175));
#33203=CARTESIAN_POINT('Origin',(2.2,-3.81051177665153,0.015));
#33204=CARTESIAN_POINT('',(2.015,-3.81051177665153,0.015));
#33205=CARTESIAN_POINT('Origin',(0.,0.,0.38));
#33206=CARTESIAN_POINT('',(4.7,5.75583995599256E-16,0.36));
#33207=CARTESIAN_POINT('',(4.68,5.73134702000961E-16,0.38));
#33208=CARTESIAN_POINT('',(-4.7,-5.75583995599256E-16,0.36));
#33209=CARTESIAN_POINT('Origin',(0.,0.,0.36));
#33210=CARTESIAN_POINT('Origin',(0.,0.,0.36));
#33211=CARTESIAN_POINT('Origin',(0.,0.,0.2));
#33212=CARTESIAN_POINT('',(-4.7,-5.75583995599256E-16,0.04));
#33213=CARTESIAN_POINT('',(-4.7,-5.75583995599256E-16,0.2));
#33214=CARTESIAN_POINT('',(4.7,-5.75583995599256E-16,0.04));
#33215=CARTESIAN_POINT('Origin',(0.,0.,0.04));
#33216=CARTESIAN_POINT('Origin',(0.,0.,0.04));
#33217=CARTESIAN_POINT('Origin',(0.,0.,0.02));
#33218=CARTESIAN_POINT('',(4.68,5.73134702000961E-16,0.02));
#33219=CARTESIAN_POINT('Origin',(0.,0.,0.02));
#33220=CARTESIAN_POINT('',(3.3,4.04133443718627E-16,0.04));
#33221=CARTESIAN_POINT('',(3.32,-4.06582737316921E-16,0.02));
#33222=CARTESIAN_POINT('',(-3.3,-4.04133443718627E-16,0.04));
#33223=CARTESIAN_POINT('Origin',(0.,0.,0.04));
#33224=CARTESIAN_POINT('Origin',(0.,0.,0.04));
#33225=CARTESIAN_POINT('Origin',(0.,0.,0.2));
#33226=CARTESIAN_POINT('',(3.3,-4.04133443718627E-16,0.36));
#33227=CARTESIAN_POINT('',(-3.3,-4.04133443718627E-16,0.36));
#33228=CARTESIAN_POINT('Origin',(0.,0.,0.36));
#33229=CARTESIAN_POINT('Origin',(0.,0.,0.36));
#33230=CARTESIAN_POINT('',(-3.3,-4.04133443718627E-16,0.2));
#33231=CARTESIAN_POINT('Origin',(0.,0.,0.38));
#33232=CARTESIAN_POINT('',(3.32,-4.06582737316921E-16,0.38));
#33233=CARTESIAN_POINT('',(0.,0.,0.));
#33234=CARTESIAN_POINT('Origin',(0.,0.,-0.48));
#33235=CARTESIAN_POINT('',(-0.395253163807729,0.000335471986130265,-0.715584015536924));
#33236=CARTESIAN_POINT('',(-0.395255438336,0.000332125708880706,-0.726115984463077));
#33237=CARTESIAN_POINT('',(-0.3954,-4.84225344382863E-17,-0.48));
#33238=CARTESIAN_POINT('',(-0.395861479162046,-0.000213366483867161,-0.790584015536923));
#33239=CARTESIAN_POINT('Ctrl Pts',(-0.395253163807729,0.000335471986130265,
-0.715584015536924));
#33240=CARTESIAN_POINT('Ctrl Pts',(-0.395551653151419,0.0357534542470482,
-0.716652535192449));
#33241=CARTESIAN_POINT('Ctrl Pts',(-0.391174119565203,0.0710989968386545,
-0.717721054847974));
#33242=CARTESIAN_POINT('Ctrl Pts',(-0.381823957673672,0.105076140411834,
-0.718789574503499));
#33243=CARTESIAN_POINT('Ctrl Pts',(-0.347453343346403,0.22997400969405,
-0.722717386386032));
#33244=CARTESIAN_POINT('Ctrl Pts',(-0.2458899929036,0.336381360783369,-0.726645198268564));
#33245=CARTESIAN_POINT('Ctrl Pts',(-0.122725269859081,0.376524449371095,
-0.730573010151097));
#33246=CARTESIAN_POINT('Ctrl Pts',(0.000439453185439045,0.416667537958822,
-0.73450082203363));
#33247=CARTESIAN_POINT('Ctrl Pts',(0.145205548831676,0.390546364044954,
-0.738428633916163));
#33248=CARTESIAN_POINT('Ctrl Pts',(0.246571894502321,0.309893277568692,
-0.742356445798696));
#33249=CARTESIAN_POINT('Ctrl Pts',(0.347938240172965,0.229240191092431,
-0.746284257681229));
#33250=CARTESIAN_POINT('Ctrl Pts',(0.405904835868018,0.0940551920537777,
-0.750212069563761));
#33251=CARTESIAN_POINT('Ctrl Pts',(0.394465702582075,-0.0349816075370925,
-0.754139881446293));
#33252=CARTESIAN_POINT('Ctrl Pts',(0.383026569296131,-0.164018407127964,
-0.758067693328826));
#33253=CARTESIAN_POINT('Ctrl Pts',(0.302181707029189,-0.286907007271051,
-0.76199550521136));
#33254=CARTESIAN_POINT('Ctrl Pts',(0.188191962309989,-0.348457576111146,
-0.765923317093893));
#33255=CARTESIAN_POINT('Ctrl Pts',(0.0742022175907893,-0.41000814495124,
-0.769851128976425));
#33256=CARTESIAN_POINT('Ctrl Pts',(-0.0729324095806676,-0.410220682488342,
-0.773778940858958));
#33257=CARTESIAN_POINT('Ctrl Pts',(-0.18709178097685,-0.349037578722476,
-0.77770675274149));
#33258=CARTESIAN_POINT('Ctrl Pts',(-0.301251152373033,-0.287854474956611,
-0.781634564624023));
#33259=CARTESIAN_POINT('Ctrl Pts',(-0.382435267993942,-0.165275729887777,
-0.785562376506555));
#33260=CARTESIAN_POINT('Ctrl Pts',(-0.394322160558364,-0.0362597276125358,
-0.789490188389088));
#33261=CARTESIAN_POINT('Ctrl Pts',(-0.395425591355561,-0.0242834916475591,
-0.789854797438367));
#33262=CARTESIAN_POINT('Ctrl Pts',(-0.395931891509389,-0.0122517861649356,
-0.790219406487645));
#33263=CARTESIAN_POINT('Ctrl Pts',(-0.395861479162046,-0.000213366483867161,
-0.790584015536923));
#33264=CARTESIAN_POINT('',(-0.3954,-4.84225344382863E-17,-0.9646));
#33265=CARTESIAN_POINT('',(-0.3954,-4.84225344382863E-17,-0.48));
#33266=CARTESIAN_POINT('Origin',(0.,0.,-0.9646));
#33267=CARTESIAN_POINT('',(-0.278857777366742,0.281064285032673,-0.800000000000001));
#33268=CARTESIAN_POINT('Ctrl Pts',(-0.395861479162046,-0.000213366483867161,
-0.790584015536923));
#33269=CARTESIAN_POINT('Ctrl Pts',(-0.39525534905282,0.10341687610184,-0.793722677024616));
#33270=CARTESIAN_POINT('Ctrl Pts',(-0.351913261714371,0.207544658964529,
-0.796861338512308));
#33271=CARTESIAN_POINT('Ctrl Pts',(-0.278859905177388,0.28106907114812,
-0.800000000000001));
#33272=CARTESIAN_POINT('',(-0.393673192958032,-0.0369131026361662,-0.8));
#33273=CARTESIAN_POINT('Origin',(0.,0.,-0.8));
#33274=CARTESIAN_POINT('Ctrl Pts',(-0.393673192958032,-0.0369131026361654,
-0.8));
#33275=CARTESIAN_POINT('Ctrl Pts',(-0.381526729866673,-0.166453470874879,
-0.796072188117467));
#33276=CARTESIAN_POINT('Ctrl Pts',(-0.300626129406055,-0.288465681742495,
-0.792144376234934));
#33277=CARTESIAN_POINT('Ctrl Pts',(-0.186505338687462,-0.349319299154459,
-0.788216564352402));
#33278=CARTESIAN_POINT('Ctrl Pts',(-0.0723845479688678,-0.410172916566423,
-0.784288752469869));
#33279=CARTESIAN_POINT('Ctrl Pts',(0.0749564330077028,-0.409867940522735,
-0.780360940587336));
#33280=CARTESIAN_POINT('Ctrl Pts',(0.188884746658086,-0.348150998874613,
-0.776433128704804));
#33281=CARTESIAN_POINT('Ctrl Pts',(0.302813060308468,-0.286434057226491,
-0.772505316822271));
#33282=CARTESIAN_POINT('Ctrl Pts',(0.383328706632664,-0.163305149973936,
-0.768577504939738));
#33283=CARTESIAN_POINT('Ctrl Pts',(0.394503823024529,-0.0342255654622517,
-0.764649693057205));
#33284=CARTESIAN_POINT('Ctrl Pts',(0.405678939416394,0.0948540190494324,
-0.760721881174672));
#33285=CARTESIAN_POINT('Ctrl Pts',(0.347513525875929,0.229884280820245,
-0.756794069292139));
#33286=CARTESIAN_POINT('Ctrl Pts',(0.246010089847033,0.310337863189681,
-0.752866257409607));
#33287=CARTESIAN_POINT('Ctrl Pts',(0.144506653818137,0.390791445559116,
-0.748938445527074));
#33288=CARTESIAN_POINT('Ctrl Pts',(-0.000334804699189922,0.416668348527174,
-0.745010633644541));
#33289=CARTESIAN_POINT('Ctrl Pts',(-0.12343126021814,0.376302547448928,
-0.741082821762008));
#33290=CARTESIAN_POINT('Ctrl Pts',(-0.24652771573709,0.335936746370681,
-0.737155009879476));
#33291=CARTESIAN_POINT('Ctrl Pts',(-0.347879168257662,0.22932824124613,
-0.733227197996943));
#33292=CARTESIAN_POINT('Ctrl Pts',(-0.382014496854013,0.104363742597582,
-0.72929938611441));
#33293=CARTESIAN_POINT('Ctrl Pts',(-0.391236464425464,0.070603453726573,
-0.728238252230632));
#33294=CARTESIAN_POINT('Ctrl Pts',(-0.395552602268709,0.035503436030642,
-0.727177118346855));
#33295=CARTESIAN_POINT('Ctrl Pts',(-0.395255438336,0.000332125708880706,
-0.726115984463077));
#33296=CARTESIAN_POINT('Origin',(0.,0.,-0.48));
#33297=CARTESIAN_POINT('',(-0.394965714787616,-0.000250953455007918,-0.640584015536923));
#33298=CARTESIAN_POINT('',(-0.394960834327206,-0.000248313920574979,-0.651115984463077));
#33299=CARTESIAN_POINT('',(-0.3954,-4.84225344382863E-17,-0.48));
#33300=CARTESIAN_POINT('Ctrl Pts',(-0.394965714787616,-0.000250953455007918,
-0.640584015536923));
#33301=CARTESIAN_POINT('Ctrl Pts',(-0.394471046036972,0.0828241788087287,
-0.643085663897252));
#33302=CARTESIAN_POINT('Ctrl Pts',(-0.368812762630574,0.166178887533591,
-0.64558731225758));
#33303=CARTESIAN_POINT('Ctrl Pts',(-0.320289765331127,0.232906929873211,
-0.648088960617908));
#33304=CARTESIAN_POINT('Ctrl Pts',(-0.244104315612744,0.337675930087654,
-0.652016772500441));
#33305=CARTESIAN_POINT('Ctrl Pts',(-0.111553205064048,0.401457186366483,
-0.655944584382975));
#33306=CARTESIAN_POINT('Ctrl Pts',(0.0178556785537009,0.395616446478012,
-0.659872396265507));
#33307=CARTESIAN_POINT('Ctrl Pts',(0.14726456217145,0.389775706589541,-0.66380020814804));
#33308=CARTESIAN_POINT('Ctrl Pts',(0.27353121885825,0.314312970533769,-0.667728020030573));
#33309=CARTESIAN_POINT('Ctrl Pts',(0.339968835940365,0.203106870469053,
-0.671655831913105));
#33310=CARTESIAN_POINT('Ctrl Pts',(0.40640645302248,0.091900770404338,-0.675583643795638));
#33311=CARTESIAN_POINT('Ctrl Pts',(0.413015030499909,-0.0550486936693204,
-0.679511455678171));
#33312=CARTESIAN_POINT('Ctrl Pts',(0.356828054007659,-0.171769696291924,
-0.683439267560704));
#33313=CARTESIAN_POINT('Ctrl Pts',(0.300641077515409,-0.288490698914528,
-0.687367079443237));
#33314=CARTESIAN_POINT('Ctrl Pts',(0.181658547053481,-0.374983240086078,
-0.691294891325769));
#33315=CARTESIAN_POINT('Ctrl Pts',(0.0532962243198568,-0.392416631099017,
-0.695222703208302));
#33316=CARTESIAN_POINT('Ctrl Pts',(-0.0750660984137688,-0.409850022111956,
-0.699150515090834));
#33317=CARTESIAN_POINT('Ctrl Pts',(-0.212808213419091,-0.358224262966283,
-0.703078326973367));
#33318=CARTESIAN_POINT('Ctrl Pts',(-0.298090331815884,-0.260717189655889,
-0.7070061388559));
#33319=CARTESIAN_POINT('Ctrl Pts',(-0.360172352423616,-0.189735883744952,
-0.709865431082908));
#33320=CARTESIAN_POINT('Ctrl Pts',(-0.394454424864704,-0.0944408485534943,
-0.712724723309916));
#33321=CARTESIAN_POINT('Ctrl Pts',(-0.395253163807729,0.000335471986130265,
-0.715584015536924));
#33322=CARTESIAN_POINT('Ctrl Pts',(-0.395255438336,0.000332125708880706,
-0.726115984463077));
#33323=CARTESIAN_POINT('Ctrl Pts',(-0.394452643023416,-0.0946839915107613,
-0.723249306464322));
#33324=CARTESIAN_POINT('Ctrl Pts',(-0.35998091681832,-0.190220418610138,
-0.720382628465567));
#33325=CARTESIAN_POINT('Ctrl Pts',(-0.297607838874384,-0.261268242344166,
-0.717515950466812));
#33326=CARTESIAN_POINT('Ctrl Pts',(-0.212146647626277,-0.358615236464823,
-0.713588138584279));
#33327=CARTESIAN_POINT('Ctrl Pts',(-0.0743050604579336,-0.409988732533595,
-0.709660326701746));
#33328=CARTESIAN_POINT('Ctrl Pts',(0.054025596928822,-0.392317937929058,
-0.705732514819213));
#33329=CARTESIAN_POINT('Ctrl Pts',(0.182356254315577,-0.37464714332452,
-0.70180470293668));
#33330=CARTESIAN_POINT('Ctrl Pts',(0.301175981920744,-0.287932058046674,
-0.697876891054148));
#33331=CARTESIAN_POINT('Ctrl Pts',(0.357145708980789,-0.171106530935462,
-0.693949079171615));
#33332=CARTESIAN_POINT('Ctrl Pts',(0.413115436040835,-0.0542810038242487,
-0.690021267289082));
#33333=CARTESIAN_POINT('Ctrl Pts',(0.406235162555757,0.0926549651203302,
-0.686093455406549));
#33334=CARTESIAN_POINT('Ctrl Pts',(0.339591493502025,0.20373731066395,-0.682165643524016));
#33335=CARTESIAN_POINT('Ctrl Pts',(0.272947824448293,0.314819656207569,
-0.678237831641484));
#33336=CARTESIAN_POINT('Ctrl Pts',(0.146540759825906,0.39004837835023,-0.674310019758951));
#33337=CARTESIAN_POINT('Ctrl Pts',(0.0171211347676443,0.395649013122802,
-0.670382207876419));
#33338=CARTESIAN_POINT('Ctrl Pts',(-0.112298490290618,0.401249647895373,
-0.666454395993886));
#33339=CARTESIAN_POINT('Ctrl Pts',(-0.244730675784755,0.337222195297856,
-0.662526584111353));
#33340=CARTESIAN_POINT('Ctrl Pts',(-0.320721441453192,0.232311902261895,
-0.65859877222882));
#33341=CARTESIAN_POINT('Ctrl Pts',(-0.368977551866046,0.165691140651501,
-0.656104509640239));
#33342=CARTESIAN_POINT('Ctrl Pts',(-0.394473208494698,0.0825840467829949,
-0.653610247051658));
#33343=CARTESIAN_POINT('Ctrl Pts',(-0.394960834327206,-0.000248313920574979,
-0.651115984463077));
#33344=CARTESIAN_POINT('Origin',(0.,0.,-0.48));
#33345=CARTESIAN_POINT('',(-0.39601914064734,4.10564873420969E-6,-0.565584015536924));
#33346=CARTESIAN_POINT('',(-0.396019157300021,-2.47054920110875E-7,-0.576115984463077));
#33347=CARTESIAN_POINT('',(-0.3954,-4.84225344382863E-17,-0.48));
#33348=CARTESIAN_POINT('Ctrl Pts',(-0.396019115773222,4.10548378882781E-6,
-0.565584015536924));
#33349=CARTESIAN_POINT('Ctrl Pts',(-0.396039459492,0.129774468910247,-0.569518792602056));
#33350=CARTESIAN_POINT('Ctrl Pts',(-0.326064226544098,0.259525796747945,
-0.573453569667187));
#33351=CARTESIAN_POINT('Ctrl Pts',(-0.217650027597511,0.330846869196683,
-0.577388346732319));
#33352=CARTESIAN_POINT('Ctrl Pts',(-0.109427739064012,0.402041691978786,
-0.581316158614852));
#33353=CARTESIAN_POINT('Ctrl Pts',(0.0370973536411718,0.415012938357412,
-0.585243970497384));
#33354=CARTESIAN_POINT('Ctrl Pts',(0.156143733414188,0.363937247625334,
-0.589171782379917));
#33355=CARTESIAN_POINT('Ctrl Pts',(0.275190113187202,0.312861556893256,
-0.59309959426245));
#33356=CARTESIAN_POINT('Ctrl Pts',(0.366757780028048,0.197738929050475,
-0.597027406144982));
#33357=CARTESIAN_POINT('Ctrl Pts',(0.389738001674511,0.0702529463705541,
-0.600955218027515));
#33358=CARTESIAN_POINT('Ctrl Pts',(0.412718223320974,-0.0572330363093691,
-0.604883029910048));
#33359=CARTESIAN_POINT('Ctrl Pts',(0.367110999773051,-0.197082373826433,
-0.608810841792581));
#33360=CARTESIAN_POINT('Ctrl Pts',(0.27339141480735,-0.286510589711546,
-0.612738653675114));
#33361=CARTESIAN_POINT('Ctrl Pts',(0.179671829841651,-0.375938805596657,
-0.616666465557647));
#33362=CARTESIAN_POINT('Ctrl Pts',(0.0378398834581742,-0.414945899849817,
-0.620594277440179));
#33363=CARTESIAN_POINT('Ctrl Pts',(-0.0884298780502877,-0.386019874399458,
-0.624522089322712));
#33364=CARTESIAN_POINT('Ctrl Pts',(-0.21469963955875,-0.357093848949099,
-0.628449901205245));
#33365=CARTESIAN_POINT('Ctrl Pts',(-0.325407216192197,-0.260234703795221,
-0.632377713087778));
#33366=CARTESIAN_POINT('Ctrl Pts',(-0.370851110064887,-0.138926759143254,
-0.63630552497031));
#33367=CARTESIAN_POINT('Ctrl Pts',(-0.387351499005705,-0.0948806156948923,
-0.637731688492515));
#33368=CARTESIAN_POINT('Ctrl Pts',(-0.395247720260061,-0.0476112160385504,
-0.639157852014719));
#33369=CARTESIAN_POINT('Ctrl Pts',(-0.394965714787616,-0.000250953455007918,
-0.640584015536923));
#33370=CARTESIAN_POINT('Ctrl Pts',(-0.394960834327206,-0.000248313920574979,
-0.651115984463077));
#33371=CARTESIAN_POINT('Ctrl Pts',(-0.395241091775281,-0.0478552791000078,
-0.649682435169125));
#33372=CARTESIAN_POINT('Ctrl Pts',(-0.387260581472885,-0.0953714931568358,
-0.648248885875173));
#33373=CARTESIAN_POINT('Ctrl Pts',(-0.37059260016416,-0.139614862151827,
-0.646815336581222));
#33374=CARTESIAN_POINT('Ctrl Pts',(-0.324923647363953,-0.260838200055182,
-0.642887524698689));
#33375=CARTESIAN_POINT('Ctrl Pts',(-0.214036395920803,-0.357491742387486,
-0.638959712816156));
#33376=CARTESIAN_POINT('Ctrl Pts',(-0.0877131492638707,-0.386183345199099,
-0.635031900933623));
#33377=CARTESIAN_POINT('Ctrl Pts',(0.0386100973930622,-0.414874948010711,
-0.63110408905109));
#33378=CARTESIAN_POINT('Ctrl Pts',(0.180369339263778,-0.375604611301632,
-0.627176277168558));
#33379=CARTESIAN_POINT('Ctrl Pts',(0.273922744458712,-0.286002581116925,
-0.623248465286025));
#33380=CARTESIAN_POINT('Ctrl Pts',(0.367476149653647,-0.196400550932217,
-0.619320653403493));
#33381=CARTESIAN_POINT('Ctrl Pts',(0.412823718172801,-0.0564668272718801,
-0.615392841520959));
#33382=CARTESIAN_POINT('Ctrl Pts',(0.389606897901208,0.070976263805676,
-0.611465029638427));
#33383=CARTESIAN_POINT('Ctrl Pts',(0.366390077629615,0.198419354883232,
-0.607537217755894));
#33384=CARTESIAN_POINT('Ctrl Pts',(0.274608868567275,0.313371813378008,
-0.603609405873361));
#33385=CARTESIAN_POINT('Ctrl Pts',(0.155467891744039,0.364226435131106,
-0.599681593990828));
#33386=CARTESIAN_POINT('Ctrl Pts',(0.0363269149208032,0.415081056884205,
-0.595753782108295));
#33387=CARTESIAN_POINT('Ctrl Pts',(-0.110173829663326,0.401837841895627,
-0.591825970225762));
#33388=CARTESIAN_POINT('Ctrl Pts',(-0.21826376648398,0.330442259074028,
-0.58789815834323));
#33389=CARTESIAN_POINT('Ctrl Pts',(-0.326342129060288,0.259054321274205,
-0.583970767049845));
#33390=CARTESIAN_POINT('Ctrl Pts',(-0.396017909472745,0.129526468857604,
-0.580043375756461));
#33391=CARTESIAN_POINT('Ctrl Pts',(-0.396019142095646,-2.47048853291312E-7,
-0.576115984463077));
#33392=CARTESIAN_POINT('Origin',(0.,0.,-0.48));
#33393=CARTESIAN_POINT('',(-0.394956676078496,0.000245896443633459,-0.490584015536923));
#33394=CARTESIAN_POINT('',(-0.394961414894976,0.000248589851300403,-0.501115984463076));
#33395=CARTESIAN_POINT('',(-0.3954,-4.84225344382863E-17,-0.48));
#33396=CARTESIAN_POINT('Ctrl Pts',(-0.394956676078496,0.000245896443633459,
-0.490584015536923));
#33397=CARTESIAN_POINT('Ctrl Pts',(-0.395235276024708,0.0480715230603383,
-0.492024109424326));
#33398=CARTESIAN_POINT('Ctrl Pts',(-0.387179611885601,0.0958065206795767,
-0.493464203311728));
#33399=CARTESIAN_POINT('Ctrl Pts',(-0.370362436155785,0.140224290031149,
-0.49490429719913));
#33400=CARTESIAN_POINT('Ctrl Pts',(-0.324494105458702,0.261372392790905,
-0.498832109081663));
#33401=CARTESIAN_POINT('Ctrl Pts',(-0.213448111654675,0.357843339760786,
-0.502759920964196));
#33402=CARTESIAN_POINT('Ctrl Pts',(-0.0870778555314957,0.386327105829989,
-0.506687732846729));
#33403=CARTESIAN_POINT('Ctrl Pts',(0.0392924005916832,0.414810871899191,
-0.510615544729262));
#33404=CARTESIAN_POINT('Ctrl Pts',(0.180986919034015,0.375307457067717,
-0.514543356611794));
#33405=CARTESIAN_POINT('Ctrl Pts',(0.274392836624718,0.285551671039299,
-0.518471168494327));
#33406=CARTESIAN_POINT('Ctrl Pts',(0.367798754215423,0.19579588501088,-0.52239898037686));
#33407=CARTESIAN_POINT('Ctrl Pts',(0.412916070954497,0.0557877277855151,
-0.526326792259393));
#33408=CARTESIAN_POINT('Ctrl Pts',(0.389489651066459,-0.0716170186429137,
-0.530254604141926));
#33409=CARTESIAN_POINT('Ctrl Pts',(0.366063231178422,-0.19902176507134,
-0.534182416024458));
#33410=CARTESIAN_POINT('Ctrl Pts',(0.274093074663277,-0.31382310070283,
-0.538110227906991));
#33411=CARTESIAN_POINT('Ctrl Pts',(0.154868605220906,-0.36448168775808,
-0.542038039789524));
#33412=CARTESIAN_POINT('Ctrl Pts',(0.0356441357785338,-0.415140274813329,
-0.545965851672056));
#33413=CARTESIAN_POINT('Ctrl Pts',(-0.110834646591064,-0.401656113292336,
-0.549893663554589));
#33414=CARTESIAN_POINT('Ctrl Pts',(-0.218807013758192,-0.330082832562713,
-0.553821475437122));
#33415=CARTESIAN_POINT('Ctrl Pts',(-0.326587913697395,-0.258636472618604,
-0.557742322137056));
#33416=CARTESIAN_POINT('Ctrl Pts',(-0.395998844077695,-0.129306829485993,
-0.56166316883699));
#33417=CARTESIAN_POINT('Ctrl Pts',(-0.396019115773222,4.10548378882781E-6,
-0.565584015536924));
#33418=CARTESIAN_POINT('Ctrl Pts',(-0.396019142095646,-2.47048853291312E-7,
-0.576115984463077));
#33419=CARTESIAN_POINT('Ctrl Pts',(-0.396020374982553,-0.129554705304902,
-0.572187751991396));
#33420=CARTESIAN_POINT('Ctrl Pts',(-0.326310510095658,-0.259108025856776,
-0.568259519519714));
#33421=CARTESIAN_POINT('Ctrl Pts',(-0.218193903826923,-0.330488397181274,
-0.564331287048033));
#33422=CARTESIAN_POINT('Ctrl Pts',(-0.11008887341875,-0.401861125931206,
-0.5604034751655));
#33423=CARTESIAN_POINT('Ctrl Pts',(0.0364146738056535,-0.415073361743801,
-0.556475663282968));
#33424=CARTESIAN_POINT('Ctrl Pts',(0.155544893218128,-0.364193555966734,
-0.552547851400435));
#33425=CARTESIAN_POINT('Ctrl Pts',(0.274675112630603,-0.313313750189668,
-0.548620039517903));
#33426=CARTESIAN_POINT('Ctrl Pts',(0.366432004231147,-0.198341902822938,
-0.544692227635369));
#33427=CARTESIAN_POINT('Ctrl Pts',(0.389621887462813,-0.0708939010958812,
-0.540764415752836));
#33428=CARTESIAN_POINT('Ctrl Pts',(0.412811770694479,0.056554100631176,
-0.536836603870304));
#33429=CARTESIAN_POINT('Ctrl Pts',(0.367434645557268,0.196478256718561,
-0.532908791987771));
#33430=CARTESIAN_POINT('Ctrl Pts',(0.273862287592234,0.286060496577444,
-0.528980980105239));
#33431=CARTESIAN_POINT('Ctrl Pts',(0.1802899296272,0.375642736436327,-0.525053168222706));
#33432=CARTESIAN_POINT('Ctrl Pts',(0.0385223388343421,0.414883060066708,
-0.521125356340173));
#33433=CARTESIAN_POINT('Ctrl Pts',(-0.0877948164623846,0.386164771103267,
-0.51719754445764));
#33434=CARTESIAN_POINT('Ctrl Pts',(-0.214111971759111,0.357446482139827,
-0.513269732575107));
#33435=CARTESIAN_POINT('Ctrl Pts',(-0.324978691559707,0.260769580582567,
-0.509341920692574));
#33436=CARTESIAN_POINT('Ctrl Pts',(-0.370622058898363,0.139536553455912,
-0.505414108810041));
#33437=CARTESIAN_POINT('Ctrl Pts',(-0.387270927216809,0.0953156113527008,
-0.503981400694386));
#33438=CARTESIAN_POINT('Ctrl Pts',(-0.395241844399756,0.0478274827323181,
-0.502548692578731));
#33439=CARTESIAN_POINT('Ctrl Pts',(-0.394961414894976,0.000248589851300403,
-0.501115984463076));
#33440=CARTESIAN_POINT('Origin',(0.,0.,-0.48));
#33441=CARTESIAN_POINT('',(-0.395266933374857,-0.000337325613274597,-0.415584015536924));
#33442=CARTESIAN_POINT('',(-0.395260053944926,-0.00033663270935099,-0.426115984463076));
#33443=CARTESIAN_POINT('',(-0.3954,-4.84225344382863E-17,-0.48));
#33444=CARTESIAN_POINT('Ctrl Pts',(-0.395266933374857,-0.000337325613274597,
-0.415584015536924));
#33445=CARTESIAN_POINT('Ctrl Pts',(-0.394458698757483,0.0948929263788777,
-0.418457238129129));
#33446=CARTESIAN_POINT('Ctrl Pts',(-0.359809398953095,0.190651033176329,
-0.421330460721335));
#33447=CARTESIAN_POINT('Ctrl Pts',(-0.297175326236494,0.261759452748588,
-0.42420368331354));
#33448=CARTESIAN_POINT('Ctrl Pts',(-0.211552007063425,0.358967547972998,
-0.428131495196073));
#33449=CARTESIAN_POINT('Ctrl Pts',(-0.0736307456486751,0.41011030892357,
-0.432059307078606));
#33450=CARTESIAN_POINT('Ctrl Pts',(0.0546695748141089,0.392227514609258,
-0.435987118961139));
#33451=CARTESIAN_POINT('Ctrl Pts',(0.182969895276892,0.374344720294945,
-0.439914930843672));
#33452=CARTESIAN_POINT('Ctrl Pts',(0.301649274787709,0.287436370715749,
-0.443842742726204));
#33453=CARTESIAN_POINT('Ctrl Pts',(0.357427352060231,0.170519423016928,
-0.447770554608737));
#33454=CARTESIAN_POINT('Ctrl Pts',(0.413205429332753,0.0536024753181058,
-0.45169836649127));
#33455=CARTESIAN_POINT('Ctrl Pts',(0.40608220436698,-0.0933230705003415,
-0.455626178373802));
#33456=CARTESIAN_POINT('Ctrl Pts',(0.339255604225498,-0.204295914371732,
-0.459553990256335));
#33457=CARTESIAN_POINT('Ctrl Pts',(0.272429004084016,-0.315268758243122,
-0.463481802138868));
#33458=CARTESIAN_POINT('Ctrl Pts',(0.145899028766824,-0.390288900167456,
-0.467409614021401));
#33459=CARTESIAN_POINT('Ctrl Pts',(0.0164705151944307,-0.395676519085635,
-0.471337425903934));
#33460=CARTESIAN_POINT('Ctrl Pts',(-0.112957998377962,-0.401064138003814,
-0.475265237786467));
#33461=CARTESIAN_POINT('Ctrl Pts',(-0.245285050205555,-0.33681923391584,
-0.479193049668999));
#33462=CARTESIAN_POINT('Ctrl Pts',(-0.321103242324281,-0.231784152597038,
-0.483120861551532));
#33463=CARTESIAN_POINT('Ctrl Pts',(-0.369123434363212,-0.165259158597507,
-0.485608579546663));
#33464=CARTESIAN_POINT('Ctrl Pts',(-0.394475403221431,-0.0823714058055866,
-0.488096297541793));
#33465=CARTESIAN_POINT('Ctrl Pts',(-0.394956676078496,0.000245896443633459,
-0.490584015536923));
#33466=CARTESIAN_POINT('Ctrl Pts',(-0.394961414894976,0.000248589851300403,
-0.501115984463076));
#33467=CARTESIAN_POINT('Ctrl Pts',(-0.394473038577377,-0.0826114662579111,
-0.498620880696199));
#33468=CARTESIAN_POINT('Ctrl Pts',(-0.368958940221529,-0.165746803632547,
-0.496125776929321));
#33469=CARTESIAN_POINT('Ctrl Pts',(-0.320672414820748,-0.232379781053294,
-0.493630673162443));
#33470=CARTESIAN_POINT('Ctrl Pts',(-0.244659388527761,-0.337273935739795,
-0.489702861279911));
#33471=CARTESIAN_POINT('Ctrl Pts',(-0.11221332106507,-0.401273092416749,
-0.485775049397377));
#33472=CARTESIAN_POINT('Ctrl Pts',(0.0172049583135898,-0.395645232092361,
-0.481847237514845));
#33473=CARTESIAN_POINT('Ctrl Pts',(0.14662323769225,-0.390017371767973,
-0.477919425632312));
#33474=CARTESIAN_POINT('Ctrl Pts',(0.273013728986881,-0.314762494442241,
-0.473991613749779));
#33475=CARTESIAN_POINT('Ctrl Pts',(0.339634215735493,-0.203665804142061,
-0.470063801867247));
#33476=CARTESIAN_POINT('Ctrl Pts',(0.406254702484105,-0.092569113841881,
-0.466135989984714));
#33477=CARTESIAN_POINT('Ctrl Pts',(0.413105184686698,0.0543693894327481,
-0.462208178102181));
#33478=CARTESIAN_POINT('Ctrl Pts',(0.357110181438081,0.171182588438861,
-0.458280366219648));
#33479=CARTESIAN_POINT('Ctrl Pts',(0.301115178189463,0.287995787444972,
-0.454352554337115));
#33480=CARTESIAN_POINT('Ctrl Pts',(0.182274689489637,0.374683682182567,
-0.450424742454583));
#33481=CARTESIAN_POINT('Ctrl Pts',(0.0539414055779334,0.392328287325614,
-0.44649693057205));
#33482=CARTESIAN_POINT('Ctrl Pts',(-0.0743918783337699,0.409972892468661,
-0.442569118689517));
#33483=CARTESIAN_POINT('Ctrl Pts',(-0.212217957457349,0.35857420801716,
-0.438641306806984));
#33484=CARTESIAN_POINT('Ctrl Pts',(-0.297660680088029,0.261207350206704,
-0.434713494924451));
#33485=CARTESIAN_POINT('Ctrl Pts',(-0.360001980506246,0.190165881177487,
-0.431847658103993));
#33486=CARTESIAN_POINT('Ctrl Pts',(-0.394456725068691,0.0946530128377653,
-0.428981821283535));
#33487=CARTESIAN_POINT('Ctrl Pts',(-0.395260053944926,-0.00033663270935099,
-0.426115984463076));
#33488=CARTESIAN_POINT('Origin',(0.,0.,-0.48));
#33489=CARTESIAN_POINT('',(-0.395875933213339,0.00020569453982186,-0.340584015536923));
#33490=CARTESIAN_POINT('',(-0.395880924684652,0.000202294883939828,-0.351115984463076));
#33491=CARTESIAN_POINT('',(-0.3954,-4.84225344382863E-17,-0.48));
#33492=CARTESIAN_POINT('Ctrl Pts',(-0.395875933213339,0.00020569453982186,
-0.340584015536923));
#33493=CARTESIAN_POINT('Ctrl Pts',(-0.39595581585693,0.0127020976124944,
-0.340962554951399));
#33494=CARTESIAN_POINT('Ctrl Pts',(-0.395414255679657,0.0251914927215432,
-0.341341094365876));
#33495=CARTESIAN_POINT('Ctrl Pts',(-0.394228317772475,0.0376193978231643,
-0.341719633780352));
#33496=CARTESIAN_POINT('Ctrl Pts',(-0.38192275373967,0.166574194777889,
-0.345647445662884));
#33497=CARTESIAN_POINT('Ctrl Pts',(-0.30023952618032,0.288908599922735,
-0.349575257545417));
#33498=CARTESIAN_POINT('Ctrl Pts',(-0.185849806556546,0.349701351197546,
-0.35350306942795));
#33499=CARTESIAN_POINT('Ctrl Pts',(-0.0714600869327725,0.410494102472356,
-0.357430881310483));
#33500=CARTESIAN_POINT('Ctrl Pts',(0.0756361247554245,0.409745199877132,
-0.361358693193016));
#33501=CARTESIAN_POINT('Ctrl Pts',(0.189400909071263,0.347790858520418,
-0.365286505075549));
#33502=CARTESIAN_POINT('Ctrl Pts',(0.303165693387101,0.285836517163703,
-0.369214316958082));
#33503=CARTESIAN_POINT('Ctrl Pts',(0.383599050330581,0.162676737045497,
-0.373142128840614));
#33504=CARTESIAN_POINT('Ctrl Pts',(0.394590929992081,0.0336033271388246,
-0.377069940723147));
#33505=CARTESIAN_POINT('Ctrl Pts',(0.405582809653581,-0.0954700827678465,
-0.38099775260568));
#33506=CARTESIAN_POINT('Ctrl Pts',(0.347133212033103,-0.230457122462983,
-0.384925564488213));
#33507=CARTESIAN_POINT('Ctrl Pts',(0.245482716505811,-0.310756209147683,
-0.388853376370745));
#33508=CARTESIAN_POINT('Ctrl Pts',(0.143832220978519,-0.391055295832382,
-0.392781188253278));
#33509=CARTESIAN_POINT('Ctrl Pts',(-0.00101917245558511,-0.416666429506645,
-0.396709000135811));
#33510=CARTESIAN_POINT('Ctrl Pts',(-0.124041341403078,-0.376091652725678,
-0.400636812018344));
#33511=CARTESIAN_POINT('Ctrl Pts',(-0.247063510350573,-0.33551687594471,
-0.404564623900876));
#33512=CARTESIAN_POINT('Ctrl Pts',(-0.348256454811456,-0.228756188708513,
-0.408492435783409));
#33513=CARTESIAN_POINT('Ctrl Pts',(-0.382190238576203,-0.10373913034129,
-0.412420247665942));
#33514=CARTESIAN_POINT('Ctrl Pts',(-0.391301215885916,-0.0701729477426301,
-0.413474836956269));
#33515=CARTESIAN_POINT('Ctrl Pts',(-0.395563588278611,-0.0352906926578339,
-0.414529426246596));
#33516=CARTESIAN_POINT('Ctrl Pts',(-0.395266933374857,-0.000337325613274597,
-0.415584015536924));
#33517=CARTESIAN_POINT('Ctrl Pts',(-0.395260053944926,-0.00033663270935099,
-0.426115984463076));
#33518=CARTESIAN_POINT('Ctrl Pts',(-0.39555773845617,-0.0355363461076123,
-0.425054009401002));
#33519=CARTESIAN_POINT('Ctrl Pts',(-0.39123449647611,-0.0706642118877601,
-0.423992034338928));
#33520=CARTESIAN_POINT('Ctrl Pts',(-0.381996983921461,-0.104448382212464,
-0.422930059276853));
#33521=CARTESIAN_POINT('Ctrl Pts',(-0.347831198986433,-0.229402225651767,
-0.41900224739432));
#33522=CARTESIAN_POINT('Ctrl Pts',(-0.246440262978595,-0.335974881360961,
-0.415074435511788));
#33523=CARTESIAN_POINT('Ctrl Pts',(-0.123342999167154,-0.376321225588517,
-0.411146623629255));
#33524=CARTESIAN_POINT('Ctrl Pts',(-0.000245735355712692,-0.416667569816073,
-0.407218811746722));
#33525=CARTESIAN_POINT('Ctrl Pts',(0.144557856259332,-0.390787602561992,
-0.403290999864189));
#33526=CARTESIAN_POINT('Ctrl Pts',(0.246059113610558,-0.310299972415847,
-0.399363187981656));
#33527=CARTESIAN_POINT('Ctrl Pts',(0.347560370961784,-0.229812342269703,
-0.395435376099124));
#33528=CARTESIAN_POINT('Ctrl Pts',(0.405759294049192,-0.0947170492314976,
-0.391507564216591));
#33529=CARTESIAN_POINT('Ctrl Pts',(0.394527842253011,0.0343357242411698,
-0.387579752334058));
#33530=CARTESIAN_POINT('Ctrl Pts',(0.383296390456831,0.163388497713835,
-0.383651940451526));
#33531=CARTESIAN_POINT('Ctrl Pts',(0.302634563777064,0.286398751620962,
-0.379724128568993));
#33532=CARTESIAN_POINT('Ctrl Pts',(0.188754982175704,0.34814180584345,-0.37579631668646));
#33533=CARTESIAN_POINT('Ctrl Pts',(0.0748754005743428,0.409884860065939,
-0.371868504803927));
#33534=CARTESIAN_POINT('Ctrl Pts',(-0.0722219359486128,0.410360714603788,
-0.367940692921395));
#33535=CARTESIAN_POINT('Ctrl Pts',(-0.186498602970298,0.349355737554315,
-0.364012881038862));
#33536=CARTESIAN_POINT('Ctrl Pts',(-0.300775269991983,0.288350760504841,
-0.360085069156329));
#33537=CARTESIAN_POINT('Ctrl Pts',(-0.382231267512398,0.165864951868046,
-0.356157257273796));
#33538=CARTESIAN_POINT('Ctrl Pts',(-0.394297437564028,0.0368875453552563,
-0.352229445391263));
#33539=CARTESIAN_POINT('Ctrl Pts',(-0.395437615124049,0.0246999875778991,
-0.351858291748534));
#33540=CARTESIAN_POINT('Ctrl Pts',(-0.395958206245996,0.0124544658863471,
-0.351487138105805));
#33541=CARTESIAN_POINT('Ctrl Pts',(-0.395880924684652,0.000202294883939828,
-0.351115984463076));
#33542=CARTESIAN_POINT('Origin',(0.,0.,-0.48));
#33543=CARTESIAN_POINT('',(-0.394796739701267,7.87737235064534E-5,-0.265584015536923));
#33544=CARTESIAN_POINT('',(-0.394798228541794,8.25237670084469E-5,-0.276115984463076));
#33545=CARTESIAN_POINT('',(-0.3954,-4.84225344382863E-17,-0.48));
#33546=CARTESIAN_POINT('Ctrl Pts',(-0.394796739701267,7.87737235064534E-5,
-0.265584015536923));
#33547=CARTESIAN_POINT('Ctrl Pts',(-0.394906225968879,0.0603056496953535,
-0.267395683656203));
#33548=CARTESIAN_POINT('Ctrl Pts',(-0.381947457713303,0.12048784623346,
-0.269207351775482));
#33549=CARTESIAN_POINT('Ctrl Pts',(-0.355672556193802,0.17414998820835,
-0.271019019894762));
#33550=CARTESIAN_POINT('Ctrl Pts',(-0.298706896036511,0.290492930189886,
-0.274946831777295));
#33551=CARTESIAN_POINT('Ctrl Pts',(-0.179148748818222,0.376188354397569,
-0.278874643659828));
#33552=CARTESIAN_POINT('Ctrl Pts',(-0.0506729928961993,0.392763839202375,
-0.28280245554236));
#33553=CARTESIAN_POINT('Ctrl Pts',(0.0778027630258239,0.409339324007181,
-0.286730267424893));
#33554=CARTESIAN_POINT('Ctrl Pts',(0.215196127651582,0.356794869409109,
-0.290658079307426));
#33555=CARTESIAN_POINT('Ctrl Pts',(0.299825213644828,0.258719977794535,
-0.294585891189959));
#33556=CARTESIAN_POINT('Ctrl Pts',(0.384454299638073,0.160645086179963,
-0.298513703072491));
#33557=CARTESIAN_POINT('Ctrl Pts',(0.416319106998808,0.0170397575488902,
-0.302441514955024));
#33558=CARTESIAN_POINT('Ctrl Pts',(0.381114130844172,-0.107625298583498,
-0.306369326837557));
#33559=CARTESIAN_POINT('Ctrl Pts',(0.345909154689534,-0.23229035471589,
-0.31029713872009));
#33560=CARTESIAN_POINT('Ctrl Pts',(0.243634395019522,-0.338015138349596,
-0.314224950602622));
#33561=CARTESIAN_POINT('Ctrl Pts',(0.12020546215663,-0.377335172612692,
-0.318152762485155));
#33562=CARTESIAN_POINT('Ctrl Pts',(-0.00322347070625931,-0.416655206875788,
-0.322080574367688));
#33563=CARTESIAN_POINT('Ctrl Pts',(-0.147806576762028,-0.389570491768276,
-0.326008386250221));
#33564=CARTESIAN_POINT('Ctrl Pts',(-0.248634179536782,-0.30824053983222,
-0.329936198132754));
#33565=CARTESIAN_POINT('Ctrl Pts',(-0.339744610802606,-0.234748690459619,
-0.33348547060081));
#33566=CARTESIAN_POINT('Ctrl Pts',(-0.39512693520486,-0.116963450017949,
-0.337034743068867));
#33567=CARTESIAN_POINT('Ctrl Pts',(-0.395875933213339,0.00020569453982186,
-0.340584015536923));
#33568=CARTESIAN_POINT('Ctrl Pts',(-0.395880924684652,0.000202294883939828,
-0.351115984463076));
#33569=CARTESIAN_POINT('Ctrl Pts',(-0.395140357786489,-0.11720672373916,
-0.347559326223272));
#33570=CARTESIAN_POINT('Ctrl Pts',(-0.33949812433168,-0.235226337657232,
-0.344002667983469));
#33571=CARTESIAN_POINT('Ctrl Pts',(-0.248061560911564,-0.30870150999079,
-0.340446009743665));
#33572=CARTESIAN_POINT('Ctrl Pts',(-0.147083171624631,-0.389844154435259,
-0.336518197861132));
#33573=CARTESIAN_POINT('Ctrl Pts',(-0.00245005046792381,-0.416660438935413,
-0.332590385978599));
#33574=CARTESIAN_POINT('Ctrl Pts',(0.120905672129734,-0.37711136116329,
-0.328662574096066));
#33575=CARTESIAN_POINT('Ctrl Pts',(0.244261394727393,-0.337562283391168,
-0.324734762213533));
#33576=CARTESIAN_POINT('Ctrl Pts',(0.346339718766002,-0.231647843346768,
-0.320806950331001));
#33577=CARTESIAN_POINT('Ctrl Pts',(0.381313222445306,-0.106917662992341,
-0.316879138448468));
#33578=CARTESIAN_POINT('Ctrl Pts',(0.41628672612461,0.0178125173620851,
-0.312951326565936));
#33579=CARTESIAN_POINT('Ctrl Pts',(0.384155409444609,0.161358438026538,
-0.309023514683403));
#33580=CARTESIAN_POINT('Ctrl Pts',(0.299344425008715,0.259276060389882,
-0.30509570280087));
#33581=CARTESIAN_POINT('Ctrl Pts',(0.214533440572821,0.357193682753226,
-0.301167890918337));
#33582=CARTESIAN_POINT('Ctrl Pts',(0.0770427883810332,0.409483006815461,
-0.297240079035804));
#33583=CARTESIAN_POINT('Ctrl Pts',(-0.0514019676604196,0.392669069304711,
-0.293312267153272));
#33584=CARTESIAN_POINT('Ctrl Pts',(-0.179846723701874,0.375855131793961,
-0.289384455270739));
#33585=CARTESIAN_POINT('Ctrl Pts',(-0.299245583592994,0.289937932710224,
-0.285456643388206));
#33586=CARTESIAN_POINT('Ctrl Pts',(-0.355995179884672,0.173489458377813,
-0.281528831505673));
#33587=CARTESIAN_POINT('Ctrl Pts',(-0.382063713175179,0.119997607719336,
-0.279724549158141));
#33588=CARTESIAN_POINT('Ctrl Pts',(-0.394912485224089,0.0600632843804217,
-0.277920266810608));
#33589=CARTESIAN_POINT('Ctrl Pts',(-0.394798228541794,8.25237670084469E-5,
-0.276115984463076));
#33590=CARTESIAN_POINT('Origin',(0.,0.,-0.48));
#33591=CARTESIAN_POINT('',(-0.395622884157063,-0.00031191406896286,-0.190584015536923));
#33592=CARTESIAN_POINT('',(-0.395615927747866,-0.00031357059932876,-0.201115984463076));
#33593=CARTESIAN_POINT('',(-0.3954,-4.84225344382863E-17,-0.48));
#33594=CARTESIAN_POINT('Ctrl Pts',(-0.395622884157063,-0.00031191406896286,
-0.190584015536923));
#33595=CARTESIAN_POINT('Ctrl Pts',(-0.394695938484083,0.106985189615806,
-0.193828812361006));
#33596=CARTESIAN_POINT('Ctrl Pts',(-0.349385427645315,0.214972363562661,
-0.197073609185089));
#33597=CARTESIAN_POINT('Ctrl Pts',(-0.271471059019966,0.288330801125965,
-0.200318406009172));
#33598=CARTESIAN_POINT('Ctrl Pts',(-0.177156068128913,0.377130858068399,
-0.204246217891704));
#33599=CARTESIAN_POINT('Ctrl Pts',(-0.0350666671734208,0.41518945175117,
-0.208174029774237));
#33600=CARTESIAN_POINT('Ctrl Pts',(0.0910070087554293,0.385420430263643,
-0.21210184165677));
#33601=CARTESIAN_POINT('Ctrl Pts',(0.217080684684278,0.355651408776116,
-0.216029653539303));
#33602=CARTESIAN_POINT('Ctrl Pts',(0.327138635586484,0.258054772118293,
-0.219957465421836));
#33603=CARTESIAN_POINT('Ctrl Pts',(0.37177103208318,0.136445909161074,-0.223885277304369));
#33604=CARTESIAN_POINT('Ctrl Pts',(0.416403428579877,0.0148370462038541,
-0.227813089186901));
#33605=CARTESIAN_POINT('Ctrl Pts',(0.395610270671062,-0.130784043052762,
-0.231740901069434));
#33606=CARTESIAN_POINT('Ctrl Pts',(0.318726518102726,-0.235041682158158,
-0.235668712951967));
#33607=CARTESIAN_POINT('Ctrl Pts',(0.241842765534391,-0.339299321263555,
-0.2395965248345));
#33608=CARTESIAN_POINT('Ctrl Pts',(0.108868418306535,-0.402193510217731,
-0.243524336717033));
#33609=CARTESIAN_POINT('Ctrl Pts',(-0.0204985275777863,-0.39548830038016,
-0.247452148599566));
#33610=CARTESIAN_POINT('Ctrl Pts',(-0.149865473462107,-0.388783090542588,
-0.251379960482098));
#33611=CARTESIAN_POINT('Ctrl Pts',(-0.275625018002894,-0.312478481913271,
-0.255307772364631));
#33612=CARTESIAN_POINT('Ctrl Pts',(-0.34131820372514,-0.200830947720919,
-0.259235584247163));
#33613=CARTESIAN_POINT('Ctrl Pts',(-0.37671099477824,-0.140679840633938,
-0.261351728010417));
#33614=CARTESIAN_POINT('Ctrl Pts',(-0.394668852766622,-0.0702700537530919,
-0.26346787177367));
#33615=CARTESIAN_POINT('Ctrl Pts',(-0.394796739701267,7.87737235064534E-5,
-0.265584015536923));
#33616=CARTESIAN_POINT('Ctrl Pts',(-0.394798228541794,8.25237670084469E-5,
-0.276115984463076));
#33617=CARTESIAN_POINT('Ctrl Pts',(-0.394663755442417,-0.0705111484864399,
-0.273992454928076));
#33618=CARTESIAN_POINT('Ctrl Pts',(-0.376573096370534,-0.141169144930958,
-0.271868925393075));
#33619=CARTESIAN_POINT('Ctrl Pts',(-0.340944796447611,-0.201464155788848,
-0.269745395858075));
#33620=CARTESIAN_POINT('Ctrl Pts',(-0.275044484026637,-0.312989546042017,
-0.265817583975542));
#33621=CARTESIAN_POINT('Ctrl Pts',(-0.149143526492451,-0.389060576967273,
-0.261889772093009));
#33622=CARTESIAN_POINT('Ctrl Pts',(-0.019764367298066,-0.395525637632012,
-0.257961960210476));
#33623=CARTESIAN_POINT('Ctrl Pts',(0.109614791896319,-0.401990698296751,
-0.254034148327944));
#33624=CARTESIAN_POINT('Ctrl Pts',(0.242472152750905,-0.338849788700974,
-0.250106336445411));
#33625=CARTESIAN_POINT('Ctrl Pts',(0.31916223861105,-0.234449622972972,
-0.246178524562878));
#33626=CARTESIAN_POINT('Ctrl Pts',(0.395852324471197,-0.130049457244968,
-0.242250712680345));
#33627=CARTESIAN_POINT('Ctrl Pts',(0.416375135336902,0.0156099646152614,
-0.238322900797812));
#33628=CARTESIAN_POINT('Ctrl Pts',(0.37151708387966,0.137135760428241,-0.23439508891528));
#33629=CARTESIAN_POINT('Ctrl Pts',(0.326659032422418,0.258661556241219,
-0.230467277032747));
#33630=CARTESIAN_POINT('Ctrl Pts',(0.216420118642233,0.356053726006946,
-0.226539465150214));
#33631=CARTESIAN_POINT('Ctrl Pts',(0.0902914106015626,0.385588668383179,
-0.222611653267682));
#33632=CARTESIAN_POINT('Ctrl Pts',(-0.0358372974391088,0.415123610759413,
-0.218683841385149));
#33633=CARTESIAN_POINT('Ctrl Pts',(-0.177855799740265,0.376801325746151,
-0.214756029502616));
#33634=CARTESIAN_POINT('Ctrl Pts',(-0.272005784099203,0.287826360424576,
-0.210828217620083));
#33635=CARTESIAN_POINT('Ctrl Pts',(-0.349606801932139,0.214490736232845,
-0.207590806567747));
#33636=CARTESIAN_POINT('Ctrl Pts',(-0.394688285862518,0.106744154164166,
-0.204353395515412));
#33637=CARTESIAN_POINT('Ctrl Pts',(-0.395615927747866,-0.00031357059932876,
-0.201115984463076));
#33638=CARTESIAN_POINT('Origin',(0.,0.,-0.48));
#33639=CARTESIAN_POINT('',(-0.395559352324906,0.000325232430651398,-0.115584015536923));
#33640=CARTESIAN_POINT('',(-0.395566345080525,0.000324025114679023,-0.126115984463076));
#33641=CARTESIAN_POINT('',(-0.3954,-4.84225344382863E-17,-0.48));
#33642=CARTESIAN_POINT('Ctrl Pts',(-0.395559352324906,0.000325232430651398,
-0.115584015536923));
#33643=CARTESIAN_POINT('Ctrl Pts',(-0.395778471079392,0.0251397697442085,
-0.116334129183277));
#33644=CARTESIAN_POINT('Ctrl Pts',(-0.393638970125572,0.0499166998589586,
-0.11708424282963));
#33645=CARTESIAN_POINT('Ctrl Pts',(-0.389002685395281,0.0742173137443584,
-0.117834356475983));
#33646=CARTESIAN_POINT('Ctrl Pts',(-0.364725758368326,0.20146235246073,
-0.121762168358516));
#33647=CARTESIAN_POINT('Ctrl Pts',(-0.27199020820128,0.315647408351251,
-0.125689980241049));
#33648=CARTESIAN_POINT('Ctrl Pts',(-0.152429834240862,0.365508475309613,
-0.129617792123582));
#33649=CARTESIAN_POINT('Ctrl Pts',(-0.0328694602804443,0.415369542267976,
-0.133545604006115));
#33650=CARTESIAN_POINT('Ctrl Pts',(0.113515737473344,0.400906620294181,
-0.137473415888647));
#33651=CARTESIAN_POINT('Ctrl Pts',(0.221007441079253,0.328613450240116,
-0.14140122777118));
#33652=CARTESIAN_POINT('Ctrl Pts',(0.328499144685164,0.256320280186051,
-0.145329039653713));
#33653=CARTESIAN_POINT('Ctrl Pts',(0.397097354143193,0.126196862051714,
-0.149256851536246));
#33654=CARTESIAN_POINT('Ctrl Pts',(0.396005127209871,-0.00333908159127506,
-0.153184663418779));
#33655=CARTESIAN_POINT('Ctrl Pts',(0.394912900276549,-0.132875025234262,
-0.157112475301311));
#33656=CARTESIAN_POINT('Ctrl Pts',(0.324130236951877,-0.261823494385903,
-0.161040287183844));
#33657=CARTESIAN_POINT('Ctrl Pts',(0.215434677460811,-0.332293691977232,
-0.164968099066377));
#33658=CARTESIAN_POINT('Ctrl Pts',(0.106739117969747,-0.40276388956856,
-0.16889591094891));
#33659=CARTESIAN_POINT('Ctrl Pts',(-0.0398693376877085,-0.414755815599578,
-0.172823722831442));
#33660=CARTESIAN_POINT('Ctrl Pts',(-0.158571801886283,-0.362885871046767,
-0.176751534713975));
#33661=CARTESIAN_POINT('Ctrl Pts',(-0.27727426608486,-0.311015926493954,
-0.180679346596508));
#33662=CARTESIAN_POINT('Ctrl Pts',(-0.368070738824554,-0.195284111357307,
-0.184607158479041));
#33663=CARTESIAN_POINT('Ctrl Pts',(-0.390198684781093,-0.0676474436879351,
-0.188534970361573));
#33664=CARTESIAN_POINT('Ctrl Pts',(-0.394046557528791,-0.0454524484499415,
-0.189217985420023));
#33665=CARTESIAN_POINT('Ctrl Pts',(-0.395818002029563,-0.0228974691955075,
-0.189901000478473));
#33666=CARTESIAN_POINT('Ctrl Pts',(-0.395622884157063,-0.00031191406896286,
-0.190584015536923));
#33667=CARTESIAN_POINT('Ctrl Pts',(-0.395615927747866,-0.00031357059932876,
-0.201115984463076));
#33668=CARTESIAN_POINT('Ctrl Pts',(-0.395813753948313,-0.0231443884537417,
-0.200425583632879));
#33669=CARTESIAN_POINT('Ctrl Pts',(-0.394003526001132,-0.0459438780543778,
-0.199735182802682));
#33670=CARTESIAN_POINT('Ctrl Pts',(-0.390072407059393,-0.0683716192899147,
-0.199044781972485));
#33671=CARTESIAN_POINT('Ctrl Pts',(-0.367707579243926,-0.195966988052947,
-0.195116970089952));
#33672=CARTESIAN_POINT('Ctrl Pts',(-0.276696457196274,-0.311530079949128,
-0.191189158207419));
#33673=CARTESIAN_POINT('Ctrl Pts',(-0.157897917538397,-0.363179578141115,
-0.187261346324886));
#33674=CARTESIAN_POINT('Ctrl Pts',(-0.0390993778805183,-0.414829076333103,
-0.183333534442354));
#33675=CARTESIAN_POINT('Ctrl Pts',(0.107486579387586,-0.402564980820896,
-0.179405722559821));
#33676=CARTESIAN_POINT('Ctrl Pts',(0.216051120986117,-0.331893167348008,
-0.175477910677288));
#33677=CARTESIAN_POINT('Ctrl Pts',(0.324615662584646,-0.261221353875121,
-0.171550098794755));
#33678=CARTESIAN_POINT('Ctrl Pts',(0.395158788513602,-0.132141822441553,
-0.167622286912222));
#33679=CARTESIAN_POINT('Ctrl Pts',(0.396010585569408,-0.00260404166427942,
-0.16369447502969));
#33680=CARTESIAN_POINT('Ctrl Pts',(0.396862382625215,0.126933739112996,
-0.159766663147157));
#33681=CARTESIAN_POINT('Ctrl Pts',(0.328022850807872,0.256929769233978,
-0.155838851264624));
#33682=CARTESIAN_POINT('Ctrl Pts',(0.220397103955469,0.329023195087183,
-0.151911039382091));
#33683=CARTESIAN_POINT('Ctrl Pts',(0.112771357103067,0.401116620940388,
-0.147983227499559));
#33684=CARTESIAN_POINT('Ctrl Pts',(-0.0336406047843918,0.415307442525814,
-0.144055415617026));
#33685=CARTESIAN_POINT('Ctrl Pts',(-0.15310812608344,0.365224690280065,
-0.140127603734493));
#33686=CARTESIAN_POINT('Ctrl Pts',(-0.272575647382488,0.315141938034316,
-0.13619979185196));
#33687=CARTESIAN_POINT('Ctrl Pts',(-0.365098728093125,0.200785611957391,
-0.132271979969427));
#33688=CARTESIAN_POINT('Ctrl Pts',(-0.389139571160733,0.0734954365042287,
-0.128344168086895));
#33689=CARTESIAN_POINT('Ctrl Pts',(-0.393685563893927,0.0494255563012018,
-0.127601440212289));
#33690=CARTESIAN_POINT('Ctrl Pts',(-0.395782854098394,0.0248932036270088,
-0.126858712337682));
#33691=CARTESIAN_POINT('Ctrl Pts',(-0.395566345080525,0.000324025114679023,
-0.126115984463076));
#33692=CARTESIAN_POINT('Origin',(0.,0.,-0.48));
#33693=CARTESIAN_POINT('',(-0.394794988713166,-8.02750947288822E-5,-0.0405840155369234));
#33694=CARTESIAN_POINT('',(-0.39480767064478,-0.000104727820695843,-0.0511159844630761));
#33695=CARTESIAN_POINT('',(-0.3954,-4.84225344382863E-17,-0.48));
#33696=CARTESIAN_POINT('Ctrl Pts',(-0.394794988713166,-8.02750947288822E-5,
-0.0405840155369234));
#33697=CARTESIAN_POINT('Ctrl Pts',(-0.394615005116812,0.0724759759833135,
-0.0427672578880801));
#33698=CARTESIAN_POINT('Ctrl Pts',(-0.37544474313299,0.145114666223604,
-0.0449505002392368));
#33699=CARTESIAN_POINT('Ctrl Pts',(-0.337893742543562,0.206539063180415,
-0.0471337425903935));
#33700=CARTESIAN_POINT('Ctrl Pts',(-0.270336759582872,0.317046023672708,
-0.0510615544729262));
#33701=CARTESIAN_POINT('Ctrl Pts',(-0.14328752260418,0.391256097572554,
-0.054989366355459));
#33702=CARTESIAN_POINT('Ctrl Pts',(-0.01382092735515,0.395787669078235,
-0.0589171782379918));
#33703=CARTESIAN_POINT('Ctrl Pts',(0.11564566789388,0.400319240583916,-0.0628449901205246));
#33704=CARTESIAN_POINT('Ctrl Pts',(0.24752962141325,0.335172309695432,-0.0667728020030573));
#33705=CARTESIAN_POINT('Ctrl Pts',(0.322641754051717,0.229628399641421,
-0.07070061388559));
#33706=CARTESIAN_POINT('Ctrl Pts',(0.397753886690185,0.124084489587409,
-0.0746284257681228));
#33707=CARTESIAN_POINT('Ctrl Pts',(0.41609419844775,-0.0218563996321296,
-0.0785562376506555));
#33708=CARTESIAN_POINT('Ctrl Pts',(0.369418829098776,-0.142692926762401,
-0.0824840495331883));
#33709=CARTESIAN_POINT('Ctrl Pts',(0.322743459749801,-0.263529453892673,
-0.0864118614157211));
#33710=CARTESIAN_POINT('Ctrl Pts',(0.211052409294286,-0.359261618933676,
-0.090339673298254));
#33711=CARTESIAN_POINT('Ctrl Pts',(0.0844939542274045,-0.38690169880114,
-0.0942674851807868));
#33712=CARTESIAN_POINT('Ctrl Pts',(-0.042064500839475,-0.414541778668603,
-0.0981952970633196));
#33713=CARTESIAN_POINT('Ctrl Pts',(-0.183490360517721,-0.37408977336253,
-0.102123108945852));
#33714=CARTESIAN_POINT('Ctrl Pts',(-0.276294138413411,-0.283711259938383,
-0.106050920828385));
#33715=CARTESIAN_POINT('Ctrl Pts',(-0.351374720210459,-0.210592777871152,
-0.109228619064565));
#33716=CARTESIAN_POINT('Ctrl Pts',(-0.394631101941742,-0.104796320598328,
-0.112406317300744));
#33717=CARTESIAN_POINT('Ctrl Pts',(-0.395559352324906,0.000325232430651398,
-0.115584015536923));
#33718=CARTESIAN_POINT('Ctrl Pts',(-0.395566345080525,0.000324025114679023,
-0.126115984463076));
#33719=CARTESIAN_POINT('Ctrl Pts',(-0.394637876614533,-0.105037440696735,
-0.122930900455149));
#33720=CARTESIAN_POINT('Ctrl Pts',(-0.351158580959819,-0.211076134618309,
-0.119745816447223));
#33721=CARTESIAN_POINT('Ctrl Pts',(-0.275767342730863,-0.284224269941031,
-0.116560732439296));
#33722=CARTESIAN_POINT('Ctrl Pts',(-0.182795665808806,-0.374429776103722,
-0.112632920556764));
#33723=CARTESIAN_POINT('Ctrl Pts',(-0.0412937065401148,-0.414616763599703,
-0.108705108674231));
#33724=CARTESIAN_POINT('Ctrl Pts',(0.085212636995385,-0.386742913751592,
-0.104777296791698));
#33725=CARTESIAN_POINT('Ctrl Pts',(0.211718980530884,-0.358869063903481,
-0.100849484909165));
#33726=CARTESIAN_POINT('Ctrl Pts',(0.32322970833319,-0.262934376711279,
-0.0969216730266324));
#33727=CARTESIAN_POINT('Ctrl Pts',(0.369681792863869,-0.14200931744245,
-0.0929938611440997));
#33728=CARTESIAN_POINT('Ctrl Pts',(0.416133877394547,-0.0210842581736197,
-0.0890660492615669));
#33729=CARTESIAN_POINT('Ctrl Pts',(0.397527318653598,0.124831173171839,
-0.0851382373790342));
#33730=CARTESIAN_POINT('Ctrl Pts',(0.322217300233705,0.230231435304264,
-0.0812104254965014));
#33731=CARTESIAN_POINT('Ctrl Pts',(0.246907281813811,0.335631697436688,
-0.0772826136139687));
#33732=CARTESIAN_POINT('Ctrl Pts',(0.114893803714973,0.40051679035608,-0.0733548017314358));
#33733=CARTESIAN_POINT('Ctrl Pts',(-0.0145601156695766,0.395752615374949,
-0.0694269898489031));
#33734=CARTESIAN_POINT('Ctrl Pts',(-0.144014035054129,0.390988440393817,
-0.0654991779663702));
#33735=CARTESIAN_POINT('Ctrl Pts',(-0.270908395724393,0.316574997512162,
-0.0615713660838375));
#33736=CARTESIAN_POINT('Ctrl Pts',(-0.338267890539552,0.205928032203031,
-0.0576435542013047));
#33737=CARTESIAN_POINT('Ctrl Pts',(-0.375582457622321,0.144633872844177,
-0.0554676976218951));
#33738=CARTESIAN_POINT('Ctrl Pts',(-0.394627361076789,0.0722206111356247,
-0.0532918410424856));
#33739=CARTESIAN_POINT('Ctrl Pts',(-0.39480767064478,-0.000104727820695843,
-0.0511159844630761));
#33740=CARTESIAN_POINT('Origin',(0.,0.,-0.953243520205039));
#33741=CARTESIAN_POINT('',(-0.351835822326257,-7.15400518810813E-5,-0.015743520205039));
#33742=CARTESIAN_POINT('',(-0.352300869236444,-9.88871641177669E-6,-0.00095647979495892));
#33743=CARTESIAN_POINT('',(-0.352375,-1.84016574122319E-14,-0.953243520205039));
#33744=CARTESIAN_POINT('',(-0.0878173632231217,-0.341256870028339,-1.11022302462516E-16));
#33745=CARTESIAN_POINT('Ctrl Pts',(-0.351835822326257,-7.15400518810534E-5,
-0.015743520205039));
#33746=CARTESIAN_POINT('Ctrl Pts',(-0.351963992710222,-0.0517404851579902,
-0.0139989506736631));
#33747=CARTESIAN_POINT('Ctrl Pts',(-0.319843451957026,-0.207024739602225,
-0.00875111060531678));
#33748=CARTESIAN_POINT('Ctrl Pts',(-0.187433410478183,-0.315404643562256,
-0.00350327053697048));
#33749=CARTESIAN_POINT('Ctrl Pts',(-0.0877607245812972,-0.341761560210009,
-9.26992857475106E-17));
#33750=CARTESIAN_POINT('',(-0.351244341336214,-0.0282055544935595,-2.22044604925031E-16));
#33751=CARTESIAN_POINT('Origin',(0.,0.,-1.11022302462516E-16));
#33752=CARTESIAN_POINT('Ctrl Pts',(-0.352300869236444,-9.88871641181485E-6,
-0.000956479794958919));
#33753=CARTESIAN_POINT('Ctrl Pts',(-0.352345797709144,-0.00941591104682515,
-0.000637653196639279));
#33754=CARTESIAN_POINT('Ctrl Pts',(-0.351997710417371,-0.0188238340684492,
-0.00031882659831964));
#33755=CARTESIAN_POINT('Ctrl Pts',(-0.351244341336214,-0.0282055544935645,
0.));
#33756=CARTESIAN_POINT('Origin',(0.,0.,-0.953243520205039));
#33757=CARTESIAN_POINT('',(-0.352517012583431,0.000289842634663734,-0.0907435202050393));
#33758=CARTESIAN_POINT('',(-0.351847124287948,-9.33319823582524E-5,-0.0759564797949592));
#33759=CARTESIAN_POINT('',(-0.352375,-1.84016574122319E-14,-0.953243520205039));
#33760=CARTESIAN_POINT('Ctrl Pts',(-0.352517012583431,0.000289842634663726,
-0.0907435202050393));
#33761=CARTESIAN_POINT('Ctrl Pts',(-0.35168976870693,-0.0933930285049049,
-0.08756582196886));
#33762=CARTESIAN_POINT('Ctrl Pts',(-0.265490968213442,-0.304218052429229,
-0.0804603118501481));
#33763=CARTESIAN_POINT('Ctrl Pts',(0.0885494659099983,-0.405484154345161,
-0.0694269898489031));
#33764=CARTESIAN_POINT('Ctrl Pts',(0.387162014500754,-0.149538618257732,
-0.0576435542013047));
#33765=CARTESIAN_POINT('Ctrl Pts',(0.338128119541936,0.240642875207636,
-0.0458601185537062));
#33766=CARTESIAN_POINT('Ctrl Pts',(-0.01447133509682,0.414817000942304,
-0.0340766829061081));
#33767=CARTESIAN_POINT('Ctrl Pts',(-0.303855303328585,0.245786425248945,
-0.0240378167898856));
#33768=CARTESIAN_POINT('Ctrl Pts',(-0.351675423439652,0.0645895853240114,
-0.0179267625561959));
#33769=CARTESIAN_POINT('Ctrl Pts',(-0.351835822326257,-7.15400518810534E-5,
-0.015743520205039));
#33770=CARTESIAN_POINT('Ctrl Pts',(-0.351847124287948,-9.33319823582628E-5,
-0.0759564797949592));
#33771=CARTESIAN_POINT('Ctrl Pts',(-0.351976508103106,-0.0519914558104146,
-0.0742045244918361));
#33772=CARTESIAN_POINT('Ctrl Pts',(-0.317060654848262,-0.2200783548687,
-0.0685247573061803));
#33773=CARTESIAN_POINT('Ctrl Pts',(-0.0593024712652474,-0.410811133390711,
-0.0589171782379917));
#33774=CARTESIAN_POINT('Ctrl Pts',(0.31016609475332,-0.275771257119863,
-0.0471337425903933));
#33775=CARTESIAN_POINT('Ctrl Pts',(0.400971528752744,0.106676728393338,
-0.0353503069427951));
#33776=CARTESIAN_POINT('Ctrl Pts',(0.13207620156309,0.39373277295688,-0.0235668712951966));
#33777=CARTESIAN_POINT('Ctrl Pts',(-0.245564839941522,0.328304388362198,
-0.012102262245918));
#33778=CARTESIAN_POINT('Ctrl Pts',(-0.351792297499737,0.106462395441665,
-0.00456546507917205));
#33779=CARTESIAN_POINT('Ctrl Pts',(-0.352300869236444,-9.88871641181485E-6,
-0.000956479794958919));
#33780=CARTESIAN_POINT('Origin',(0.,0.,-0.953243520205039));
#33781=CARTESIAN_POINT('',(-0.352573631271738,-0.000277973495335076,-0.165743520205039));
#33782=CARTESIAN_POINT('',(-0.352523244430323,0.000288766691396741,-0.150956479794959));
#33783=CARTESIAN_POINT('',(-0.352375,-1.84016574122319E-14,-0.953243520205039));
#33784=CARTESIAN_POINT('Ctrl Pts',(-0.352573631271738,-0.000277973495335138,
-0.165743520205039));
#33785=CARTESIAN_POINT('Ctrl Pts',(-0.352747517615496,-0.0204059072022519,
-0.165060505146589));
#33786=CARTESIAN_POINT('Ctrl Pts',(-0.342090283220367,-0.15609951803055,
-0.160449678205607));
#33787=CARTESIAN_POINT('Ctrl Pts',(-0.166186424962074,-0.380311672880833,
-0.151911039382091));
#33788=CARTESIAN_POINT('Ctrl Pts',(0.225779846375536,-0.348250558046386,
-0.140127603734493));
#33789=CARTESIAN_POINT('Ctrl Pts',(0.415021432028277,-0.00349929236118479,
-0.128344168086895));
#33790=CARTESIAN_POINT('Ctrl Pts',(0.231620111407843,0.344393268071943,
-0.116560732439296));
#33791=CARTESIAN_POINT('Ctrl Pts',(-0.159749266881169,0.383060734919559,
-0.104777296791698));
#33792=CARTESIAN_POINT('Ctrl Pts',(-0.340821595749303,0.160106819675714,
-0.096171559380279));
#33793=CARTESIAN_POINT('Ctrl Pts',(-0.35271228818058,0.0224042143743351,
-0.0914936338513928));
#33794=CARTESIAN_POINT('Ctrl Pts',(-0.352517012583431,0.000289842634663726,
-0.0907435202050393));
#33795=CARTESIAN_POINT('Ctrl Pts',(-0.352523244430323,0.000288766691396772,
-0.150956479794959));
#33796=CARTESIAN_POINT('Ctrl Pts',(-0.351695806201427,-0.0936079113948325,
-0.147771395787033));
#33797=CARTESIAN_POINT('Ctrl Pts',(-0.26516385741625,-0.304644789833165,
-0.140658499896574));
#33798=CARTESIAN_POINT('Ctrl Pts',(0.0893042060071663,-0.40531479967714,
-0.129617792123582));
#33799=CARTESIAN_POINT('Ctrl Pts',(0.387434651449787,-0.148827808786758,
-0.117834356475983));
#33800=CARTESIAN_POINT('Ctrl Pts',(0.33768892962625,0.241285621564956,-0.106050920828385));
#33801=CARTESIAN_POINT('Ctrl Pts',(-0.0152568165427812,0.414759708192197,
-0.0942674851807867));
#33802=CARTESIAN_POINT('Ctrl Pts',(-0.304075372848491,0.245390612282059,
-0.0842360048363115));
#33803=CARTESIAN_POINT('Ctrl Pts',(-0.351686434899936,0.0643620077109535,
-0.0781323363743689));
#33804=CARTESIAN_POINT('Ctrl Pts',(-0.351847124287948,-9.33319823582628E-5,
-0.0759564797949592));
#33805=CARTESIAN_POINT('Origin',(0.,0.,-0.953243520205039));
#33806=CARTESIAN_POINT('',(-0.351837382782584,7.0202050624176E-5,-0.240743520205039));
#33807=CARTESIAN_POINT('',(-0.352567431816273,-0.00027944977225125,-0.225956479794959));
#33808=CARTESIAN_POINT('',(-0.352375,-1.84016574122319E-14,-0.953243520205039));
#33809=CARTESIAN_POINT('Ctrl Pts',(-0.351837382782584,7.02020506242011E-5,
-0.240743520205039));
#33810=CARTESIAN_POINT('Ctrl Pts',(-0.351723411718861,-0.0626236980051817,
-0.238627376441786));
#33811=CARTESIAN_POINT('Ctrl Pts',(-0.306014692059434,-0.241840017228692,
-0.232583420796));
#33812=CARTESIAN_POINT('Ctrl Pts',(-0.0214828697613762,-0.414479711673496,
-0.222611653267681));
#33813=CARTESIAN_POINT('Ctrl Pts',(0.334031816159831,-0.24632842310955,
-0.210828217620083));
#33814=CARTESIAN_POINT('Ctrl Pts',(0.389623538603825,0.142998066471633,
-0.199044781972485));
#33815=CARTESIAN_POINT('Ctrl Pts',(0.095377177077531,0.403928376352516,
-0.187261346324887));
#33816=CARTESIAN_POINT('Ctrl Pts',(-0.262487523267468,0.308074448246341,
-0.176160925735738));
#33817=CARTESIAN_POINT('Ctrl Pts',(-0.351747550134876,0.0953437182368893,
-0.168988317029122));
#33818=CARTESIAN_POINT('Ctrl Pts',(-0.352573631271738,-0.000277973495335138,
-0.165743520205039));
#33819=CARTESIAN_POINT('Ctrl Pts',(-0.352567431816273,-0.000279449772251281,
-0.225956479794959));
#33820=CARTESIAN_POINT('Ctrl Pts',(-0.352743731784361,-0.0206259582230498,
-0.225266078964762));
#33821=CARTESIAN_POINT('Ctrl Pts',(-0.341952418100667,-0.156540578529107,
-0.220647866252033));
#33822=CARTESIAN_POINT('Ctrl Pts',(-0.16548019720029,-0.380619515500736,
-0.21210184165677));
#33823=CARTESIAN_POINT('Ctrl Pts',(0.226425923378982,-0.347830739657686,
-0.200318406009172));
#33824=CARTESIAN_POINT('Ctrl Pts',(0.415027091810056,-0.00272907130485191,
-0.188534970361573));
#33825=CARTESIAN_POINT('Ctrl Pts',(0.230980581763497,0.344822909832333,
-0.176751534713975));
#33826=CARTESIAN_POINT('Ctrl Pts',(-0.160460352000493,0.382762900395039,
-0.164968099066377));
#33827=CARTESIAN_POINT('Ctrl Pts',(-0.340962773002534,0.159666203276401,
-0.156369747426705));
#33828=CARTESIAN_POINT('Ctrl Pts',(-0.352716194266368,0.0221844780679374,
-0.151699207669566));
#33829=CARTESIAN_POINT('Ctrl Pts',(-0.352523244430323,0.000288766691396772,
-0.150956479794959));
#33830=CARTESIAN_POINT('Origin',(0.,0.,-0.953243520205039));
#33831=CARTESIAN_POINT('',(-0.352799145083587,0.000183312123080604,-0.315743520205039));
#33832=CARTESIAN_POINT('',(-0.351838709616628,7.35440374098617E-5,-0.300956479794959));
#33833=CARTESIAN_POINT('',(-0.352375,-1.84016574122319E-14,-0.953243520205039));
#33834=CARTESIAN_POINT('Ctrl Pts',(-0.352799145083587,0.000183312123080604,
-0.315743520205039));
#33835=CARTESIAN_POINT('Ctrl Pts',(-0.352131648439078,-0.104236205614763,
-0.312194247736983));
#33836=CARTESIAN_POINT('Ctrl Pts',(-0.248155783239845,-0.325368532847375,
-0.304717163386393));
#33837=CARTESIAN_POINT('Ctrl Pts',(0.125977747866173,-0.395454868510028,
-0.293312267153272));
#33838=CARTESIAN_POINT('Ctrl Pts',(0.399415292924746,-0.112793482827731,
-0.281528831505673));
#33839=CARTESIAN_POINT('Ctrl Pts',(0.314222868844781,0.271143752956601,
-0.269745395858075));
#33840=CARTESIAN_POINT('Ctrl Pts',(-0.0531063182568973,0.411624422068856,
-0.257961960210477));
#33841=CARTESIAN_POINT('Ctrl Pts',(-0.315348018446608,0.223658028597815,
-0.248294668326131));
#33842=CARTESIAN_POINT('Ctrl Pts',(-0.351934955426869,0.0537435592094025,
-0.242555188324319));
#33843=CARTESIAN_POINT('Ctrl Pts',(-0.351837382782584,7.02020506242011E-5,
-0.240743520205039));
#33844=CARTESIAN_POINT('Ctrl Pts',(-0.351838709616628,7.35440374098409E-5,
-0.300956479794959));
#33845=CARTESIAN_POINT('Ctrl Pts',(-0.351718869054174,-0.0628385582901232,
-0.298832950259959));
#33846=CARTESIAN_POINT('Ctrl Pts',(-0.305776206148664,-0.242280141890258,
-0.292781608842426));
#33847=CARTESIAN_POINT('Ctrl Pts',(-0.0207134553279411,-0.414518842516768,
-0.28280245554236));
#33848=CARTESIAN_POINT('Ctrl Pts',(0.334488460689772,-0.245707931903623,
-0.271019019894762));
#33849=CARTESIAN_POINT('Ctrl Pts',(0.389357394519836,0.14372104213278,-0.259235584247163));
#33850=CARTESIAN_POINT('Ctrl Pts',(0.0946272181670758,0.404104697832314,
-0.247452148599565));
#33851=CARTESIAN_POINT('Ctrl Pts',(-0.262820927742507,0.307650859050363,
-0.236359113782163));
#33852=CARTESIAN_POINT('Ctrl Pts',(-0.351740730224602,0.0951289107829825,
-0.229193890847295));
#33853=CARTESIAN_POINT('Ctrl Pts',(-0.352567431816273,-0.000279449772251281,
-0.225956479794959));
#33854=CARTESIAN_POINT('Origin',(0.,0.,-0.953243520205039));
#33855=CARTESIAN_POINT('',(-0.352256412867894,-0.000300619911437438,-0.390743520205039));
#33856=CARTESIAN_POINT('',(-0.352803593413643,0.000180282396865468,-0.375956479794959));
#33857=CARTESIAN_POINT('',(-0.352375,-1.84016574122319E-14,-0.953243520205039));
#33858=CARTESIAN_POINT('Ctrl Pts',(-0.352256412867894,-0.000300619911437438,
-0.390743520205039));
#33859=CARTESIAN_POINT('Ctrl Pts',(-0.352520787606664,-0.0314505761894478,
-0.389688930914712));
#33860=CARTESIAN_POINT('Ctrl Pts',(-0.334574478215314,-0.178318959414863,
-0.384706529741852));
#33861=CARTESIAN_POINT('Ctrl Pts',(-0.129997826644863,-0.394151634612728,
-0.37579631668646));
#33862=CARTESIAN_POINT('Ctrl Pts',(0.257270836187783,-0.325678772484742,
-0.364012881038862));
#33863=CARTESIAN_POINT('Ctrl Pts',(0.41353925015983,0.0352169643329669,
-0.352229445391263));
#33864=CARTESIAN_POINT('Ctrl Pts',(0.198495971305819,0.364491831701348,
-0.340446009743665));
#33865=CARTESIAN_POINT('Ctrl Pts',(-0.194774344275583,0.366494066541952,
-0.328662574096066));
#33866=CARTESIAN_POINT('Ctrl Pts',(-0.347379815174857,0.137941644433663,
-0.320428410916525));
#33867=CARTESIAN_POINT('Ctrl Pts',(-0.352870335388431,0.0113199333490138,
-0.316122059619516));
#33868=CARTESIAN_POINT('Ctrl Pts',(-0.352799145083587,0.000183312123080604,
-0.315743520205039));
#33869=CARTESIAN_POINT('Ctrl Pts',(-0.352803593413643,0.000180282396865497,
-0.375956479794959));
#33870=CARTESIAN_POINT('Ctrl Pts',(-0.352143610457793,-0.10445300778349,
-0.372399821555156));
#33871=CARTESIAN_POINT('Ctrl Pts',(-0.247793743118397,-0.325783646241757,
-0.36491535143282));
#33872=CARTESIAN_POINT('Ctrl Pts',(0.126711582028227,-0.395220309612058,
-0.353503069427949));
#33873=CARTESIAN_POINT('Ctrl Pts',(0.399623944950114,-0.112051866435688,
-0.341719633780353));
#33874=CARTESIAN_POINT('Ctrl Pts',(0.313718992635124,0.271726538679157,
-0.329936198132753));
#33875=CARTESIAN_POINT('Ctrl Pts',(-0.0538702984580581,0.411525101398655,
-0.318152762485156));
#33876=CARTESIAN_POINT('Ctrl Pts',(-0.315562529348155,0.223216238813576,
-0.308492856372557));
#33877=CARTESIAN_POINT('Ctrl Pts',(-0.351940533588365,0.0535275665997614,
-0.302760762142492));
#33878=CARTESIAN_POINT('Ctrl Pts',(-0.351838709616628,7.35440374098409E-5,
-0.300956479794959));
#33879=CARTESIAN_POINT('Origin',(0.,0.,-0.953243520205039));
#33880=CARTESIAN_POINT('',(-0.351979915865352,0.000219139502586136,-0.46574352020504));
#33881=CARTESIAN_POINT('',(-0.352250282015284,-0.000300002405069166,-0.45095647979496));
#33882=CARTESIAN_POINT('',(-0.352375,-1.84016574122319E-14,-0.953243520205039));
#33883=CARTESIAN_POINT('Ctrl Pts',(-0.351979915865352,0.000219139502586143,
-0.46574352020504));
#33884=CARTESIAN_POINT('Ctrl Pts',(-0.351551012165278,-0.0734082552370908,
-0.463255802209909));
#33885=CARTESIAN_POINT('Ctrl Pts',(-0.293285509062973,-0.263906146917594,
-0.456840272332246));
#33886=CARTESIAN_POINT('Ctrl Pts',(0.0172614319911864,-0.414676969416019,
-0.44649693057205));
#33887=CARTESIAN_POINT('Ctrl Pts',(0.355546713117099,-0.214106237165738,
-0.434713494924451));
#33888=CARTESIAN_POINT('Ctrl Pts',(0.37459107121508,0.178707793242271,-0.422930059276854));
#33889=CARTESIAN_POINT('Ctrl Pts',(0.0572948166238478,0.411062343188925,
-0.411146623629255));
#33890=CARTESIAN_POINT('Ctrl Pts',(-0.278444336628561,0.28656647445625,
-0.400417777271984));
#33891=CARTESIAN_POINT('Ctrl Pts',(-0.351536125378526,0.0845672608314457,
-0.393616742797245));
#33892=CARTESIAN_POINT('Ctrl Pts',(-0.352256412867894,-0.000300619911437438,
-0.390743520205039));
#33893=CARTESIAN_POINT('Ctrl Pts',(-0.352250282015284,-0.000300002405069236,
-0.450956479794959));
#33894=CARTESIAN_POINT('Ctrl Pts',(-0.35251557432598,-0.0316694991392887,
-0.449894504732885));
#33895=CARTESIAN_POINT('Ctrl Pts',(-0.334412778538798,-0.178761099283432,
-0.444904717788278));
#33896=CARTESIAN_POINT('Ctrl Pts',(-0.129265949902175,-0.394392231601152,
-0.435987118961139));
#33897=CARTESIAN_POINT('Ctrl Pts',(0.257874911974541,-0.325200627191768,
-0.42420368331354));
#33898=CARTESIAN_POINT('Ctrl Pts',(0.413473132937555,0.0359845312630004,
-0.412420247665942));
#33899=CARTESIAN_POINT('Ctrl Pts',(0.197819026895949,0.364859631570464,
-0.400636812018343));
#33900=CARTESIAN_POINT('Ctrl Pts',(-0.195454295996888,0.366131856477703,
-0.388853376370746));
#33901=CARTESIAN_POINT('Ctrl Pts',(-0.347498740933083,0.137501831020397,
-0.38062659896295));
#33902=CARTESIAN_POINT('Ctrl Pts',(-0.352872465670038,0.0110992473866874,
-0.376327633437688));
#33903=CARTESIAN_POINT('Ctrl Pts',(-0.352803593413643,0.000180282396865497,
-0.375956479794959));
#33904=CARTESIAN_POINT('Origin',(0.,0.,-0.953243520205039));
#33905=CARTESIAN_POINT('',(-0.352926766978824,3.65888010280694E-6,-0.54074352020504));
#33906=CARTESIAN_POINT('',(-0.351984139032922,0.000221539830159989,-0.52595647979496));
#33907=CARTESIAN_POINT('',(-0.352375,-1.84016574122319E-14,-0.953243520205039));
#33908=CARTESIAN_POINT('Ctrl Pts',(-0.352926747396533,3.65875024863191E-6,
-0.54074352020504));
#33909=CARTESIAN_POINT('Ctrl Pts',(-0.352908681542431,-0.115236454325059,
-0.536822673505106));
#33910=CARTESIAN_POINT('Ctrl Pts',(-0.229082675555813,-0.345954773140889,
-0.528974014922639));
#33911=CARTESIAN_POINT('Ctrl Pts',(0.162305420542359,-0.381984157190963,
-0.517197544457641));
#33912=CARTESIAN_POINT('Ctrl Pts',(0.408193007052407,-0.0750560794736075,
-0.505414108810041));
#33913=CARTESIAN_POINT('Ctrl Pts',(0.287569224913323,0.299263908404139,
-0.493630673162444));
#33914=CARTESIAN_POINT('Ctrl Pts',(-0.09125934819834,0.40487859581871,-0.481847237514845));
#33915=CARTESIAN_POINT('Ctrl Pts',(-0.32546833938393,0.201410083407456,
-0.472551519862377));
#33916=CARTESIAN_POINT('Ctrl Pts',(-0.352228200276193,0.0428406751097234,
-0.467183614092442));
#33917=CARTESIAN_POINT('Ctrl Pts',(-0.351979915865352,0.000219139502586143,
-0.46574352020504));
#33918=CARTESIAN_POINT('Ctrl Pts',(-0.351984139032922,0.000221539830159961,
-0.52595647979496));
#33919=CARTESIAN_POINT('Ctrl Pts',(-0.351548904827268,-0.0736221937851192,
-0.523461376028082));
#33920=CARTESIAN_POINT('Ctrl Pts',(-0.293017054148803,-0.264342833231124,
-0.517038460378671));
#33921=CARTESIAN_POINT('Ctrl Pts',(0.0180311431761832,-0.414644180006055,
-0.506687732846728));
#33922=CARTESIAN_POINT('Ctrl Pts',(0.355943505618862,-0.213445868946458,
-0.49490429719913));
#33923=CARTESIAN_POINT('Ctrl Pts',(0.374258670005346,0.17940280397765,-0.483120861551532));
#33924=CARTESIAN_POINT('Ctrl Pts',(0.0565316805849977,0.411167955025903,
-0.471337425903933));
#33925=CARTESIAN_POINT('Ctrl Pts',(-0.278744807800919,0.286135228707803,
-0.460615965318409));
#33926=CARTESIAN_POINT('Ctrl Pts',(-0.35153436645443,0.0843534532086563,
-0.453822316615418));
#33927=CARTESIAN_POINT('Ctrl Pts',(-0.352250282015284,-0.000300002405069236,
-0.450956479794959));
#33928=CARTESIAN_POINT('Origin',(0.,0.,-0.953243520205039));
#33929=CARTESIAN_POINT('',(-0.351987971037649,-0.000223646241047472,-0.61574352020504));
#33930=CARTESIAN_POINT('',(-0.35292677092685,-2.20166561067338E-7,-0.60095647979496));
#33931=CARTESIAN_POINT('',(-0.352375,-1.84016574122319E-14,-0.953243520205039));
#33932=CARTESIAN_POINT('Ctrl Pts',(-0.351987971037649,-0.000223646241047443,
-0.61574352020504));
#33933=CARTESIAN_POINT('Ctrl Pts',(-0.352239290406269,-0.0424304558714861,
-0.614317356682835));
#33934=CARTESIAN_POINT('Ctrl Pts',(-0.325821604001666,-0.200575489607239,
-0.608963381278098));
#33935=CARTESIAN_POINT('Ctrl Pts',(-0.0926762852132086,-0.404556616836208,
-0.599681593990828));
#33936=CARTESIAN_POINT('Ctrl Pts',(0.286519709527895,-0.300268871483724,
-0.58789815834323));
#33937=CARTESIAN_POINT('Ctrl Pts',(0.408453286141698,0.0736265026253448,
-0.576114722695632));
#33938=CARTESIAN_POINT('Ctrl Pts',(0.163641779290076,0.381413573840065,
-0.564331287048033));
#33939=CARTESIAN_POINT('Ctrl Pts',(-0.228101616324409,0.34673418884258,
-0.552547851400434));
#33940=CARTESIAN_POINT('Ctrl Pts',(-0.352834663655244,0.115857896512362,
-0.544685262452771));
#33941=CARTESIAN_POINT('Ctrl Pts',(-0.352926779489594,0.000208376886847085,
-0.540750485387639));
#33942=CARTESIAN_POINT('Ctrl Pts',(-0.352926747396533,3.65875024863191E-6,
-0.54074352020504));
#33943=CARTESIAN_POINT('Ctrl Pts',(-0.352926770854712,-2.20166532327402E-7,
-0.60095647979496));
#33944=CARTESIAN_POINT('Ctrl Pts',(-0.352926770972352,-1.2581965258919E-5,
-0.600956059205812));
#33945=CARTESIAN_POINT('Ctrl Pts',(-0.352921218665278,-0.115469719509711,
-0.597027826734131));
#33946=CARTESIAN_POINT('Ctrl Pts',(-0.22867160906457,-0.346358504439924,
-0.589171782379916));
#33947=CARTESIAN_POINT('Ctrl Pts',(0.163014183448326,-0.38168218876817,
-0.577388346732319));
#33948=CARTESIAN_POINT('Ctrl Pts',(0.408331593749854,-0.0742982379650506,
-0.56560491108472));
#33949=CARTESIAN_POINT('Ctrl Pts',(0.28701319867986,0.299797167962814,-0.553821475437122));
#33950=CARTESIAN_POINT('Ctrl Pts',(-0.0920107376299498,0.404708465680984,
-0.542038039789523));
#33951=CARTESIAN_POINT('Ctrl Pts',(-0.325655832183524,0.200967578910638,
-0.532749707908803));
#33952=CARTESIAN_POINT('Ctrl Pts',(-0.352234053921003,0.0426231897516333,
-0.527389187910615));
#33953=CARTESIAN_POINT('Ctrl Pts',(-0.351984139032922,0.000221539830159961,
-0.52595647979496));
#33954=CARTESIAN_POINT('Origin',(0.,0.,-0.953243520205039));
#33955=CARTESIAN_POINT('',(-0.352244141620507,0.000298967984602608,-0.69074352020504));
#33956=CARTESIAN_POINT('',(-0.351983621638971,-0.000221293924554444,-0.67595647979496));
#33957=CARTESIAN_POINT('',(-0.352375,-1.84016574122319E-14,-0.953243520205039));
#33958=CARTESIAN_POINT('Ctrl Pts',(-0.352244141620507,0.000298967984602598,
-0.69074352020504));
#33959=CARTESIAN_POINT('Ctrl Pts',(-0.351532316544511,-0.0841643753389943,
-0.687884227978032));
#33960=CARTESIAN_POINT('Ctrl Pts',(-0.279011704689758,-0.285752370658725,
-0.681097123868492));
#33961=CARTESIAN_POINT('Ctrl Pts',(0.055855997335481,-0.411260820487245,
-0.670382207876418));
#33962=CARTESIAN_POINT('Ctrl Pts',(0.373962743705146,-0.180017958610726,
-0.65859877222882));
#33963=CARTESIAN_POINT('Ctrl Pts',(0.356294325733907,0.212860018649936,
-0.646815336581221));
#33964=CARTESIAN_POINT('Ctrl Pts',(0.0187130423499051,0.414614052167785,
-0.635031900933623));
#33965=CARTESIAN_POINT('Ctrl Pts',(-0.292778674157529,0.264729732699978,
-0.624674628808229));
#33966=CARTESIAN_POINT('Ctrl Pts',(-0.351547129102879,0.0738117602623278,
-0.618245168565368));
#33967=CARTESIAN_POINT('Ctrl Pts',(-0.351987971037649,-0.000223646241047443,
-0.61574352020504));
#33968=CARTESIAN_POINT('Ctrl Pts',(-0.351983621638971,-0.000221293924554434,
-0.67595647979496));
#33969=CARTESIAN_POINT('Ctrl Pts',(-0.352233383192499,-0.0426479614893011,
-0.674522930501008));
#33970=CARTESIAN_POINT('Ctrl Pts',(-0.325634615254823,-0.201017878084083,
-0.669161569324524));
#33971=CARTESIAN_POINT('Ctrl Pts',(-0.0919250879749927,-0.404727983568883,
-0.659872396265506));
#33972=CARTESIAN_POINT('Ctrl Pts',(0.287076527003714,-0.299736444131386,
-0.64808896061791));
#33973=CARTESIAN_POINT('Ctrl Pts',(0.408315900728571,0.074384541261718,
-0.636305524970309));
#33974=CARTESIAN_POINT('Ctrl Pts',(0.162933476272259,0.381716654782934,
-0.624522089322712));
#33975=CARTESIAN_POINT('Ctrl Pts',(-0.228730842945548,0.346311409591309,
-0.612739074264261));
#33976=CARTESIAN_POINT('Ctrl Pts',(-0.352925672358273,0.115432193888956,
-0.604883871088345));
#33977=CARTESIAN_POINT('Ctrl Pts',(-0.352926770854712,-2.20166532327402E-7,
-0.60095647979496));
#33978=CARTESIAN_POINT('Origin',(0.,0.,-0.953243520205039));
#33979=CARTESIAN_POINT('',(-0.352786263833399,-0.000190149253296143,-0.76574352020504));
#33980=CARTESIAN_POINT('',(-0.352246168648578,0.000295985828685064,-0.75095647979496));
#33981=CARTESIAN_POINT('',(-0.352375,-1.84016574122319E-14,-0.953243520205039));
#33982=CARTESIAN_POINT('Ctrl Pts',(-0.352786263833399,-0.000190149253296124,
-0.76574352020504));
#33983=CARTESIAN_POINT('Ctrl Pts',(-0.352849014341479,-0.0109186220279966,
-0.765378911155762));
#33984=CARTESIAN_POINT('Ctrl Pts',(-0.347537096564293,-0.137150916764344,
-0.761086490223951));
#33985=CARTESIAN_POINT('Ctrl Pts',(-0.196120693160165,-0.365772397335523,
-0.752866257409607));
#33986=CARTESIAN_POINT('Ctrl Pts',(0.197252328460035,-0.365204165813244,
-0.741082821762008));
#33987=CARTESIAN_POINT('Ctrl Pts',(0.413395790837222,-0.036654313951176,
-0.72929938611441));
#33988=CARTESIAN_POINT('Ctrl Pts',(0.258418710730661,0.324770678736576,
-0.717515950466812));
#33989=CARTESIAN_POINT('Ctrl Pts',(-0.128621903482862,0.394607163242637,
-0.705732514819214));
#33990=CARTESIAN_POINT('Ctrl Pts',(-0.334268395112202,0.179152490472527,
-0.696808371398623));
#33991=CARTESIAN_POINT('Ctrl Pts',(-0.352510151186726,0.0318629829041549,
-0.691812039860565));
#33992=CARTESIAN_POINT('Ctrl Pts',(-0.352244141620507,0.000298967984602598,
-0.69074352020504));
#33993=CARTESIAN_POINT('Ctrl Pts',(-0.352246168648579,0.000295985828685053,
-0.75095647979496));
#33994=CARTESIAN_POINT('Ctrl Pts',(-0.351530728592248,-0.0843810609727061,
-0.748089801796205));
#33995=CARTESIAN_POINT('Ctrl Pts',(-0.278717649207867,-0.286178366077153,
-0.741295311914916));
#33996=CARTESIAN_POINT('Ctrl Pts',(0.056622872027267,-0.411159623934646,
-0.730573010151098));
#33997=CARTESIAN_POINT('Ctrl Pts',(0.374294355448138,-0.179321777388505,
-0.718789574503498));
#33998=CARTESIAN_POINT('Ctrl Pts',(0.355899542327467,0.213520119856154,
-0.7070061388559));
#33999=CARTESIAN_POINT('Ctrl Pts',(0.017942870124783,0.414648503505772,
-0.695222703208303));
#34000=CARTESIAN_POINT('Ctrl Pts',(-0.29304745006662,0.26429292408189,-0.684872816854654));
#34001=CARTESIAN_POINT('Ctrl Pts',(-0.351549056255237,0.0735977579290679,
-0.678450742383541));
#34002=CARTESIAN_POINT('Ctrl Pts',(-0.351983621638971,-0.000221293924554434,
-0.67595647979496));
#34003=CARTESIAN_POINT('Ctrl Pts',(-0.350836093496678,-0.0328964454765271,
-0.824840495331884));
#34004=CARTESIAN_POINT('Ctrl Pts',(-0.340011333932142,-0.148341026301304,
-0.820912683449351));
#34005=CARTESIAN_POINT('Ctrl Pts',(-0.195816346135933,-0.365812208923844,
-0.813057059684284));
#34006=CARTESIAN_POINT('Ctrl Pts',(0.198108374437807,-0.364996837653778,
-0.801273624036688));
#34007=CARTESIAN_POINT('Ctrl Pts',(0.413371658758658,-0.0358045106953606,
-0.789490188389087));
#34008=CARTESIAN_POINT('Ctrl Pts',(0.257863027527083,0.32520678286678,-0.777706752741491));
#34009=CARTESIAN_POINT('Ctrl Pts',(-0.129379073725142,0.394390194728457,
-0.765923317093891));
#34010=CARTESIAN_POINT('Ctrl Pts',(-0.400348103178378,0.109366128011736,
-0.754139881446294));
#34011=CARTESIAN_POINT('Ctrl Pts',(-0.311904664228006,-0.273809580860039,
-0.742356445798694));
#34012=CARTESIAN_POINT('Ctrl Pts',(0.056622872027267,-0.411159623934646,
-0.730573010151098));
#34013=CARTESIAN_POINT('Ctrl Pts',(0.374294355448138,-0.179321777388505,
-0.718789574503498));
#34014=CARTESIAN_POINT('Ctrl Pts',(0.355899542327467,0.213520119856154,
-0.7070061388559));
#34015=CARTESIAN_POINT('Ctrl Pts',(0.017942870124783,0.414648503505772,
-0.695222703208303));
#34016=CARTESIAN_POINT('Ctrl Pts',(-0.336122314727238,0.243467368383994,
-0.683439267560703));
#34017=CARTESIAN_POINT('Ctrl Pts',(-0.38838863294677,-0.146319091464592,
-0.671655831913106));
#34018=CARTESIAN_POINT('Ctrl Pts',(-0.0919250879749927,-0.404727983568883,
-0.659872396265506));
#34019=CARTESIAN_POINT('Ctrl Pts',(0.287076527003714,-0.299736444131386,
-0.64808896061791));
#34020=CARTESIAN_POINT('Ctrl Pts',(0.408315900728571,0.074384541261718,
-0.636305524970309));
#34021=CARTESIAN_POINT('Ctrl Pts',(0.162933476272259,0.381716654782934,
-0.624522089322712));
#34022=CARTESIAN_POINT('Ctrl Pts',(-0.22874482321813,0.346310145817832,
-0.612738653675113));
#34023=CARTESIAN_POINT('Ctrl Pts',(-0.4150360455362,-4.38686883980485E-5,
-0.600955218027516));
#34024=CARTESIAN_POINT('Ctrl Pts',(-0.22867160906457,-0.346358504439924,
-0.589171782379916));
#34025=CARTESIAN_POINT('Ctrl Pts',(0.163014183448326,-0.38168218876817,
-0.577388346732319));
#34026=CARTESIAN_POINT('Ctrl Pts',(0.408331593749854,-0.0742982379650506,
-0.56560491108472));
#34027=CARTESIAN_POINT('Ctrl Pts',(0.28701319867986,0.299797167962814,-0.553821475437122));
#34028=CARTESIAN_POINT('Ctrl Pts',(-0.0920107376299498,0.404708465680984,
-0.542038039789523));
#34029=CARTESIAN_POINT('Ctrl Pts',(-0.38841939005586,0.14623712132408,-0.530254604141926));
#34030=CARTESIAN_POINT('Ctrl Pts',(-0.336071155929779,-0.243538695681005,
-0.518471168494327));
#34031=CARTESIAN_POINT('Ctrl Pts',(0.0180311431761832,-0.414644180006055,
-0.506687732846728));
#34032=CARTESIAN_POINT('Ctrl Pts',(0.355943505618862,-0.213445868946458,
-0.49490429719913));
#34033=CARTESIAN_POINT('Ctrl Pts',(0.374258670005346,0.17940280397765,-0.483120861551532));
#34034=CARTESIAN_POINT('Ctrl Pts',(0.0565316805849977,0.411167955025903,
-0.471337425903933));
#34035=CARTESIAN_POINT('Ctrl Pts',(-0.311954394006589,0.273750569338514,
-0.459553990256335));
#34036=CARTESIAN_POINT('Ctrl Pts',(-0.400340540765316,-0.109464010390782,
-0.447770554608737));
#34037=CARTESIAN_POINT('Ctrl Pts',(-0.129265949902175,-0.394392231601152,
-0.435987118961139));
#34038=CARTESIAN_POINT('Ctrl Pts',(0.257874911974541,-0.325200627191768,
-0.42420368331354));
#34039=CARTESIAN_POINT('Ctrl Pts',(0.413473132937555,0.0359845312630004,
-0.412420247665942));
#34040=CARTESIAN_POINT('Ctrl Pts',(0.197819026895949,0.364859631570464,
-0.400636812018343));
#34041=CARTESIAN_POINT('Ctrl Pts',(-0.195454295996888,0.366131856477703,
-0.388853376370746));
#34042=CARTESIAN_POINT('Ctrl Pts',(-0.413231664177891,0.0386588912395302,
-0.377069940723146));
#34043=CARTESIAN_POINT('Ctrl Pts',(-0.259973517118929,-0.323525406343912,
-0.365286505075549));
#34044=CARTESIAN_POINT('Ctrl Pts',(0.126711582028227,-0.395220309612058,
-0.353503069427949));
#34045=CARTESIAN_POINT('Ctrl Pts',(0.399623944950114,-0.112051866435688,
-0.341719633780353));
#34046=CARTESIAN_POINT('Ctrl Pts',(0.313718992635124,0.271726538679157,
-0.329936198132753));
#34047=CARTESIAN_POINT('Ctrl Pts',(-0.0538702984580581,0.411525101398655,
-0.318152762485156));
#34048=CARTESIAN_POINT('Ctrl Pts',(-0.373090125879399,0.181820450206457,
-0.306369326837557));
#34049=CARTESIAN_POINT('Ctrl Pts',(-0.357317020662606,-0.211138497127641,
-0.294585891189959));
#34050=CARTESIAN_POINT('Ctrl Pts',(-0.0207134553279411,-0.414518842516768,
-0.28280245554236));
#34051=CARTESIAN_POINT('Ctrl Pts',(0.334488460689772,-0.245707931903623,
-0.271019019894762));
#34052=CARTESIAN_POINT('Ctrl Pts',(0.389357394519836,0.14372104213278,-0.259235584247163));
#34053=CARTESIAN_POINT('Ctrl Pts',(0.0946272181670758,0.404104697832314,
-0.247452148599565));
#34054=CARTESIAN_POINT('Ctrl Pts',(-0.285067544718883,0.301647829990517,
-0.235668712951967));
#34055=CARTESIAN_POINT('Ctrl Pts',(-0.408803749032928,-0.0716548379065293,
-0.223885277304369));
#34056=CARTESIAN_POINT('Ctrl Pts',(-0.16548019720029,-0.380619515500736,
-0.21210184165677));
#34057=CARTESIAN_POINT('Ctrl Pts',(0.226425923378982,-0.347830739657686,
-0.200318406009172));
#34058=CARTESIAN_POINT('Ctrl Pts',(0.415027091810056,-0.00272907130485191,
-0.188534970361573));
#34059=CARTESIAN_POINT('Ctrl Pts',(0.230980581763497,0.344822909832333,
-0.176751534713975));
#34060=CARTESIAN_POINT('Ctrl Pts',(-0.160460352000493,0.382762900395039,
-0.164968099066377));
#34061=CARTESIAN_POINT('Ctrl Pts',(-0.40782621365004,0.0770245817201009,
-0.153184663418778));
#34062=CARTESIAN_POINT('Ctrl Pts',(-0.289009548904106,-0.29787254080843,
-0.14140122777118));
#34063=CARTESIAN_POINT('Ctrl Pts',(0.0893042060071663,-0.40531479967714,
-0.129617792123582));
#34064=CARTESIAN_POINT('Ctrl Pts',(0.387434651449787,-0.148827808786758,
-0.117834356475983));
#34065=CARTESIAN_POINT('Ctrl Pts',(0.33768892962625,0.241285621564956,-0.106050920828385));
#34066=CARTESIAN_POINT('Ctrl Pts',(-0.0152568165427812,0.414759708192197,
-0.0942674851807867));
#34067=CARTESIAN_POINT('Ctrl Pts',(-0.354516303198198,0.215811021276995,
-0.0824840495331884));
#34068=CARTESIAN_POINT('Ctrl Pts',(-0.375435905852211,-0.176882543716822,
-0.07070061388559));
#34069=CARTESIAN_POINT('Ctrl Pts',(-0.0593024712652474,-0.410811133390711,
-0.0589171782379917));
#34070=CARTESIAN_POINT('Ctrl Pts',(0.31016609475332,-0.275771257119863,
-0.0471337425903933));
#34071=CARTESIAN_POINT('Ctrl Pts',(0.400971528752744,0.106676728393338,
-0.0353503069427951));
#34072=CARTESIAN_POINT('Ctrl Pts',(0.13207620156309,0.39373277295688,-0.0235668712951966));
#34073=CARTESIAN_POINT('Ctrl Pts',(-0.256066899639439,0.326484848838067,
-0.0117834356475983));
#34074=CARTESIAN_POINT('Ctrl Pts',(-0.360525536959465,0.0873733625685078,
-0.00392781188253277));
#34075=CARTESIAN_POINT('Ctrl Pts',(-0.351244341336214,-0.0282055544935645,
0.));
#34076=CARTESIAN_POINT('Ctrl Pts',(-0.365115126650463,-0.0342353311964058,
-0.816560330221256));
#34077=CARTESIAN_POINT('Ctrl Pts',(-0.353849799243652,-0.154378507825829,
-0.812632518338723));
#34078=CARTESIAN_POINT('Ctrl Pts',(-0.203786073739102,-0.3807007701526,
-0.804776894573657));
#34079=CARTESIAN_POINT('Ctrl Pts',(0.206171387619962,-0.3798522132622,-0.792993458926059));
#34080=CARTESIAN_POINT('Ctrl Pts',(0.430195890158058,-0.0372617547040343,
-0.781210023278461));
#34081=CARTESIAN_POINT('Ctrl Pts',(0.268358055796544,0.338442702774873,
-0.769426587630862));
#34082=CARTESIAN_POINT('Ctrl Pts',(-0.134644803555601,0.410441880317382,
-0.757643151983264));
#34083=CARTESIAN_POINT('Ctrl Pts',(-0.416642275711663,0.113817330715017,
-0.745859716335666));
#34084=CARTESIAN_POINT('Ctrl Pts',(-0.324599187750211,-0.28495363403871,
-0.734076280688068));
#34085=CARTESIAN_POINT('Ctrl Pts',(0.0589274235883146,-0.427893825490553,
-0.722292845040469));
#34086=CARTESIAN_POINT('Ctrl Pts',(0.389528140140729,-0.186620175848612,
-0.710509409392871));
#34087=CARTESIAN_POINT('Ctrl Pts',(0.370384657908538,0.222210391259072,
-0.698725973745272));
#34088=CARTESIAN_POINT('Ctrl Pts',(0.0186731451510285,0.431524702501478,
-0.686942538097674));
#34089=CARTESIAN_POINT('Ctrl Pts',(-0.349802496911123,0.253376493156109,
-0.675159102450075));
#34090=CARTESIAN_POINT('Ctrl Pts',(-0.404196054900214,-0.152274280217354,
-0.663375666802478));
#34091=CARTESIAN_POINT('Ctrl Pts',(-0.0956664401425461,-0.421200417285852,
-0.65159223115488));
#34092=CARTESIAN_POINT('Ctrl Pts',(0.298760545047307,-0.311935720951775,
-0.639808795507281));
#34093=CARTESIAN_POINT('Ctrl Pts',(0.424934362716365,0.0774119929706307,
-0.628025359859682));
#34094=CARTESIAN_POINT('Ctrl Pts',(0.169564870683152,0.397252527146217,
-0.616241924212084));
#34095=CARTESIAN_POINT('Ctrl Pts',(-0.238054740227906,0.36040497284757,
-0.604458488564485));
#34096=CARTESIAN_POINT('Ctrl Pts',(-0.431928017497127,-4.56541445331377E-5,
-0.592675052916888));
#34097=CARTESIAN_POINT('Ctrl Pts',(-0.237978546257431,-0.360455299666153,
-0.580891617269288));
#34098=CARTESIAN_POINT('Ctrl Pts',(0.169648862642238,-0.397216658364245,
-0.569108181621692));
#34099=CARTESIAN_POINT('Ctrl Pts',(0.4249506944438,-0.0773221771287707,
-0.557324745974091));
#34100=CARTESIAN_POINT('Ctrl Pts',(0.298694639259925,0.311998916243858,
-0.545541310326495));
#34101=CARTESIAN_POINT('Ctrl Pts',(-0.0957555757394711,0.421180105019685,
-0.533757874678895));
#34102=CARTESIAN_POINT('Ctrl Pts',(-0.404228063824008,0.152188973891156,
-0.521974439031298));
#34103=CARTESIAN_POINT('Ctrl Pts',(-0.349749255950003,-0.25345072347495,
-0.510191003383699));
#34104=CARTESIAN_POINT('Ctrl Pts',(0.0187650109166624,-0.431520203035271,
-0.498407567736101));
#34105=CARTESIAN_POINT('Ctrl Pts',(0.370430410506412,-0.222133118336476,
-0.486624132088503));
#34106=CARTESIAN_POINT('Ctrl Pts',(0.389491002299994,0.186704500220892,
-0.474840696440904));
#34107=CARTESIAN_POINT('Ctrl Pts',(0.0588325206532684,0.427902495657323,
-0.463057260793306));
#34108=CARTESIAN_POINT('Ctrl Pts',(-0.324650941531368,0.284892220747562,
-0.451273825145707));
#34109=CARTESIAN_POINT('Ctrl Pts',(-0.4166344055083,-0.113919196908045,
-0.439490389498109));
#34110=CARTESIAN_POINT('Ctrl Pts',(-0.134527075591703,-0.41044400009082,
-0.42770695385051));
#34111=CARTESIAN_POINT('Ctrl Pts',(0.268370423941152,-0.338436296563816,
-0.415923518202913));
#34112=CARTESIAN_POINT('Ctrl Pts',(0.430301494337237,0.0374491021109036,
-0.404140082555314));
#34113=CARTESIAN_POINT('Ctrl Pts',(0.205870263629731,0.379709422889672,
-0.392356646907716));
#34114=CARTESIAN_POINT('Ctrl Pts',(-0.203409288155115,0.381033427365681,
-0.380573211260117));
#34115=CARTESIAN_POINT('Ctrl Pts',(-0.430050197796199,0.0402323085701024,
-0.368789775612519));
#34116=CARTESIAN_POINT('Ctrl Pts',(-0.270554442339733,-0.336692894207642,
-0.357006339964921));
#34117=CARTESIAN_POINT('Ctrl Pts',(0.13186874491508,-0.411305780886562,
-0.345222904317323));
#34118=CARTESIAN_POINT('Ctrl Pts',(0.415888644234946,-0.116612378724581,
-0.333439468669723));
#34119=CARTESIAN_POINT('Ctrl Pts',(0.326487359344952,0.282785812016435,
-0.321656033022126));
#34120=CARTESIAN_POINT('Ctrl Pts',(-0.056062820242291,0.428274177891669,
-0.309872597374527));
#34121=CARTESIAN_POINT('Ctrl Pts',(-0.388274898414303,0.1892205446798,-0.298089161726929));
#34122=CARTESIAN_POINT('Ctrl Pts',(-0.371859827628678,-0.219731836457348,
-0.286305726079331));
#34123=CARTESIAN_POINT('Ctrl Pts',(-0.021556493204716,-0.431389764308688,
-0.274522290431732));
#34124=CARTESIAN_POINT('Ctrl Pts',(0.348102144995012,-0.255708247637481,
-0.262738854784134));
#34125=CARTESIAN_POINT('Ctrl Pts',(0.40520424508076,0.149570490247016,-0.250955419136536));
#34126=CARTESIAN_POINT('Ctrl Pts',(0.0984785470653985,0.420551763812434,
-0.239171983488937));
#34127=CARTESIAN_POINT('Ctrl Pts',(-0.296669797159729,0.313924900237974,
-0.227388547841339));
#34128=CARTESIAN_POINT('Ctrl Pts',(-0.425442066452478,-0.0745711906566084,
-0.215605112193741));
#34129=CARTESIAN_POINT('Ctrl Pts',(-0.172215243183067,-0.396110734282261,
-0.203821676546142));
#34130=CARTESIAN_POINT('Ctrl Pts',(0.235641461137884,-0.361987454874687,
-0.192038240898544));
#34131=CARTESIAN_POINT('Ctrl Pts',(0.431918699354223,-0.00284014453923051,
-0.180254805250946));
#34132=CARTESIAN_POINT('Ctrl Pts',(0.240381494172507,0.358857206339876,
-0.168471369603347));
#34133=CARTESIAN_POINT('Ctrl Pts',(-0.166991090224279,0.398341354967106,
-0.156687933955749));
#34134=CARTESIAN_POINT('Ctrl Pts',(-0.424424745367948,0.0801594831068888,
-0.14490449830815));
#34135=CARTESIAN_POINT('Ctrl Pts',(-0.300772240961904,-0.309995956741533,
-0.133121062660552));
#34136=CARTESIAN_POINT('Ctrl Pts',(0.0929388882476368,-0.421811116816654,
-0.121337627012954));
#34137=CARTESIAN_POINT('Ctrl Pts',(0.403203246345024,-0.154885102364198,
-0.109554191365355));
#34138=CARTESIAN_POINT('Ctrl Pts',(0.351432873055049,0.251105949215736,
-0.0977707557177572));
#34139=CARTESIAN_POINT('Ctrl Pts',(-0.015877769156476,0.431640433219955,
-0.0859873200701588));
#34140=CARTESIAN_POINT('Ctrl Pts',(-0.368945120930351,0.224594532394832,
-0.0742038844225605));
#34141=CARTESIAN_POINT('Ctrl Pts',(-0.390716151659747,-0.184081665337648,
-0.0624204487749621));
#34142=CARTESIAN_POINT('Ctrl Pts',(-0.0617160825469674,-0.427531151377359,
-0.0506370131273638));
#34143=CARTESIAN_POINT('Ctrl Pts',(0.322789858477346,-0.286995150545506,
-0.0388535774797655));
#34144=CARTESIAN_POINT('Ctrl Pts',(0.417291074714279,0.111018472500347,
-0.0270701418321671));
#34145=CARTESIAN_POINT('Ctrl Pts',(0.137451704528447,0.409757701471928,
-0.0152867061845688));
#34146=CARTESIAN_POINT('Ctrl Pts',(-0.266488825482632,0.339772786046305,
-0.0035032705369704));
#34147=CARTESIAN_POINT('Ctrl Pts',(-0.375198930576758,0.0909294594581953,
0.00435235322809514));
#34148=CARTESIAN_POINT('Ctrl Pts',(-0.365539990181895,-0.0293535208949691,
0.0082801651106279));
#34149=CARTESIAN_POINT('Ctrl Pts',(-0.379394159804248,-0.0355742169162846,
-0.808280165110628));
#34150=CARTESIAN_POINT('Ctrl Pts',(-0.367688264555163,-0.160415989350353,
-0.804352353228095));
#34151=CARTESIAN_POINT('Ctrl Pts',(-0.21175580134227,-0.395589331381355,
-0.79649672946303));
#34152=CARTESIAN_POINT('Ctrl Pts',(0.214234400802117,-0.394707588870624,
-0.784713293815431));
#34153=CARTESIAN_POINT('Ctrl Pts',(0.447020121557459,-0.0387189987127072,
-0.772929858167834));
#34154=CARTESIAN_POINT('Ctrl Pts',(0.278853084066004,0.351678622682965,
-0.761146422520234));
#34155=CARTESIAN_POINT('Ctrl Pts',(-0.13991053338606,0.426493565906307,
-0.749362986872636));
#34156=CARTESIAN_POINT('Ctrl Pts',(-0.432936448244949,0.118268533418297,
-0.737579551225038));
#34157=CARTESIAN_POINT('Ctrl Pts',(-0.337293711272416,-0.29609768721738,
-0.72579611557744));
#34158=CARTESIAN_POINT('Ctrl Pts',(0.0612319751493615,-0.44462802704646,
-0.71401267992984));
#34159=CARTESIAN_POINT('Ctrl Pts',(0.404761924833321,-0.193918574308719,
-0.702229244282244));
#34160=CARTESIAN_POINT('Ctrl Pts',(0.384869773489609,0.230900662661991,
-0.690445808634644));
#34161=CARTESIAN_POINT('Ctrl Pts',(0.0194034201772741,0.448400901497184,
-0.678662372987047));
#34162=CARTESIAN_POINT('Ctrl Pts',(-0.363482679095007,0.263285617928224,
-0.666878937339448));
#34163=CARTESIAN_POINT('Ctrl Pts',(-0.420003476853659,-0.158229468970116,
-0.65509550169185));
#34164=CARTESIAN_POINT('Ctrl Pts',(-0.0994077923100996,-0.437672851002821,
-0.643312066044252));
#34165=CARTESIAN_POINT('Ctrl Pts',(0.310444563090901,-0.324134997772164,
-0.631528630396652));
#34166=CARTESIAN_POINT('Ctrl Pts',(0.441552824704159,0.0804394446795438,
-0.619745194749055));
#34167=CARTESIAN_POINT('Ctrl Pts',(0.176196265094044,0.4127883995095,-0.607961759101456));
#34168=CARTESIAN_POINT('Ctrl Pts',(-0.247364657237681,0.37449979987731,
-0.596178323453858));
#34169=CARTESIAN_POINT('Ctrl Pts',(-0.448819989458054,-4.74396006692321E-5,
-0.584394887806259));
#34170=CARTESIAN_POINT('Ctrl Pts',(-0.247285483450293,-0.374552094892382,
-0.572611452158662));
#34171=CARTESIAN_POINT('Ctrl Pts',(0.176283541836149,-0.41275112796032,
-0.560828016511063));
#34172=CARTESIAN_POINT('Ctrl Pts',(0.441569795137746,-0.0803461162924902,
-0.549044580863465));
#34173=CARTESIAN_POINT('Ctrl Pts',(0.310376079839991,0.324200664524903,
-0.537261145215866));
#34174=CARTESIAN_POINT('Ctrl Pts',(-0.0995004138489923,0.437651744358387,
-0.525477709568268));
#34175=CARTESIAN_POINT('Ctrl Pts',(-0.420036737592155,0.158140826458231,
-0.513694273920669));
#34176=CARTESIAN_POINT('Ctrl Pts',(-0.363427355970227,-0.263362751268896,
-0.501910838273072));
#34177=CARTESIAN_POINT('Ctrl Pts',(0.0194988786571419,-0.448396226064488,
-0.490127402625472));
#34178=CARTESIAN_POINT('Ctrl Pts',(0.384917315393962,-0.230820367726493,
-0.478343966977875));
#34179=CARTESIAN_POINT('Ctrl Pts',(0.404723334594643,0.194006196464134,
-0.466560531330276));
#34180=CARTESIAN_POINT('Ctrl Pts',(0.0611333607215388,0.444637036288742,
-0.454777095682678));
#34181=CARTESIAN_POINT('Ctrl Pts',(-0.337347489056148,0.296033872156611,
-0.442993660035079));
#34182=CARTESIAN_POINT('Ctrl Pts',(-0.432928270251285,-0.118374383425309,
-0.431210224387481));
#34183=CARTESIAN_POINT('Ctrl Pts',(-0.13978820128123,-0.426495768580487,
-0.419426788739883));
#34184=CARTESIAN_POINT('Ctrl Pts',(0.278865935907763,-0.351671965935864,
-0.407643353092284));
#34185=CARTESIAN_POINT('Ctrl Pts',(0.447129855736918,0.0389136729588066,
-0.395859917444686));
#34186=CARTESIAN_POINT('Ctrl Pts',(0.213921500363513,0.394559214208881,
-0.384076481797088));
#34187=CARTESIAN_POINT('Ctrl Pts',(-0.211364280313341,0.395934998253659,
-0.37229304614949));
#34188=CARTESIAN_POINT('Ctrl Pts',(-0.446868731414507,0.0418057259006754,
-0.360509610501891));
#34189=CARTESIAN_POINT('Ctrl Pts',(-0.281135367560537,-0.349860382071373,
-0.348726174854292));
#34190=CARTESIAN_POINT('Ctrl Pts',(0.137025907801932,-0.427391252161065,
-0.336942739206695));
#34191=CARTESIAN_POINT('Ctrl Pts',(0.432153343519779,-0.121172891013474,
-0.325159303559096));
#34192=CARTESIAN_POINT('Ctrl Pts',(0.33925572605478,0.293845085353713,-0.313375867911498));
#34193=CARTESIAN_POINT('Ctrl Pts',(-0.0582553420265235,0.445023254384683,
-0.301592432263899));
#34194=CARTESIAN_POINT('Ctrl Pts',(-0.403459670949207,0.196620639153144,
-0.289808996616301));
#34195=CARTESIAN_POINT('Ctrl Pts',(-0.386402634594751,-0.228325175787054,
-0.278025560968703));
#34196=CARTESIAN_POINT('Ctrl Pts',(-0.0223995310814905,-0.448260686100608,
-0.266242125321104));
#34197=CARTESIAN_POINT('Ctrl Pts',(0.361715829300251,-0.265708563371338,
-0.254458689673506));
#34198=CARTESIAN_POINT('Ctrl Pts',(0.421051095641684,0.155419938361253,
-0.242675254025907));
#34199=CARTESIAN_POINT('Ctrl Pts',(0.102329875963721,0.436998829792555,
-0.23089181837831));
#34200=CARTESIAN_POINT('Ctrl Pts',(-0.308272049600575,0.326201970485431,
-0.219108382730711));
#34201=CARTESIAN_POINT('Ctrl Pts',(-0.442080383872028,-0.077487543406688,
-0.207324947083113));
#34202=CARTESIAN_POINT('Ctrl Pts',(-0.178950289165844,-0.411601953063784,
-0.195541511435514));
#34203=CARTESIAN_POINT('Ctrl Pts',(0.244856998896787,-0.376144170091689,
-0.183758075787916));
#34204=CARTESIAN_POINT('Ctrl Pts',(0.44881030689839,-0.0029512177736084,
-0.171974640140318));
#34205=CARTESIAN_POINT('Ctrl Pts',(0.249782406581518,0.372891502847418,
-0.160191204492719));
#34206=CARTESIAN_POINT('Ctrl Pts',(-0.173521828448066,0.413919809539174,
-0.148407768845121));
#34207=CARTESIAN_POINT('Ctrl Pts',(-0.441023277085855,0.0832943844936766,
-0.136624333197523));
#34208=CARTESIAN_POINT('Ctrl Pts',(-0.312534933019702,-0.322119372674637,
-0.124840897549924));
#34209=CARTESIAN_POINT('Ctrl Pts',(0.0965735704881073,-0.438307433956169,
-0.113057461902326));
#34210=CARTESIAN_POINT('Ctrl Pts',(0.41897184124026,-0.160942395941638,
-0.101274026254728));
#34211=CARTESIAN_POINT('Ctrl Pts',(0.365176816483849,0.260926276866517,
-0.0894905906071292));
#34212=CARTESIAN_POINT('Ctrl Pts',(-0.016498721770171,0.448521158247713,
-0.0777071549595309));
#34213=CARTESIAN_POINT('Ctrl Pts',(-0.383373938662503,0.23337804351267,
-0.0659237193119325));
#34214=CARTESIAN_POINT('Ctrl Pts',(-0.405996397467284,-0.191280786958474,
-0.0541402836643343));
#34215=CARTESIAN_POINT('Ctrl Pts',(-0.0641296938286871,-0.444251169364007,
-0.0423568480167359));
#34216=CARTESIAN_POINT('Ctrl Pts',(0.335413622201372,-0.298219043971149,
-0.0305734123691375));
#34217=CARTESIAN_POINT('Ctrl Pts',(0.433610620675813,0.115360216607358,
-0.0187899767215392));
#34218=CARTESIAN_POINT('Ctrl Pts',(0.142827207493804,0.425782629986974,
-0.00700654107394083));
#34219=CARTESIAN_POINT('Ctrl Pts',(-0.276910751325826,0.353060723254543,
0.00477689457365749));
#34220=CARTESIAN_POINT('Ctrl Pts',(-0.389872324194051,0.0944855563478826,
0.012632518338723));
#34221=CARTESIAN_POINT('Ctrl Pts',(-0.379835639027576,-0.0305014872963737,
0.0165603302212558));
#34222=CARTESIAN_POINT('Ctrl Pts',(-0.393673192958032,-0.0369131026361633,
-0.8));
#34223=CARTESIAN_POINT('Ctrl Pts',(-0.381526729866674,-0.166453470874877,
-0.796072188117467));
#34224=CARTESIAN_POINT('Ctrl Pts',(-0.219725528945438,-0.410477892610111,
-0.788216564352402));
#34225=CARTESIAN_POINT('Ctrl Pts',(0.222297413984273,-0.409562964479047,
-0.776433128704804));
#34226=CARTESIAN_POINT('Ctrl Pts',(0.463844352956859,-0.0401762427213809,
-0.764649693057204));
#34227=CARTESIAN_POINT('Ctrl Pts',(0.289348112335464,0.364914542591059,
-0.752866257409607));
#34228=CARTESIAN_POINT('Ctrl Pts',(-0.145176263216518,0.442545251495232,
-0.741082821762008));
#34229=CARTESIAN_POINT('Ctrl Pts',(-0.449230620778234,0.122719736121578,
-0.72929938611441));
#34230=CARTESIAN_POINT('Ctrl Pts',(-0.349988234794621,-0.307241740396052,
-0.717515950466812));
#34231=CARTESIAN_POINT('Ctrl Pts',(0.0635365267104093,-0.461362228602367,
-0.705732514819213));
#34232=CARTESIAN_POINT('Ctrl Pts',(0.419995709525912,-0.201216972768827,
-0.693949079171616));
#34233=CARTESIAN_POINT('Ctrl Pts',(0.39935488907068,0.239590934064909,-0.682165643524016));
#34234=CARTESIAN_POINT('Ctrl Pts',(0.0201336952035193,0.465277100492891,
-0.670382207876419));
#34235=CARTESIAN_POINT('Ctrl Pts',(-0.377162861278892,0.273194742700339,
-0.658598772228819));
#34236=CARTESIAN_POINT('Ctrl Pts',(-0.435810898807103,-0.164184657722877,
-0.646815336581222));
#34237=CARTESIAN_POINT('Ctrl Pts',(-0.103149144477653,-0.454145284719791,
-0.635031900933623));
#34238=CARTESIAN_POINT('Ctrl Pts',(0.322128581134495,-0.336334274592552,
-0.623248465286026));
#34239=CARTESIAN_POINT('Ctrl Pts',(0.458171286691953,0.0834668963884565,
-0.611465029638426));
#34240=CARTESIAN_POINT('Ctrl Pts',(0.182827659504937,0.428324271872783,
-0.599681593990828));
#34241=CARTESIAN_POINT('Ctrl Pts',(-0.256674574247458,0.388594626907048,
-0.587898158343229));
#34242=CARTESIAN_POINT('Ctrl Pts',(-0.465711961418981,-4.92250568048239E-5,
-0.576114722695633));
#34243=CARTESIAN_POINT('Ctrl Pts',(-0.256592420643155,-0.388648890118611,
-0.564331287048032));
#34244=CARTESIAN_POINT('Ctrl Pts',(0.18291822103006,-0.428285597556395,
-0.552547851400436));
#34245=CARTESIAN_POINT('Ctrl Pts',(0.458188895831691,-0.0833700554562097,
-0.540764415752836));
#34246=CARTESIAN_POINT('Ctrl Pts',(0.322057520420056,0.336402412805948,
-0.528980980105239));
#34247=CARTESIAN_POINT('Ctrl Pts',(-0.103245251958514,0.454123383697088,
-0.51719754445764));
#34248=CARTESIAN_POINT('Ctrl Pts',(-0.435845411360303,0.164092679025306,
-0.505414108810041));
#34249=CARTESIAN_POINT('Ctrl Pts',(-0.377105455990451,-0.273274779062841,
-0.493630673162444));
#34250=CARTESIAN_POINT('Ctrl Pts',(0.0202327463976213,-0.465272249093704,
-0.481847237514844));
#34251=CARTESIAN_POINT('Ctrl Pts',(0.399404220281511,-0.23950761711651,
-0.470063801867247));
#34252=CARTESIAN_POINT('Ctrl Pts',(0.419955666889291,0.201307892707376,
-0.458280366219648));
#34253=CARTESIAN_POINT('Ctrl Pts',(0.0634342007898095,0.461371576920162,
-0.44649693057205));
#34254=CARTESIAN_POINT('Ctrl Pts',(-0.350044036580928,0.307175523565658,
-0.434713494924451));
#34255=CARTESIAN_POINT('Ctrl Pts',(-0.44922213499427,-0.122829569942572,
-0.422930059276853));
#34256=CARTESIAN_POINT('Ctrl Pts',(-0.145049326970758,-0.442547537070155,
-0.411146623629255));
#34257=CARTESIAN_POINT('Ctrl Pts',(0.289361447874374,-0.364907635307912,
-0.399363187981656));
#34258=CARTESIAN_POINT('Ctrl Pts',(0.4639582171366,0.0403782438067095,-0.387579752334058));
#34259=CARTESIAN_POINT('Ctrl Pts',(0.221972737097294,0.409409005528091,
-0.37579631668646));
#34260=CARTESIAN_POINT('Ctrl Pts',(-0.219319272471568,0.410836569141637,
-0.364012881038862));
#34261=CARTESIAN_POINT('Ctrl Pts',(-0.463687265032815,0.0433791432312484,
-0.352229445391263));
#34262=CARTESIAN_POINT('Ctrl Pts',(-0.291716292781341,-0.363027869935104,
-0.340446009743666));
#34263=CARTESIAN_POINT('Ctrl Pts',(0.142183070688784,-0.443476723435568,
-0.328662574096066));
#34264=CARTESIAN_POINT('Ctrl Pts',(0.448418042804611,-0.125733403302368,
-0.316879138448469));
#34265=CARTESIAN_POINT('Ctrl Pts',(0.352024092764608,0.304904358690991,
-0.305095702800869));
#34266=CARTESIAN_POINT('Ctrl Pts',(-0.0604478638107563,0.461772330877697,
-0.293312267153272));
#34267=CARTESIAN_POINT('Ctrl Pts',(-0.418644443484112,0.204020733626488,
-0.281528831505673));
#34268=CARTESIAN_POINT('Ctrl Pts',(-0.400945441560823,-0.236918515116761,
-0.269745395858075));
#34269=CARTESIAN_POINT('Ctrl Pts',(-0.0232425689582656,-0.465131607892529,
-0.257961960210476));
#34270=CARTESIAN_POINT('Ctrl Pts',(0.375329513605492,-0.275708879105196,
-0.246178524562878));
#34271=CARTESIAN_POINT('Ctrl Pts',(0.436897946202607,0.161269386475489,
-0.234395088915279));
#34272=CARTESIAN_POINT('Ctrl Pts',(0.106181204862043,0.453445895772676,
-0.222611653267682));
#34273=CARTESIAN_POINT('Ctrl Pts',(-0.31987430204142,0.338479040732887,
-0.210828217620083));
#34274=CARTESIAN_POINT('Ctrl Pts',(-0.458718701291578,-0.0804038961567671,
-0.199044781972485));
#34275=CARTESIAN_POINT('Ctrl Pts',(-0.185685335148621,-0.427093171845309,
-0.187261346324886));
#34276=CARTESIAN_POINT('Ctrl Pts',(0.254072536655689,-0.390300885308689,
-0.175477910677288));
#34277=CARTESIAN_POINT('Ctrl Pts',(0.465701914442558,-0.00306229100798743,
-0.16369447502969));
#34278=CARTESIAN_POINT('Ctrl Pts',(0.259183318990528,0.386925799354961,
-0.151911039382092));
#34279=CARTESIAN_POINT('Ctrl Pts',(-0.180052566671852,0.429498264111241,
-0.140127603734493));
#34280=CARTESIAN_POINT('Ctrl Pts',(-0.457621808803763,0.086429285880465,
-0.128344168086895));
#34281=CARTESIAN_POINT('Ctrl Pts',(-0.3242976250775,-0.33424278860774,-0.116560732439296));
#34282=CARTESIAN_POINT('Ctrl Pts',(0.100208252728578,-0.454803751095683,
-0.104777296791698));
#34283=CARTESIAN_POINT('Ctrl Pts',(0.434740436135497,-0.166999689519078,
-0.0929938611440996));
#34284=CARTESIAN_POINT('Ctrl Pts',(0.378920759912649,0.270746604517297,
-0.0812104254965015));
#34285=CARTESIAN_POINT('Ctrl Pts',(-0.017119674383866,0.465401883275472,
-0.0694269898489029));
#34286=CARTESIAN_POINT('Ctrl Pts',(-0.397802756394656,0.242161554630506,
-0.0576435542013048));
#34287=CARTESIAN_POINT('Ctrl Pts',(-0.42127664327482,-0.1984799085793,-0.0458601185537062));
#34288=CARTESIAN_POINT('Ctrl Pts',(-0.0665433051104071,-0.460971187350655,
-0.0340766829061081));
#34289=CARTESIAN_POINT('Ctrl Pts',(0.348037385925398,-0.309442937396792,
-0.0222932472585096));
#34290=CARTESIAN_POINT('Ctrl Pts',(0.449930166637347,0.119701960714367,
-0.0105098116109113));
#34291=CARTESIAN_POINT('Ctrl Pts',(0.148202710459161,0.441807558502022,
0.00127362403668708));
#34292=CARTESIAN_POINT('Ctrl Pts',(-0.28733267716902,0.366348660462781,
0.0130570596842854));
#34293=CARTESIAN_POINT('Ctrl Pts',(-0.404545717811344,0.0980416532375701,
0.0209126834493509));
#34294=CARTESIAN_POINT('Ctrl Pts',(-0.394131287873257,-0.0316494536977783,
0.0248404953318837));
#34295=CARTESIAN_POINT('',(0.164868911863601,0.359387537208669,-1.11022302462516E-16));
#34296=CARTESIAN_POINT('Ctrl Pts',(0.16490687856217,0.359956139019385,-9.0205620750794E-17));
#34297=CARTESIAN_POINT('Ctrl Pts',(0.15191557524441,0.365209344759306,-8.50453259551574E-17));
#34298=CARTESIAN_POINT('Ctrl Pts',(0.138666480801866,0.36972436752869,-1.12193463301161E-16));
#34299=CARTESIAN_POINT('Ctrl Pts',(0.125198970394113,0.373451590864263,
-7.28583859910259E-17));
#34300=CARTESIAN_POINT('Ctrl Pts',(0.1077614757708,0.378277533811857,-2.52714042912841E-17));
#34301=CARTESIAN_POINT('Ctrl Pts',(0.0899575316801376,0.381783553779889,
-1.1966838214923E-16));
#34302=CARTESIAN_POINT('Ctrl Pts',(0.0719258827732591,0.384004455949837,
-1.2490009027033E-16));
#34303=CARTESIAN_POINT('Ctrl Pts',(0.0653106445601438,0.384819234286422,
-1.26819437505921E-16));
#34304=CARTESIAN_POINT('Ctrl Pts',(0.0586641660849231,0.385460608990607,
-2.41353700608386E-16));
#34305=CARTESIAN_POINT('Ctrl Pts',(0.0520091005880364,0.385929118179874,
-2.22044604925031E-16));
#34306=CARTESIAN_POINT('Ctrl Pts',(0.0301527436928502,0.387467781331137,
-1.58630279885535E-16));
#34307=CARTESIAN_POINT('Ctrl Pts',(0.00816286325548518,0.387151739749051,
-6.77153354539665E-17));
#34308=CARTESIAN_POINT('Ctrl Pts',(-0.0137135983350831,0.385041704764503,
6.93889390390723E-18));
#34309=CARTESIAN_POINT('Ctrl Pts',(-0.0205956652624267,0.384377913596879,
3.04242002786661E-17));
#34310=CARTESIAN_POINT('Ctrl Pts',(-0.0274664476022094,0.383536195767146,
1.30920738496616E-16));
#34311=CARTESIAN_POINT('Ctrl Pts',(-0.0343179685799315,0.382517420028697,
1.2490009027033E-16));
#34312=CARTESIAN_POINT('Ctrl Pts',(-0.0394223585790314,0.381758431081924,
1.20414701304248E-16));
#34313=CARTESIAN_POINT('Ctrl Pts',(-0.0445135904220789,0.380901415994797,
-8.09570049575627E-17));
#34314=CARTESIAN_POINT('Ctrl Pts',(-0.0495799285321691,0.379948761826662,
-7.28583859910259E-17));
#34315=CARTESIAN_POINT('Ctrl Pts',(-0.0708814681958342,0.375943304609374,
-3.88075489983239E-17));
#34316=CARTESIAN_POINT('Ctrl Pts',(-0.0917880441950763,0.370244752838114,
6.22075423807223E-17));
#34317=CARTESIAN_POINT('Ctrl Pts',(-0.112062658453149,0.362907076418133,
3.12250225675825E-17));
#34318=CARTESIAN_POINT('Ctrl Pts',(-0.126357969121762,0.357733396530852,
9.37973661601609E-18));
#34319=CARTESIAN_POINT('Ctrl Pts',(-0.140339041692395,0.351743737927013,
-1.31114297266183E-16));
#34320=CARTESIAN_POINT('Ctrl Pts',(-0.153915171464246,0.344943241496427,
-1.83880688453542E-16));
#34321=CARTESIAN_POINT('Ctrl Pts',(-0.16029905866049,0.341745452227992,
-2.08692965203534E-16));
#34322=CARTESIAN_POINT('Ctrl Pts',(-0.166593284437042,0.33836822022888,
2.86834908564699E-17));
#34323=CARTESIAN_POINT('Ctrl Pts',(-0.172787641053473,0.334811292422105,
3.98986399474666E-17));
#34324=CARTESIAN_POINT('Ctrl Pts',(-0.177212136992572,0.332270655256496,
4.7909380155397E-17));
#34325=CARTESIAN_POINT('Ctrl Pts',(-0.18158449532273,0.329638806505941,
8.55558718079072E-17));
#34326=CARTESIAN_POINT('Ctrl Pts',(-0.185890887386474,0.326922548472184,
9.54097911787244E-17));
#34327=CARTESIAN_POINT('Ctrl Pts',(-0.201503676834758,0.317074777033701,
1.31135095818816E-16));
#34328=CARTESIAN_POINT('Ctrl Pts',(-0.216288937869559,0.306098120574002,
5.49150136144099E-16));
#34329=CARTESIAN_POINT('Ctrl Pts',(-0.230088091924545,0.294011759332474,
3.76434994286967E-16));
#34330=CARTESIAN_POINT('Ctrl Pts',(-0.241247208182782,0.284237746396911,
2.38394309878886E-16));
#34331=CARTESIAN_POINT('Ctrl Pts',(-0.251761185600929,0.273737308875212,
4.47279742850693E-17));
#34332=CARTESIAN_POINT('Ctrl Pts',(-0.261602104460616,0.262589914361208,
1.16226472890446E-16));
#34333=CARTESIAN_POINT('Ctrl Pts',(-0.266706827128519,0.256807491167292,
1.53314473691571E-16));
#34334=CARTESIAN_POINT('Ctrl Pts',(-0.271630267579517,0.250850862471227,
1.68452480644874E-16));
#34335=CARTESIAN_POINT('Ctrl Pts',(-0.276367301437873,0.244730512258966,
2.0122792321331E-16));
#34336=CARTESIAN_POINT('Ctrl Pts',(-0.280626564308997,0.239227452496922,
2.30697677872155E-16));
#34337=CARTESIAN_POINT('Ctrl Pts',(-0.284737477503322,0.233588071488557,
2.55208427141222E-16));
#34338=CARTESIAN_POINT('Ctrl Pts',(-0.288679976022965,0.227844262538324,
2.53269627492614E-16));
#34339=CARTESIAN_POINT('Ctrl Pts',(-0.30046346930519,0.210676942413222,
2.47474867514614E-16));
#34340=CARTESIAN_POINT('Ctrl Pts',(-0.310775801429704,0.192543893686169,
5.6438178067964E-17));
#34341=CARTESIAN_POINT('Ctrl Pts',(-0.319548265568143,0.173669187960367,
9.62771529167128E-17));
#34342=CARTESIAN_POINT('Ctrl Pts',(-0.326817975209212,0.158027786864642,
1.29291568818306E-16));
#34343=CARTESIAN_POINT('Ctrl Pts',(-0.333029562487829,0.141876008150292,
-5.70505344164234E-17));
#34344=CARTESIAN_POINT('Ctrl Pts',(-0.338118323450462,0.125333828641746,
-7.02563007770607E-17));
#34345=CARTESIAN_POINT('Ctrl Pts',(-0.339619932817922,0.120452504505944,
-7.41531044621277E-17));
#34346=CARTESIAN_POINT('Ctrl Pts',(-0.341023607935996,0.115537177016873,
-5.42574854396036E-17));
#34347=CARTESIAN_POINT('Ctrl Pts',(-0.342327260445792,0.110590939653933,
-4.9439619065339E-17));
#34348=CARTESIAN_POINT('Ctrl Pts',(-0.34373737166573,0.105240783266747,
-4.42283166826413E-17));
#34349=CARTESIAN_POINT('Ctrl Pts',(-0.345028225001506,0.0998626025727999,
-1.15077223344712E-16));
#34350=CARTESIAN_POINT('Ctrl Pts',(-0.346197043797798,0.0944662829877048,
-1.06685493772574E-16));
#34351=CARTESIAN_POINT('Ctrl Pts',(-0.350565249921096,0.0742987118212727,
-7.53232290499652E-17));
#34352=CARTESIAN_POINT('Ctrl Pts',(-0.353239911805653,0.0538525131720056,
-1.31602125640592E-16));
#34353=CARTESIAN_POINT('Ctrl Pts',(-0.354123093098514,0.0333368081597991,
-1.83013326715553E-16));
#34354=CARTESIAN_POINT('Ctrl Pts',(-0.355006274391374,0.0128211031475926,
-2.34424527790514E-16));
#34355=CARTESIAN_POINT('Ctrl Pts',(-0.354098424041937,-0.00776559513595167,
-3.76796022219801E-17));
#34356=CARTESIAN_POINT('Ctrl Pts',(-0.351244341336214,-0.0282055544935644,
-1.73472347597681E-18));
#34357=CARTESIAN_POINT('Ctrl Pts',(-0.39480767064478,-0.000104727820695843,
-0.0511159844630761));
#34358=CARTESIAN_POINT('Ctrl Pts',(-0.394952852228362,-0.0583396144091755,
-0.0493640291599528));
#34359=CARTESIAN_POINT('Ctrl Pts',(-0.382867850318616,-0.116517499431679,
-0.0476120738568295));
#34360=CARTESIAN_POINT('Ctrl Pts',(-0.35824210576739,-0.168788211172892,
-0.0458601185537063));
#34361=CARTESIAN_POINT('Ctrl Pts',(-0.303032197220016,-0.285977001503084,
-0.0419323066711736));
#34362=CARTESIAN_POINT('Ctrl Pts',(-0.18478775116521,-0.37347409442687,
-0.0380044947886408));
#34363=CARTESIAN_POINT('Ctrl Pts',(-0.0565687462985088,-0.391967932563119,
-0.034076682906108));
#34364=CARTESIAN_POINT('Ctrl Pts',(0.0716502585681938,-0.410461770699368,
-0.0301488710235753));
#34365=CARTESIAN_POINT('Ctrl Pts',(0.209843822246795,-0.35995235404808,
-0.0262210591410425));
#34366=CARTESIAN_POINT('Ctrl Pts',(0.295922734204754,-0.263173496037244,
-0.0222932472585097));
#34367=CARTESIAN_POINT('Ctrl Pts',(0.382001646162714,-0.166394638026406,
-0.0183654353759768));
#34368=CARTESIAN_POINT('Ctrl Pts',(0.415965906400031,-0.023346338656019,
-0.0144376234934441));
#34369=CARTESIAN_POINT('Ctrl Pts',(0.382660127155657,0.101862077327118,
-0.0105098116109112));
#34370=CARTESIAN_POINT('Ctrl Pts',(0.35295423526798,0.213537220590751,-0.00700654107394087));
#34371=CARTESIAN_POINT('Ctrl Pts',(0.26973431106858,0.31102054676347,-0.00350327053697048));
#34372=CARTESIAN_POINT('Ctrl Pts',(0.16490687856217,0.359956139019385,-9.0205620750794E-17));
#34373=CARTESIAN_POINT('',(0.200169762396267,-0.290577011776231,-0.8));
#34374=CARTESIAN_POINT('Ctrl Pts',(0.20016976239627,-0.290577011776229,
-0.8));
#34375=CARTESIAN_POINT('Ctrl Pts',(0.190306482557462,-0.298378649280142,
-0.8));
#34376=CARTESIAN_POINT('Ctrl Pts',(0.180035217986072,-0.305605974903153,
-0.8));
#34377=CARTESIAN_POINT('Ctrl Pts',(0.169385277865962,-0.312209719032721,
-0.8));
#34378=CARTESIAN_POINT('Ctrl Pts',(0.15368545462129,-0.321944761147323,
-0.8));
#34379=CARTESIAN_POINT('Ctrl Pts',(0.137163515983412,-0.330326466268722,
-0.8));
#34380=CARTESIAN_POINT('Ctrl Pts',(0.120002461186164,-0.337372376845852,
-0.8));
#34381=CARTESIAN_POINT('Ctrl Pts',(0.114202478233197,-0.339753708396756,
-0.8));
#34382=CARTESIAN_POINT('Ctrl Pts',(0.108338590630642,-0.341978348949641,
-0.8));
#34383=CARTESIAN_POINT('Ctrl Pts',(0.102419584724057,-0.344047141145212,
-0.8));
#34384=CARTESIAN_POINT('Ctrl Pts',(0.0863681048207357,-0.349657403556746,
-0.8));
#34385=CARTESIAN_POINT('Ctrl Pts',(0.0699088827807137,-0.354124467710462,
-0.8));
#34386=CARTESIAN_POINT('Ctrl Pts',(0.0531808102711496,-0.357460993149358,
-0.8));
#34387=CARTESIAN_POINT('Ctrl Pts',(0.0464251329711486,-0.358808457966691,
-0.8));
#34388=CARTESIAN_POINT('Ctrl Pts',(0.0396254752335136,-0.359971281620787,
-0.8));
#34389=CARTESIAN_POINT('Ctrl Pts',(0.0327905864186719,-0.360949250929142,
-0.8));
#34390=CARTESIAN_POINT('Ctrl Pts',(0.0272161405436249,-0.361746869899189,
-0.8));
#34391=CARTESIAN_POINT('Ctrl Pts',(0.021618656359546,-0.362421254066241,
-0.8));
#34392=CARTESIAN_POINT('Ctrl Pts',(0.0160166140773693,-0.362971297712489,
-0.8));
#34393=CARTESIAN_POINT('Ctrl Pts',(-0.00503455293683043,-0.36503823331901,
-0.8));
#34394=CARTESIAN_POINT('Ctrl Pts',(-0.0261975225172284,-0.365360927269529,
-0.8));
#34395=CARTESIAN_POINT('Ctrl Pts',(-0.0472196904885675,-0.363958480743644,
-0.8));
#34396=CARTESIAN_POINT('Ctrl Pts',(-0.0621644164904353,-0.362961477052578,
-0.8));
#34397=CARTESIAN_POINT('Ctrl Pts',(-0.0770386390163482,-0.361091594946764,
-0.8));
#34398=CARTESIAN_POINT('Ctrl Pts',(-0.0917535281674465,-0.358339847735959,
-0.8));
#34399=CARTESIAN_POINT('Ctrl Pts',(-0.098600486653832,-0.357059437212716,
-0.8));
#34400=CARTESIAN_POINT('Ctrl Pts',(-0.105412934492697,-0.355587902723317,
-0.8));
#34401=CARTESIAN_POINT('Ctrl Pts',(-0.112181716986231,-0.353923330911631,
-0.8));
#34402=CARTESIAN_POINT('Ctrl Pts',(-0.116968091051461,-0.352746270878047,
-0.8));
#34403=CARTESIAN_POINT('Ctrl Pts',(-0.12172870669558,-0.351473523653454,
-0.8));
#34404=CARTESIAN_POINT('Ctrl Pts',(-0.126452665500413,-0.350107261479429,
-0.8));
#34405=CARTESIAN_POINT('Ctrl Pts',(-0.143772909154477,-0.345097904978429,
-0.8));
#34406=CARTESIAN_POINT('Ctrl Pts',(-0.160631985153867,-0.338825890448156,
-0.8));
#34407=CARTESIAN_POINT('Ctrl Pts',(-0.176878423079808,-0.331288354642354,
-0.8));
#34408=CARTESIAN_POINT('Ctrl Pts',(-0.191156219349634,-0.324664170245606,
-0.8));
#34409=CARTESIAN_POINT('Ctrl Pts',(-0.204961220157989,-0.317062223203108,
-0.8));
#34410=CARTESIAN_POINT('Ctrl Pts',(-0.218247963486141,-0.308569468881161,
-0.8));
#34411=CARTESIAN_POINT('Ctrl Pts',(-0.224802936957718,-0.304379594966531,
-0.8));
#34412=CARTESIAN_POINT('Ctrl Pts',(-0.231231666263234,-0.299972654194668,
-0.8));
#34413=CARTESIAN_POINT('Ctrl Pts',(-0.237527947545455,-0.295357764267163,
-0.8));
#34414=CARTESIAN_POINT('Ctrl Pts',(-0.242759499159343,-0.291523273118186,
-0.8));
#34415=CARTESIAN_POINT('Ctrl Pts',(-0.247901647723441,-0.287543179968104,
-0.8));
#34416=CARTESIAN_POINT('Ctrl Pts',(-0.252932096788435,-0.283438407946873,
-0.8));
#34417=CARTESIAN_POINT('Ctrl Pts',(-0.269421005257647,-0.269983702557636,
-0.8));
#34418=CARTESIAN_POINT('Ctrl Pts',(-0.284755423501557,-0.255163052021068,
-0.8));
#34419=CARTESIAN_POINT('Ctrl Pts',(-0.298831470631119,-0.239191762115533,
-0.8));
#34420=CARTESIAN_POINT('Ctrl Pts',(-0.311279850930076,-0.225067293166332,
-0.8));
#34421=CARTESIAN_POINT('Ctrl Pts',(-0.322744216465833,-0.210041634577153,
-0.8));
#34422=CARTESIAN_POINT('Ctrl Pts',(-0.333132984278499,-0.194238114040248,
-0.8));
#34423=CARTESIAN_POINT('Ctrl Pts',(-0.336326088260912,-0.189380725245687,
-0.8));
#34424=CARTESIAN_POINT('Ctrl Pts',(-0.339417416663507,-0.184449716680632,
-0.8));
#34425=CARTESIAN_POINT('Ctrl Pts',(-0.342403840382252,-0.179448352887251,
-0.8));
#34426=CARTESIAN_POINT('Ctrl Pts',(-0.345031246832228,-0.175048235312868,
-0.8));
#34427=CARTESIAN_POINT('Ctrl Pts',(-0.347572530726044,-0.170601882868889,
-0.8));
#34428=CARTESIAN_POINT('Ctrl Pts',(-0.350026053733772,-0.166112593145433,
-0.8));
#34429=CARTESIAN_POINT('Ctrl Pts',(-0.361014852315233,-0.146006036007191,
-0.8));
#34430=CARTESIAN_POINT('Ctrl Pts',(-0.370248738553699,-0.125038049791925,
-0.8));
#34431=CARTESIAN_POINT('Ctrl Pts',(-0.377580893333559,-0.103434617138351,
-0.8));
#34432=CARTESIAN_POINT('Ctrl Pts',(-0.384469721870555,-0.0831373992223077,
-0.8));
#34433=CARTESIAN_POINT('Ctrl Pts',(-0.38968034295518,-0.062277824821227,
-0.8));
#34434=CARTESIAN_POINT('Ctrl Pts',(-0.393046362175399,-0.0410217592765385,
-0.8));
#34435=CARTESIAN_POINT('Ctrl Pts',(-0.393262980232635,-0.0396538385008335,
-0.8));
#34436=CARTESIAN_POINT('Ctrl Pts',(-0.393471941134707,-0.0382842719653916,
-0.8));
#34437=CARTESIAN_POINT('Ctrl Pts',(-0.393673192958032,-0.0369131026361633,
-0.8));
#34438=CARTESIAN_POINT('Ctrl Pts',(0.200169762396267,-0.290577011776231,
-0.8));
#34439=CARTESIAN_POINT('Ctrl Pts',(0.284652167513286,-0.231483393422286,
-0.79649672946303));
#34440=CARTESIAN_POINT('Ctrl Pts',(0.407768891830231,-0.0227977591064635,
-0.789065647043525));
#34441=CARTESIAN_POINT('Ctrl Pts',(0.257863027527083,0.32520678286678,-0.777706752741491));
#34442=CARTESIAN_POINT('Ctrl Pts',(-0.129379073725142,0.394390194728457,
-0.765923317093891));
#34443=CARTESIAN_POINT('Ctrl Pts',(-0.334426670897645,0.178706874259964,
-0.757006559445049));
#34444=CARTESIAN_POINT('Ctrl Pts',(-0.352510997026901,0.0316401701347851,
-0.752017613678738));
#34445=CARTESIAN_POINT('Ctrl Pts',(-0.352246168648579,0.000295985828685053,
-0.75095647979496));
#34446=CARTESIAN_POINT('Origin',(-9.39637619619865E-17,-2.12715743287418E-17,
-0.8));
#34447=CARTESIAN_POINT('',(0.339445800272064,0.0945763675695885,-0.8));
#34448=CARTESIAN_POINT('Ctrl Pts',(-0.278859905177389,0.281069071148119,
-0.800000000000001));
#34449=CARTESIAN_POINT('Ctrl Pts',(-0.268475009873748,0.290477793453348,
-0.800000000000001));
#34450=CARTESIAN_POINT('Ctrl Pts',(-0.25759371033593,0.29928240376613,-0.800000000000001));
#34451=CARTESIAN_POINT('Ctrl Pts',(-0.24623586993354,0.307422754976269,
-0.800000000000001));
#34452=CARTESIAN_POINT('Ctrl Pts',(-0.231529933077798,0.317962742037073,
-0.800000000000001));
#34453=CARTESIAN_POINT('Ctrl Pts',(-0.216025100159335,0.327389965026806,
-0.8));
#34454=CARTESIAN_POINT('Ctrl Pts',(-0.199863609434863,0.335689279670645,
-0.8));
#34455=CARTESIAN_POINT('Ctrl Pts',(-0.193934478213887,0.33873403132174,
-0.8));
#34456=CARTESIAN_POINT('Ctrl Pts',(-0.187916258974387,0.341626769901992,
-0.8));
#34457=CARTESIAN_POINT('Ctrl Pts',(-0.181830402402309,0.344360193317562,
-0.8));
#34458=CARTESIAN_POINT('Ctrl Pts',(-0.161843412934983,0.353337221344707,
-0.8));
#34459=CARTESIAN_POINT('Ctrl Pts',(-0.1410918738637,0.360619192332112,-0.8));
#34460=CARTESIAN_POINT('Ctrl Pts',(-0.119828519294813,0.366177991655667,
-0.8));
#34461=CARTESIAN_POINT('Ctrl Pts',(-0.113139294026385,0.367926730819884,
-0.8));
#34462=CARTESIAN_POINT('Ctrl Pts',(-0.106399340447922,0.369504553265394,
-0.8));
#34463=CARTESIAN_POINT('Ctrl Pts',(-0.0996164460696241,0.370909525367399,
-0.8));
#34464=CARTESIAN_POINT('Ctrl Pts',(-0.094563178597882,0.371956231894996,
-0.8));
#34465=CARTESIAN_POINT('Ctrl Pts',(-0.0894884791182313,0.372906381891583,
-0.8));
#34466=CARTESIAN_POINT('Ctrl Pts',(-0.0844041867529184,0.37375817163292,
-0.8));
#34467=CARTESIAN_POINT('Ctrl Pts',(-0.0630272839706001,0.377339520851892,
-0.8));
#34468=CARTESIAN_POINT('Ctrl Pts',(-0.0414376343613116,0.379195383149306,
-0.8));
#34469=CARTESIAN_POINT('Ctrl Pts',(-0.0198763137447139,0.37929474254576,
-0.8));
#34470=CARTESIAN_POINT('Ctrl Pts',(-0.00467371801110023,0.37936479951321,
-0.8));
#34471=CARTESIAN_POINT('Ctrl Pts',(0.0105151140659063,0.378560564121899,
-0.8));
#34472=CARTESIAN_POINT('Ctrl Pts',(0.0256032632385705,0.376855601414503,
-0.8));
#34473=CARTESIAN_POINT('Ctrl Pts',(0.0326988428047688,0.376053800053098,
-0.8));
#34474=CARTESIAN_POINT('Ctrl Pts',(0.039772093686793,0.375052608106074,
-0.8));
#34475=CARTESIAN_POINT('Ctrl Pts',(0.0468135179423963,0.373848268808225,
-0.8));
#34476=CARTESIAN_POINT('Ctrl Pts',(0.0518424079668323,0.372988145960754,
-0.8));
#34477=CARTESIAN_POINT('Ctrl Pts',(0.0568537870825205,0.372024437031212,
-0.8));
#34478=CARTESIAN_POINT('Ctrl Pts',(0.0618323347754462,0.370958760988685,
-0.8));
#34479=CARTESIAN_POINT('Ctrl Pts',(0.0798818210244701,0.36709520352938,
-0.8));
#34480=CARTESIAN_POINT('Ctrl Pts',(0.0975435693854742,0.361886824549212,
-0.8));
#34481=CARTESIAN_POINT('Ctrl Pts',(0.114662125904877,0.355296980178815,
-0.8));
#34482=CARTESIAN_POINT('Ctrl Pts',(0.128506110242191,0.34996769308935,-0.8));
#34483=CARTESIAN_POINT('Ctrl Pts',(0.141994842420674,0.343734144970146,
-0.8));
#34484=CARTESIAN_POINT('Ctrl Pts',(0.155074724264531,0.33666131221326,-0.8));
#34485=CARTESIAN_POINT('Ctrl Pts',(0.161859575051541,0.332992462947662,
-0.8));
#34486=CARTESIAN_POINT('Ctrl Pts',(0.168534289696369,0.329097603646923,
-0.8));
#34487=CARTESIAN_POINT('Ctrl Pts',(0.175090444399602,0.324984809875769,
-0.8));
#34488=CARTESIAN_POINT('Ctrl Pts',(0.180985353825959,0.321286827160645,
-0.8));
#34489=CARTESIAN_POINT('Ctrl Pts',(0.186787985179493,0.317409747559543,
-0.8));
#34490=CARTESIAN_POINT('Ctrl Pts',(0.192468510837425,0.313376595109622,
-0.8));
#34491=CARTESIAN_POINT('Ctrl Pts',(0.2094466944668,0.301322146802642,-0.8));
#34492=CARTESIAN_POINT('Ctrl Pts',(0.225376684523978,0.287854111002053,
-0.8));
#34493=CARTESIAN_POINT('Ctrl Pts',(0.240116755803838,0.273159151623289,
-0.8));
#34494=CARTESIAN_POINT('Ctrl Pts',(0.252331794876079,0.260981496605985,
-0.8));
#34495=CARTESIAN_POINT('Ctrl Pts',(0.263729437817635,0.247960058877349,
-0.8));
#34496=CARTESIAN_POINT('Ctrl Pts',(0.274207594017334,0.234185164645355,
-0.8));
#34497=CARTESIAN_POINT('Ctrl Pts',(0.277299531732945,0.230120411821221,
-0.8));
#34498=CARTESIAN_POINT('Ctrl Pts',(0.280311253869966,0.225989986271888,
-0.8));
#34499=CARTESIAN_POINT('Ctrl Pts',(0.283239733805565,0.221796072218523,
-0.8));
#34500=CARTESIAN_POINT('Ctrl Pts',(0.286407344655221,0.217259695685267,
-0.8));
#34501=CARTESIAN_POINT('Ctrl Pts',(0.289472662759133,0.212655910806126,
-0.8));
#34502=CARTESIAN_POINT('Ctrl Pts',(0.292429674704035,0.207993040211104,
-0.8));
#34503=CARTESIAN_POINT('Ctrl Pts',(0.303480889882578,0.190566534246487,
-0.8));
#34504=CARTESIAN_POINT('Ctrl Pts',(0.313038342233419,0.172294802880286,
-0.8));
#34505=CARTESIAN_POINT('Ctrl Pts',(0.320938020590327,0.153340401549331,
-0.8));
#34506=CARTESIAN_POINT('Ctrl Pts',(0.328837698947234,0.134386000218375,
-0.8));
#34507=CARTESIAN_POINT('Ctrl Pts',(0.335080537221356,0.114747687841751,
-0.8));
#34508=CARTESIAN_POINT('Ctrl Pts',(0.339445800272064,0.0945763675695893,
-0.8));
#34509=CARTESIAN_POINT('Origin',(0.,0.,-0.8));
#34510=CARTESIAN_POINT('Origin',(0.,0.,-0.953243520205039));
#34511=CARTESIAN_POINT('Ctrl Pts',(0.339445800272064,0.094576367569588,
-0.8));
#34512=CARTESIAN_POINT('Ctrl Pts',(0.308324917009509,0.206272908636879,
-0.796072188117467));
#34513=CARTESIAN_POINT('Ctrl Pts',(0.12785742430771,0.394733928544834,-0.788216564352402));
#34514=CARTESIAN_POINT('Ctrl Pts',(-0.247689876721063,0.326277103430375,
-0.776797737754082));
#34515=CARTESIAN_POINT('Ctrl Pts',(-0.352173024012217,0.104655642871124,
-0.769306723038295));
#34516=CARTESIAN_POINT('Ctrl Pts',(-0.352786263833399,-0.000190149253296124,
-0.76574352020504));
#34517=CARTESIAN_POINT('Ctrl Pts',(0.380892144526639,0.106124145404794,
-0.824840495331884));
#34518=CARTESIAN_POINT('Ctrl Pts',(0.345971400313757,0.231458838098676,
-0.820912683449351));
#34519=CARTESIAN_POINT('Ctrl Pts',(0.143468820351243,0.44293095522278,-0.813057059684284));
#34520=CARTESIAN_POINT('Ctrl Pts',(-0.291388392138657,0.363662793626005,
-0.801273624036688));
#34521=CARTESIAN_POINT('Ctrl Pts',(-0.46361938361485,-0.042696984818944,
-0.789490188389088));
#34522=CARTESIAN_POINT('Ctrl Pts',(-0.220067036752125,-0.410433220025444,
-0.77770675274149));
#34523=CARTESIAN_POINT('Ctrl Pts',(0.221336844762247,-0.409795607414138,
-0.765923317093893));
#34524=CARTESIAN_POINT('Ctrl Pts',(0.463871431563072,-0.0411298069848769,
-0.754139881446293));
#34525=CARTESIAN_POINT('Ctrl Pts',(0.289971644477912,0.364425190131086,
-0.742356445798696));
#34526=CARTESIAN_POINT('Ctrl Pts',(-0.144326642460796,0.442788711872689,
-0.730573010151097));
#34527=CARTESIAN_POINT('Ctrl Pts',(-0.449016693789206,0.123566658604731,
-0.7187895745035));
#34528=CARTESIAN_POINT('Ctrl Pts',(-0.350550328424412,-0.30659850382061,
-0.7070061388559));
#34529=CARTESIAN_POINT('Ctrl Pts',(0.0626760165915523,-0.461475781257629,
-0.695222703208302));
#34530=CARTESIAN_POINT('Ctrl Pts',(0.419623607977338,-0.201998157742978,
-0.683439267560704));
#34531=CARTESIAN_POINT('Ctrl Pts',(0.39979787554505,0.238850234477996,-0.671655831913105));
#34532=CARTESIAN_POINT('Ctrl Pts',(0.0209979054846499,0.465238442645313,
-0.659872396265508));
#34533=CARTESIAN_POINT('Ctrl Pts',(-0.376655426161442,0.273894673808823,
-0.648088960617908));
#34534=CARTESIAN_POINT('Ctrl Pts',(-0.436114792825645,-0.163375558641342,
-0.636305524970311));
#34535=CARTESIAN_POINT('Ctrl Pts',(-0.103992062925303,-0.453952994102977,
-0.624522089322712));
#34536=CARTESIAN_POINT('Ctrl Pts',(0.321503776225126,-0.336931711343498,
-0.612738653675114));
#34537=CARTESIAN_POINT('Ctrl Pts',(0.458325446868897,0.082616301207692,
-0.600955218027515));
#34538=CARTESIAN_POINT('Ctrl Pts',(0.183622446346355,0.427984184736038,
-0.589171782379917));
#34539=CARTESIAN_POINT('Ctrl Pts',(-0.255952831769196,0.38907044560016,
-0.577388346732319));
#34540=CARTESIAN_POINT('Ctrl Pts',(-0.465711284854635,0.000815248043422982,
-0.565604911084721));
#34541=CARTESIAN_POINT('Ctrl Pts',(-0.257313428960664,-0.388171951771344,
-0.553821475437122));
#34542=CARTESIAN_POINT('Ctrl Pts',(0.182122918148132,-0.428624436334322,
-0.542038039789524));
#34543=CARTESIAN_POINT('Ctrl Pts',(0.45803338769357,-0.0842204294398452,
-0.530254604141926));
#34544=CARTESIAN_POINT('Ctrl Pts',(0.322681437476349,0.335804042236243,
-0.518471168494327));
#34545=CARTESIAN_POINT('Ctrl Pts',(-0.10240211785065,0.454314286730666,
-0.506687732846729));
#34546=CARTESIAN_POINT('Ctrl Pts',(-0.435540099262727,0.164901445821025,
-0.49490429719913));
#34547=CARTESIAN_POINT('Ctrl Pts',(-0.377612102033148,-0.272574329827866,
-0.483120861551532));
#34548=CARTESIAN_POINT('Ctrl Pts',(0.0193690534496328,-0.465309042091788,
-0.471337425903934));
#34549=CARTESIAN_POINT('Ctrl Pts',(0.398958979401207,-0.24024861631879,
-0.459553990256335));
#34550=CARTESIAN_POINT('Ctrl Pts',(0.420328654298526,0.200528021136553,
-0.447770554608737));
#34551=CARTESIAN_POINT('Ctrl Pts',(0.064290515766074,0.461253069874142,
-0.435987118961139));
#34552=CARTESIAN_POINT('Ctrl Pts',(-0.349473268478174,0.307824787022427,
-0.42420368331354));
#34553=CARTESIAN_POINT('Ctrl Pts',(-0.449449399272338,-0.121995501472316,
-0.412420247665942));
#34554=CARTESIAN_POINT('Ctrl Pts',(-0.145870565889691,-0.442277563180907,
-0.400636812018343));
#34555=CARTESIAN_POINT('Ctrl Pts',(0.288683614412624,-0.36544416215812,
-0.388853376370746));
#34556=CARTESIAN_POINT('Ctrl Pts',(0.46403240727406,0.0395169569272912,
-0.377069940723147));
#34557=CARTESIAN_POINT('Ctrl Pts',(0.222732336443623,0.408996297281908,
-0.365286505075549));
#34558=CARTESIAN_POINT('Ctrl Pts',(-0.218556298620971,0.41124300506758,
-0.35350306942795));
#34559=CARTESIAN_POINT('Ctrl Pts',(-0.463605981299019,0.0442397896330434,
-0.341719633780352));
#34560=CARTESIAN_POINT('Ctrl Pts',(-0.292389682817799,-0.362485776660763,
-0.329936198132754));
#34561=CARTESIAN_POINT('Ctrl Pts',(0.14135963534951,-0.443739921983301,
-0.318152762485155));
#34562=CARTESIAN_POINT('Ctrl Pts',(0.448183914359544,-0.126565571082187,
-0.306369326837557));
#34563=CARTESIAN_POINT('Ctrl Pts',(0.352589492277338,0.304250414811037,
-0.294585891189958));
#34564=CARTESIAN_POINT('Ctrl Pts',(-0.0595906015999328,0.461883778605252,
-0.28280245554236));
#34565=CARTESIAN_POINT('Ctrl Pts',(-0.418265043254798,0.204797505982204,
-0.271019019894762));
#34566=CARTESIAN_POINT('Ctrl Pts',(-0.40138456254368,-0.236173873283955,
-0.259235584247163));
#34567=CARTESIAN_POINT('Ctrl Pts',(-0.024105928921317,-0.465087699171906,
-0.247452148599566));
#34568=CARTESIAN_POINT('Ctrl Pts',(0.374817112762246,-0.276405132309377,
-0.235668712951966));
#34569=CARTESIAN_POINT('Ctrl Pts',(0.437196586488692,0.160458135460469,
-0.223885277304369));
#34570=CARTESIAN_POINT('Ctrl Pts',(0.107022733782069,0.45324804543394,-0.21210184165677));
#34571=CARTESIAN_POINT('Ctrl Pts',(-0.319245469084403,0.339072264385629,
-0.200318406009172));
#34572=CARTESIAN_POINT('Ctrl Pts',(-0.458867211564245,-0.0795522962206605,
-0.188534970361574));
#34573=CARTESIAN_POINT('Ctrl Pts',(-0.186477793345172,-0.426747741630595,
-0.176751534713975));
#34574=CARTESIAN_POINT('Ctrl Pts',(0.253347573627205,-0.390771963537543,
-0.164968099066377));
#34575=CARTESIAN_POINT('Ctrl Pts',(0.465695563601222,-0.00392655608262027,
-0.153184663418778));
#34576=CARTESIAN_POINT('Ctrl Pts',(0.259900935227136,0.386443698320385,
-0.14140122777118));
#34577=CARTESIAN_POINT('Ctrl Pts',(-0.179254658034234,0.429832464241771,
-0.129617792123582));
#34578=CARTESIAN_POINT('Ctrl Pts',(-0.457461308535371,0.087277296570209,
-0.117834356475983));
#34579=CARTESIAN_POINT('Ctrl Pts',(-0.324916220195966,-0.333637768056457,
-0.106050920828385));
#34580=CARTESIAN_POINT('Ctrl Pts',(0.0993613588387723,-0.454993783974677,
-0.0942674851807868));
#34581=CARTESIAN_POINT('Ctrl Pts',(0.434434510205315,-0.167797288851672,
-0.0824840495331884));
#34582=CARTESIAN_POINT('Ctrl Pts',(0.379413574932619,0.270025378806949,
-0.07070061388559));
#34583=CARTESIAN_POINT('Ctrl Pts',(-0.0162382856254888,0.4654661714724,
-0.0589171782379918));
#34584=CARTESIAN_POINT('Ctrl Pts',(-0.397385996561566,0.242835949772861,
-0.0471337425903934));
#34585=CARTESIAN_POINT('Ctrl Pts',(-0.421580183389628,-0.197575591481363,
-0.035350306942795));
#34586=CARTESIAN_POINT('Ctrl Pts',(-0.0675247742952343,-0.461083753126696,
-0.0235668712951966));
#34587=CARTESIAN_POINT('Ctrl Pts',(0.347731504741513,-0.309602865163979,
-0.0117834356475983));
#34588=CARTESIAN_POINT('Ctrl Pts',(0.41551906970067,-0.0247650213838164,
-0.00392781188253288));
#34589=CARTESIAN_POINT('Ctrl Pts',(0.382276194676387,0.101025100760854,
-1.11022302462516E-16));
#34590=CARTESIAN_POINT('Ctrl Pts',(0.367076696441781,0.102274886126392,
-0.816560330221256));
#34591=CARTESIAN_POINT('Ctrl Pts',(0.333422572545675,0.223063528278077,
-0.812632518338723));
#34592=CARTESIAN_POINT('Ctrl Pts',(0.138265021670065,0.426865279663465,
-0.804776894573656));
#34593=CARTESIAN_POINT('Ctrl Pts',(-0.280819360295995,0.3504722762632,-0.792993458926061));
#34594=CARTESIAN_POINT('Ctrl Pts',(-0.446803312142898,-0.0411483102515571,
-0.78121002327846));
#34595=CARTESIAN_POINT('Ctrl Pts',(-0.212084922221472,-0.395546279128804,
-0.769426587630863));
#34596=CARTESIAN_POINT('Ctrl Pts',(0.21330867266151,-0.394931793547173,
-0.757643151983265));
#34597=CARTESIAN_POINT('Ctrl Pts',(0.447046217987789,-0.0396379759736438,
-0.745859716335665));
#34598=CARTESIAN_POINT('Ctrl Pts',(0.279453999895495,0.351207019666249,
-0.734076280688068));
#34599=CARTESIAN_POINT('Ctrl Pts',(-0.139091729468151,0.426728195662672,
-0.72229284504047));
#34600=CARTESIAN_POINT('Ctrl Pts',(-0.432730280663021,0.119084736933454,
-0.710509409392871));
#34601=CARTESIAN_POINT('Ctrl Pts',(-0.337835417043143,-0.295477781660029,
-0.698725973745272));
#34602=CARTESIAN_POINT('Ctrl Pts',(0.0604026768395285,-0.444737461000834,
-0.686942538097675));
#34603=CARTESIAN_POINT('Ctrl Pts',(0.404403319886607,-0.194671424698894,
-0.675159102450075));
#34604=CARTESIAN_POINT('Ctrl Pts',(0.385296692274669,0.230186829201976,
-0.663375666802478));
#34605=CARTESIAN_POINT('Ctrl Pts',(0.0202362844397346,0.44836364581947,
-0.651592231154879));
#34606=CARTESIAN_POINT('Ctrl Pts',(-0.362993649302062,0.26396016163497,
-0.639808795507281));
#34607=CARTESIAN_POINT('Ctrl Pts',(-0.420296348245201,-0.157449716953142,
-0.628025359859683));
#34608=CARTESIAN_POINT('Ctrl Pts',(-0.100220137021271,-0.437487535014054,
-0.616241924212084));
#34609=CARTESIAN_POINT('Ctrl Pts',(0.309842420659382,-0.324710764723573,
-0.604458488564485));
#34610=CARTESIAN_POINT('Ctrl Pts',(0.441701393293164,0.0796197016802426,
-0.592675052916888));
#34611=CARTESIAN_POINT('Ctrl Pts',(0.176962223994262,0.412460647770714,
-0.580891617269289));
#34612=CARTESIAN_POINT('Ctrl Pts',(-0.2466690932876,0.3749583600143,-0.569108181621692));
#34613=CARTESIAN_POINT('Ctrl Pts',(-0.448819337433567,0.000785677948102577,
-0.557324745974092));
#34614=CARTESIAN_POINT('Ctrl Pts',(-0.247980339868577,-0.374092455712532,
-0.545541310326495));
#34615=CARTESIAN_POINT('Ctrl Pts',(0.175517085612874,-0.413077676619869,
-0.533757874678895));
#34616=CARTESIAN_POINT('Ctrl Pts',(0.441419927479849,-0.0811656461177657,
-0.521974439031298));
#34617=CARTESIAN_POINT('Ctrl Pts',(0.310977366622007,0.323623997625541,
-0.510191003383699));
#34618=CARTESIAN_POINT('Ctrl Pts',(-0.0986878612998801,0.437835723093348,
-0.498407567736101));
#34619=CARTESIAN_POINT('Ctrl Pts',(-0.419742499557131,0.158920258241822,
-0.486624132088502));
#34620=CARTESIAN_POINT('Ctrl Pts',(-0.363915625309175,-0.262687708228774,
-0.474840696440904));
#34621=CARTESIAN_POINT('Ctrl Pts',(0.0186665129634842,-0.448431684533198,
-0.463057260793306));
#34622=CARTESIAN_POINT('Ctrl Pts',(0.384488223973171,-0.231534489934439,
-0.451273825145707));
#34623=CARTESIAN_POINT('Ctrl Pts',(0.405082793270711,0.193254611838459,
-0.439490389498109));
#34624=CARTESIAN_POINT('Ctrl Pts',(0.0619586160519983,0.444522827645736,
-0.427706953850511));
#34625=CARTESIAN_POINT('Ctrl Pts',(-0.336797423446752,0.296659585992549,
-0.415923518202913));
#34626=CARTESIAN_POINT('Ctrl Pts',(-0.43314729136162,-0.117570567691465,
-0.404140082555314));
#34627=CARTESIAN_POINT('Ctrl Pts',(-0.140579652808082,-0.426235586991514,
-0.392356646907716));
#34628=CARTESIAN_POINT('Ctrl Pts',(0.278212688337677,-0.352189032266994,
-0.380573211260117));
#34629=CARTESIAN_POINT('Ctrl Pts',(0.44720135490265,0.0380836260625165,
-0.36878977561252));
#34630=CARTESIAN_POINT('Ctrl Pts',(0.214653548064355,0.394161475421722,
-0.35700633996492));
#34631=CARTESIAN_POINT('Ctrl Pts',(-0.210628980505842,0.396326692225704,
-0.345222904317323));
#34632=CARTESIAN_POINT('Ctrl Pts',(-0.446790395946305,0.0426351555502902,
-0.333439468669723));
#34633=CARTESIAN_POINT('Ctrl Pts',(-0.281784332874083,-0.349337951217475,
-0.321656033022126));
#34634=CARTESIAN_POINT('Ctrl Pts',(0.136232339521731,-0.427644904158876,
-0.309872597374527));
#34635=CARTESIAN_POINT('Ctrl Pts',(0.431927707214611,-0.121974874997368,
-0.298089161726929));
#34636=CARTESIAN_POINT('Ctrl Pts',(0.339800617799819,0.293214860859558,
-0.28630572607933));
#34637=CARTESIAN_POINT('Ctrl Pts',(-0.0574291738189212,0.445130659759787,
-0.274522290431733));
#34638=CARTESIAN_POINT('Ctrl Pts',(-0.403094032054294,0.197369236976231,
-0.262738854784134));
#34639=CARTESIAN_POINT('Ctrl Pts',(-0.386825828094648,-0.227607543071477,
-0.250955419136536));
#34640=CARTESIAN_POINT('Ctrl Pts',(-0.0232315758680031,-0.44821837000577,
-0.239171983488938));
#34641=CARTESIAN_POINT('Ctrl Pts',(0.361222013894774,-0.266379562576102,
-0.227388547841339));
#34642=CARTESIAN_POINT('Ctrl Pts',(0.421338903860403,0.154638112464191,
-0.215605112193741));
#34643=CARTESIAN_POINT('Ctrl Pts',(0.103140881547223,0.436808155740133,
-0.203821676546142));
#34644=CARTESIAN_POINT('Ctrl Pts',(-0.307666025223877,0.326773677153128,
-0.192038240898544));
#34645=CARTESIAN_POINT('Ctrl Pts',(-0.442223507486053,-0.0766668320958137,
-0.180254805250946));
#34646=CARTESIAN_POINT('Ctrl Pts',(-0.179714003884139,-0.411269052047342,
-0.168471369603347));
#34647=CARTESIAN_POINT('Ctrl Pts',(0.244158331209982,-0.376598161707157,
-0.156687933955749));
#34648=CARTESIAN_POINT('Ctrl Pts',(0.44880418641024,-0.00378413484214192,
-0.144904498308151));
#34649=CARTESIAN_POINT('Ctrl Pts',(0.250473993954038,0.372426888237571,
-0.133121062660552));
#34650=CARTESIAN_POINT('Ctrl Pts',(-0.172752860983212,0.414241887801034,
-0.121337627012954));
#34651=CARTESIAN_POINT('Ctrl Pts',(-0.440868598368676,0.0841116367447717,
-0.109554191365355));
#34652=CARTESIAN_POINT('Ctrl Pts',(-0.313131090897422,-0.321536296997084,
-0.0977707557177573));
#34653=CARTESIAN_POINT('Ctrl Pts',(0.0957573945291805,-0.438490574098172,
-0.0859873200701589));
#34654=CARTESIAN_POINT('Ctrl Pts',(0.418677011637128,-0.161711065320358,
-0.0742038844225605));
#34655=CARTESIAN_POINT('Ctrl Pts',(0.365651756469058,0.260231210940511,
-0.062420448774962));
#34656=CARTESIAN_POINT('Ctrl Pts',(-0.0156493021159325,0.448583114629035,
-0.0506370131273639));
#34657=CARTESIAN_POINT('Ctrl Pts',(-0.382972295244705,0.234027977475628,
-0.0388535774797655));
#34658=CARTESIAN_POINT('Ctrl Pts',(-0.406288927791635,-0.190409270605048,
-0.0270701418321671));
#34659=CARTESIAN_POINT('Ctrl Pts',(-0.065075563863559,-0.44435965223454,
-0.0152867061845687));
#34660=CARTESIAN_POINT('Ctrl Pts',(0.33511883572153,-0.298373170952479,
-0.00350327053697042));
#34661=CARTESIAN_POINT('Ctrl Pts',(0.400447658493562,-0.0238667621989916,
0.00435235322809503));
#34662=CARTESIAN_POINT('Ctrl Pts',(0.368410545312071,0.09736079039141,0.00828016511062779));
#34663=CARTESIAN_POINT('Ctrl Pts',(0.353261248356923,0.0984256268479901,
-0.808280165110628));
#34664=CARTESIAN_POINT('Ctrl Pts',(0.320873744777592,0.214668218457478,
-0.804352353228095));
#34665=CARTESIAN_POINT('Ctrl Pts',(0.133061222988888,0.410799604104149,
-0.796496729463029));
#34666=CARTESIAN_POINT('Ctrl Pts',(-0.270250328453335,0.337281758900395,
-0.784713293815432));
#34667=CARTESIAN_POINT('Ctrl Pts',(-0.429987240670946,-0.0395996356841706,
-0.772929858167832));
#34668=CARTESIAN_POINT('Ctrl Pts',(-0.204102807690819,-0.380659338232164,
-0.761146422520236));
#34669=CARTESIAN_POINT('Ctrl Pts',(0.205280500560773,-0.380067979680208,
-0.749362986872634));
#34670=CARTESIAN_POINT('Ctrl Pts',(0.430221004412505,-0.03814614496241,
-0.73757955122504));
#34671=CARTESIAN_POINT('Ctrl Pts',(0.268936355313078,0.337988849201413,
-0.725796115577439));
#34672=CARTESIAN_POINT('Ctrl Pts',(-0.133856816475507,0.410667679452654,
-0.714012679929842));
#34673=CARTESIAN_POINT('Ctrl Pts',(-0.416443867536837,0.114602815262176,
-0.702229244282243));
#34674=CARTESIAN_POINT('Ctrl Pts',(-0.325120505661874,-0.284357059499448,
-0.690445808634644));
#34675=CARTESIAN_POINT('Ctrl Pts',(0.0581293370875048,-0.42799914074404,
-0.678662372987047));
#34676=CARTESIAN_POINT('Ctrl Pts',(0.389183031795877,-0.18734469165481,
-0.666878937339448));
#34677=CARTESIAN_POINT('Ctrl Pts',(0.370795509004288,0.221523423925956,
-0.655095501691849));
#34678=CARTESIAN_POINT('Ctrl Pts',(0.01947466339482,0.431488848993628,-0.643312066044252));
#34679=CARTESIAN_POINT('Ctrl Pts',(-0.349331872442684,0.254025649461116,
-0.631528630396653));
#34680=CARTESIAN_POINT('Ctrl Pts',(-0.404477903664755,-0.151523875264942,
-0.619745194749054));
#34681=CARTESIAN_POINT('Ctrl Pts',(-0.0964482111172401,-0.421022075925132,
-0.607961759101457));
#34682=CARTESIAN_POINT('Ctrl Pts',(0.298181065093639,-0.312489818103648,
-0.596178323453857));
#34683=CARTESIAN_POINT('Ctrl Pts',(0.425077339717431,0.0766231021527936,
-0.58439488780626));
#34684=CARTESIAN_POINT('Ctrl Pts',(0.170302001642169,0.396937110805389,
-0.57261145215866));
#34685=CARTESIAN_POINT('Ctrl Pts',(-0.237385354806005,0.360846274428439,
-0.560828016511064));
#34686=CARTESIAN_POINT('Ctrl Pts',(-0.431927390012499,0.000756107852782039,
-0.549044580863464));
#34687=CARTESIAN_POINT('Ctrl Pts',(-0.23864725077649,-0.360012959653721,
-0.537261145215866));
#34688=CARTESIAN_POINT('Ctrl Pts',(0.168911253077617,-0.397530916905416,
-0.525477709568268));
#34689=CARTESIAN_POINT('Ctrl Pts',(0.424806467266128,-0.0781108627956866,
-0.513694273920669));
#34690=CARTESIAN_POINT('Ctrl Pts',(0.299273295767665,0.31144395301484,-0.501910838273072));
#34691=CARTESIAN_POINT('Ctrl Pts',(-0.09497360474911,0.421357159456029,
-0.490127402625472));
#34692=CARTESIAN_POINT('Ctrl Pts',(-0.403944899851534,0.152939070662619,
-0.478343966977875));
#34693=CARTESIAN_POINT('Ctrl Pts',(-0.350219148585202,-0.252801086629681,
-0.466560531330277));
#34694=CARTESIAN_POINT('Ctrl Pts',(0.0179639724773354,-0.431554326974609,
-0.454777095682677));
#34695=CARTESIAN_POINT('Ctrl Pts',(0.370017468545135,-0.222820363550088,
-0.44299366003508));
#34696=CARTESIAN_POINT('Ctrl Pts',(0.389836932242896,0.185981202540365,
-0.431210224387481));
#34697=CARTESIAN_POINT('Ctrl Pts',(0.0596267163379231,0.427792585417331,
-0.419426788739883));
#34698=CARTESIAN_POINT('Ctrl Pts',(-0.32412157841533,0.285494384962672,
-0.407643353092284));
#34699=CARTESIAN_POINT('Ctrl Pts',(-0.416845183450903,-0.113145633910614,
-0.395859917444687));
#34700=CARTESIAN_POINT('Ctrl Pts',(-0.135288739726473,-0.410193610802121,
-0.384076481797087));
#34701=CARTESIAN_POINT('Ctrl Pts',(0.26774176226273,-0.338933902375868,
-0.37229304614949));
#34702=CARTESIAN_POINT('Ctrl Pts',(0.43037030253124,0.036650295197742,-0.360509610501891));
#34703=CARTESIAN_POINT('Ctrl Pts',(0.206574759685087,0.379326653561534,
-0.348726174854293));
#34704=CARTESIAN_POINT('Ctrl Pts',(-0.202701662390712,0.381410379383828,
-0.336942739206695));
#34705=CARTESIAN_POINT('Ctrl Pts',(-0.42997481059359,0.0410305214675364,
-0.325159303559096));
#34706=CARTESIAN_POINT('Ctrl Pts',(-0.271178982930367,-0.336190125774187,
-0.313375867911498));
#34707=CARTESIAN_POINT('Ctrl Pts',(0.131105043693952,-0.411549886334452,
-0.301592432263899));
#34708=CARTESIAN_POINT('Ctrl Pts',(0.415671500069678,-0.11738417891255,
-0.289808996616301));
#34709=CARTESIAN_POINT('Ctrl Pts',(0.3270117433223,0.28217930690808,-0.278025560968703));
#34710=CARTESIAN_POINT('Ctrl Pts',(-0.0552677460379093,0.428377540914321,
-0.266242125321104));
#34711=CARTESIAN_POINT('Ctrl Pts',(-0.387923020853791,0.189940967970258,
-0.254458689673507));
#34712=CARTESIAN_POINT('Ctrl Pts',(-0.372267093645615,-0.219041212858999,
-0.242675254025908));
#34713=CARTESIAN_POINT('Ctrl Pts',(-0.0223572228146897,-0.431349040839633,
-0.23089181837831));
#34714=CARTESIAN_POINT('Ctrl Pts',(0.347626915027303,-0.256353992842826,
-0.219108382730711));
#34715=CARTESIAN_POINT('Ctrl Pts',(0.405481221232114,0.148818089467912,
-0.207324947083113));
#34716=CARTESIAN_POINT('Ctrl Pts',(0.099259029312377,0.420368266046324,
-0.195541511435514));
#34717=CARTESIAN_POINT('Ctrl Pts',(-0.296086581363351,0.314475089920628,
-0.183758075787916));
#34718=CARTESIAN_POINT('Ctrl Pts',(-0.425579803407861,-0.073781367970967,
-0.171974640140318));
#34719=CARTESIAN_POINT('Ctrl Pts',(-0.172950214423107,-0.395790362464088,
-0.160191204492719));
#34720=CARTESIAN_POINT('Ctrl Pts',(0.234969088792759,-0.362424359876772,
-0.148407768845121));
#34721=CARTESIAN_POINT('Ctrl Pts',(0.431912809219259,-0.00364171360166344,
-0.136624333197522));
#34722=CARTESIAN_POINT('Ctrl Pts',(0.24104705268094,0.358410078154757,-0.124840897549924));
#34723=CARTESIAN_POINT('Ctrl Pts',(-0.16625106393219,0.398651311360297,
-0.113057461902326));
#34724=CARTESIAN_POINT('Ctrl Pts',(-0.424275888201981,0.0809459769193339,
-0.101274026254728));
#34725=CARTESIAN_POINT('Ctrl Pts',(-0.301345961598879,-0.309434825937711,
-0.0894905906071294));
#34726=CARTESIAN_POINT('Ctrl Pts',(0.092153430219589,-0.421987364221666,
-0.077707154959531));
#34727=CARTESIAN_POINT('Ctrl Pts',(0.402919513068942,-0.155624841789045,
-0.0659237193119326));
#34728=CARTESIAN_POINT('Ctrl Pts',(0.351889938005496,0.250437043074074,
-0.0541402836643342));
#34729=CARTESIAN_POINT('Ctrl Pts',(-0.0150603186063758,0.431700057785669,
-0.042356848016736));
#34730=CARTESIAN_POINT('Ctrl Pts',(-0.368558593927843,0.225220005178395,
-0.0305734123691377));
#34731=CARTESIAN_POINT('Ctrl Pts',(-0.390997672193642,-0.183242949728733,
-0.0187899767215392));
#34732=CARTESIAN_POINT('Ctrl Pts',(-0.0626263534318833,-0.427635551342383,
-0.00700654107394084));
#34733=CARTESIAN_POINT('Ctrl Pts',(0.322506166701548,-0.28714347674098,
0.00477689457365751));
#34734=CARTESIAN_POINT('Ctrl Pts',(0.385376247286455,-0.0229685030141659,
0.0126325183387229));
#34735=CARTESIAN_POINT('Ctrl Pts',(0.354544895947755,0.0936964800219656,
0.0165603302212557));
#34736=CARTESIAN_POINT('Ctrl Pts',(0.339445800272064,0.094576367569588,
-0.8));
#34737=CARTESIAN_POINT('Ctrl Pts',(0.308324917009509,0.206272908636879,
-0.796072188117467));
#34738=CARTESIAN_POINT('Ctrl Pts',(0.12785742430771,0.394733928544834,-0.788216564352402));
#34739=CARTESIAN_POINT('Ctrl Pts',(-0.259681296610673,0.32409124153759,
-0.776433128704804));
#34740=CARTESIAN_POINT('Ctrl Pts',(-0.413171169198995,-0.0380509611167842,
-0.764649693057206));
#34741=CARTESIAN_POINT('Ctrl Pts',(-0.196120693160165,-0.365772397335523,
-0.752866257409607));
#34742=CARTESIAN_POINT('Ctrl Pts',(0.197252328460035,-0.365204165813244,
-0.741082821762008));
#34743=CARTESIAN_POINT('Ctrl Pts',(0.413395790837222,-0.036654313951176,
-0.72929938611441));
#34744=CARTESIAN_POINT('Ctrl Pts',(0.258418710730661,0.324770678736576,
-0.717515950466812));
#34745=CARTESIAN_POINT('Ctrl Pts',(-0.128621903482862,0.394607163242637,
-0.705732514819214));
#34746=CARTESIAN_POINT('Ctrl Pts',(-0.400157454410652,0.110120893590899,
-0.693949079171615));
#34747=CARTESIAN_POINT('Ctrl Pts',(-0.312405594280605,-0.273236337338868,
-0.682165643524017));
#34748=CARTESIAN_POINT('Ctrl Pts',(0.055855997335481,-0.411260820487245,
-0.670382207876418));
#34749=CARTESIAN_POINT('Ctrl Pts',(0.373962743705146,-0.180017958610726,
-0.65859877222882));
#34750=CARTESIAN_POINT('Ctrl Pts',(0.356294325733907,0.212860018649936,
-0.646815336581221));
#34751=CARTESIAN_POINT('Ctrl Pts',(0.0187130423499051,0.414614052167785,
-0.635031900933623));
#34752=CARTESIAN_POINT('Ctrl Pts',(-0.335670095583304,0.244091137287262,
-0.623248465286025));
#34753=CARTESIAN_POINT('Ctrl Pts',(-0.388659459084311,-0.145598033576742,
-0.611465029638427));
#34754=CARTESIAN_POINT('Ctrl Pts',(-0.0926762852132086,-0.404556616836208,
-0.599681593990828));
#34755=CARTESIAN_POINT('Ctrl Pts',(0.286519709527895,-0.300268871483724,
-0.58789815834323));
#34756=CARTESIAN_POINT('Ctrl Pts',(0.408453286141698,0.0736265026253448,
-0.576114722695632));
#34757=CARTESIAN_POINT('Ctrl Pts',(0.163641779290076,0.381413573840065,
-0.564331287048033));
#34758=CARTESIAN_POINT('Ctrl Pts',(-0.228101616324409,0.34673418884258,
-0.552547851400434));
#34759=CARTESIAN_POINT('Ctrl Pts',(-0.415035442591431,0.000726537757461266,
-0.540764415752838));
#34760=CARTESIAN_POINT('Ctrl Pts',(-0.229314161684403,-0.34593346359491,
-0.528980980105238));
#34761=CARTESIAN_POINT('Ctrl Pts',(0.162305420542359,-0.381984157190963,
-0.517197544457641));
#34762=CARTESIAN_POINT('Ctrl Pts',(0.408193007052407,-0.0750560794736075,
-0.505414108810041));
#34763=CARTESIAN_POINT('Ctrl Pts',(0.287569224913323,0.299263908404139,
-0.493630673162444));
#34764=CARTESIAN_POINT('Ctrl Pts',(-0.09125934819834,0.40487859581871,-0.481847237514845));
#34765=CARTESIAN_POINT('Ctrl Pts',(-0.388147300145938,0.146957883083416,
-0.470063801867247));
#34766=CARTESIAN_POINT('Ctrl Pts',(-0.336522671861229,-0.242914465030589,
-0.458280366219648));
#34767=CARTESIAN_POINT('Ctrl Pts',(0.0172614319911864,-0.414676969416019,
-0.44649693057205));
#34768=CARTESIAN_POINT('Ctrl Pts',(0.355546713117099,-0.214106237165738,
-0.434713494924451));
#34769=CARTESIAN_POINT('Ctrl Pts',(0.37459107121508,0.178707793242271,-0.422930059276854));
#34770=CARTESIAN_POINT('Ctrl Pts',(0.0572948166238478,0.411062343188925,
-0.411146623629255));
#34771=CARTESIAN_POINT('Ctrl Pts',(-0.311445733383908,0.274329183932795,
-0.399363187981657));
#34772=CARTESIAN_POINT('Ctrl Pts',(-0.400543075540186,-0.108720700129763,
-0.387579752334058));
#34773=CARTESIAN_POINT('Ctrl Pts',(-0.129997826644863,-0.394151634612728,
-0.37579631668646));
#34774=CARTESIAN_POINT('Ctrl Pts',(0.257270836187783,-0.325678772484742,
-0.364012881038862));
#34775=CARTESIAN_POINT('Ctrl Pts',(0.41353925015983,0.0352169643329669,
-0.352229445391263));
#34776=CARTESIAN_POINT('Ctrl Pts',(0.198495971305819,0.364491831701348,
-0.340446009743665));
#34777=CARTESIAN_POINT('Ctrl Pts',(-0.194774344275583,0.366494066541952,
-0.328662574096066));
#34778=CARTESIAN_POINT('Ctrl Pts',(-0.413159225240875,0.0394258873847827,
-0.316879138448469));
#34779=CARTESIAN_POINT('Ctrl Pts',(-0.26057363298665,-0.323042300330899,
-0.30509570280087));
#34780=CARTESIAN_POINT('Ctrl Pts',(0.125977747866173,-0.395454868510028,
-0.293312267153272));
#34781=CARTESIAN_POINT('Ctrl Pts',(0.399415292924746,-0.112793482827731,
-0.281528831505673));
#34782=CARTESIAN_POINT('Ctrl Pts',(0.314222868844781,0.271143752956601,
-0.269745395858075));
#34783=CARTESIAN_POINT('Ctrl Pts',(-0.0531063182568973,0.411624422068856,
-0.257961960210477));
#34784=CARTESIAN_POINT('Ctrl Pts',(-0.372752009653287,0.182512698964285,
-0.246178524562878));
#34785=CARTESIAN_POINT('Ctrl Pts',(-0.357708359196582,-0.210474882646521,
-0.23439508891528));
#34786=CARTESIAN_POINT('Ctrl Pts',(-0.0214828697613762,-0.414479711673496,
-0.222611653267681));
#34787=CARTESIAN_POINT('Ctrl Pts',(0.334031816159831,-0.24632842310955,
-0.210828217620083));
#34788=CARTESIAN_POINT('Ctrl Pts',(0.389623538603825,0.142998066471633,
-0.199044781972485));
#34789=CARTESIAN_POINT('Ctrl Pts',(0.095377177077531,0.403928376352516,
-0.187261346324887));
#34790=CARTESIAN_POINT('Ctrl Pts',(-0.284507137502825,0.302176502688127,
-0.175477910677288));
#34791=CARTESIAN_POINT('Ctrl Pts',(-0.408936099329668,-0.0708959038461205,
-0.16369447502969));
#34792=CARTESIAN_POINT('Ctrl Pts',(-0.166186424962074,-0.380311672880833,
-0.151911039382091));
#34793=CARTESIAN_POINT('Ctrl Pts',(0.225779846375536,-0.348250558046386,
-0.140127603734493));
#34794=CARTESIAN_POINT('Ctrl Pts',(0.415021432028277,-0.00349929236118479,
-0.128344168086895));
#34795=CARTESIAN_POINT('Ctrl Pts',(0.231620111407843,0.344393268071943,
-0.116560732439296));
#34796=CARTESIAN_POINT('Ctrl Pts',(-0.159749266881169,0.383060734919559,
-0.104777296791698));
#34797=CARTESIAN_POINT('Ctrl Pts',(-0.407683178035285,0.0777803170938962,
-0.0929938611440997));
#34798=CARTESIAN_POINT('Ctrl Pts',(-0.289560832300336,-0.297333354878338,
-0.0812104254965016));
#34799=CARTESIAN_POINT('Ctrl Pts',(0.0885494659099983,-0.405484154345161,
-0.0694269898489031));
#34800=CARTESIAN_POINT('Ctrl Pts',(0.387162014500754,-0.149538618257732,
-0.0576435542013047));
#34801=CARTESIAN_POINT('Ctrl Pts',(0.338128119541936,0.240642875207636,
-0.0458601185537062));
#34802=CARTESIAN_POINT('Ctrl Pts',(-0.01447133509682,0.414817000942304,
-0.0340766829061081));
#34803=CARTESIAN_POINT('Ctrl Pts',(-0.354144892610982,0.216412032881162,
-0.0222932472585097));
#34804=CARTESIAN_POINT('Ctrl Pts',(-0.375706416595649,-0.176076628852418,
-0.0105098116109113));
#34805=CARTESIAN_POINT('Ctrl Pts',(-0.0601771430002081,-0.410911450450226,
0.00127362403668707));
#34806=CARTESIAN_POINT('Ctrl Pts',(0.309893497681566,-0.27591378252948,
0.0130570596842854));
#34807=CARTESIAN_POINT('Ctrl Pts',(0.370304836079347,-0.0220702438293411,
0.0209126834493508));
#34808=CARTESIAN_POINT('Ctrl Pts',(0.340679246583439,0.0900321696525211,
0.0248404953318836));
#34809=CARTESIAN_POINT('',(0.382276194676387,0.101025100760854,-1.11022302462516E-16));
#34810=CARTESIAN_POINT('Ctrl Pts',(-0.0877607245812972,-0.341761560210009,
-9.71445146547012E-17));
#34811=CARTESIAN_POINT('Ctrl Pts',(-0.0758129511624255,-0.345685911786213,
-1.177492375083E-16));
#34812=CARTESIAN_POINT('Ctrl Pts',(-0.0636801234265344,-0.348930529057438,
-1.71071818152792E-16));
#34813=CARTESIAN_POINT('Ctrl Pts',(-0.0514067357749123,-0.351459262350156,
-7.97972798949331E-17));
#34814=CARTESIAN_POINT('Ctrl Pts',(-0.0333136723076778,-0.355187045848529,
5.12874859358975E-17));
#34815=CARTESIAN_POINT('Ctrl Pts',(-0.0149152850678594,-0.357361071442325,
-9.16194412763928E-17));
#34816=CARTESIAN_POINT('Ctrl Pts',(0.0036226861155836,-0.358060875566304,
-2.67147415300428E-16));
#34817=CARTESIAN_POINT('Ctrl Pts',(0.00988803044492662,-0.35829739086544,
-3.26471231580539E-16));
#34818=CARTESIAN_POINT('Ctrl Pts',(0.0161593613325987,-0.358364790839047,
2.4941399093868E-17));
#34819=CARTESIAN_POINT('Ctrl Pts',(0.0224287212483521,-0.35826689462958,
2.42861286636753E-17));
#34820=CARTESIAN_POINT('Ctrl Pts',(0.0394302907234294,-0.358001414703562,
2.25091329426463E-17));
#34821=CARTESIAN_POINT('Ctrl Pts',(0.056420623703811,-0.356522253769826,
-2.5213610675368E-16));
#34822=CARTESIAN_POINT('Ctrl Pts',(0.0732737027369599,-0.353889163118092,
-2.70616862252382E-16));
#34823=CARTESIAN_POINT('Ctrl Pts',(0.080079917994765,-0.352825773945481,
-2.7808042424029E-16));
#34824=CARTESIAN_POINT('Ctrl Pts',(0.0868637834211038,-0.351573895775077,
1.10500851824191E-16));
#34825=CARTESIAN_POINT('Ctrl Pts',(0.093617012145756,-0.3501363439148,1.31838984174237E-16));
#34826=CARTESIAN_POINT('Ctrl Pts',(0.0991248085493264,-0.348963905768721,
1.49241932217071E-16));
#34827=CARTESIAN_POINT('Ctrl Pts',(0.104611759658228,-0.347667843483011,
-2.60939886659057E-16));
#34828=CARTESIAN_POINT('Ctrl Pts',(0.110060136668145,-0.346253488087783,
-2.70616862252382E-16));
#34829=CARTESIAN_POINT('Ctrl Pts',(0.130533905168791,-0.340938660408493,
-3.06980747813803E-16));
#34830=CARTESIAN_POINT('Ctrl Pts',(0.150511485695683,-0.333947922137602,
-1.0781477527908E-16));
#34831=CARTESIAN_POINT('Ctrl Pts',(0.169762335881931,-0.325386261459349,
-2.77555756156289E-17));
#34832=CARTESIAN_POINT('Ctrl Pts',(0.18344782334648,-0.319299751058283,
2.91587509110359E-17));
#34833=CARTESIAN_POINT('Ctrl Pts',(0.196766296793287,-0.312418138560091,
1.39805396323208E-17));
#34834=CARTESIAN_POINT('Ctrl Pts',(0.209631272392485,-0.304763602083614,
3.81639164714898E-17));
#34835=CARTESIAN_POINT('Ctrl Pts',(0.215617622250039,-0.301201781620584,
4.9416961872163E-17));
#34836=CARTESIAN_POINT('Ctrl Pts',(0.221505701159809,-0.29747243078369,
7.35255697550562E-18));
#34837=CARTESIAN_POINT('Ctrl Pts',(0.227286255175715,-0.29357690861442,
1.04083408558608E-17));
#34838=CARTESIAN_POINT('Ctrl Pts',(0.231373893127996,-0.290822244577161,
1.25691957028073E-17));
#34839=CARTESIAN_POINT('Ctrl Pts',(0.235404366734835,-0.287986626798667,
-6.88599098182481E-17));
#34840=CARTESIAN_POINT('Ctrl Pts',(0.239368194670903,-0.285075849963472,
-7.11236625150491E-17));
#34841=CARTESIAN_POINT('Ctrl Pts',(0.253900448925098,-0.274404309793586,
-7.94230716440859E-17));
#34842=CARTESIAN_POINT('Ctrl Pts',(0.267564666409036,-0.262706457293931,
1.34449454094602E-16));
#34843=CARTESIAN_POINT('Ctrl Pts',(0.280217681766689,-0.250031803400258,
7.45931094670027E-17));
#34844=CARTESIAN_POINT('Ctrl Pts',(0.291337752368455,-0.238892715825742,
2.51264174834658E-17));
#34845=CARTESIAN_POINT('Ctrl Pts',(0.301677019629086,-0.226998713289539,
-1.40107180888897E-16));
#34846=CARTESIAN_POINT('Ctrl Pts',(0.311222774198572,-0.214447092320648,
-1.78676518025611E-16));
#34847=CARTESIAN_POINT('Ctrl Pts',(0.315932140355436,-0.208254792008042,
-1.97704571772661E-16));
#34848=CARTESIAN_POINT('Ctrl Pts',(0.320448187331642,-0.201902232686996,
-1.19650750174349E-16));
#34849=CARTESIAN_POINT('Ctrl Pts',(0.324768233576707,-0.195400111602237,
-1.37043154602168E-16));
#34850=CARTESIAN_POINT('Ctrl Pts',(0.328357743214907,-0.189997524458835,
-1.51494435857885E-16));
#34851=CARTESIAN_POINT('Ctrl Pts',(0.331813146917509,-0.184489067659585,
-9.43126563239188E-17));
#34852=CARTESIAN_POINT('Ctrl Pts',(0.335120725151517,-0.178902066827157,
-7.63278329429795E-17));
#34853=CARTESIAN_POINT('Ctrl Pts',(0.345962373971419,-0.160588879142313,
-1.73768043084045E-17));
#34854=CARTESIAN_POINT('Ctrl Pts',(0.355249503471015,-0.141391317035762,
-5.63017718245087E-17));
#34855=CARTESIAN_POINT('Ctrl Pts',(0.362958797935917,-0.121547298462339,
8.67361737988404E-19));
#34856=CARTESIAN_POINT('Ctrl Pts',(0.369776633578432,-0.103997928966007,
5.14257829046096E-17));
#34857=CARTESIAN_POINT('Ctrl Pts',(0.375360154194583,-0.0859417157175588,
-5.76413480178255E-17));
#34858=CARTESIAN_POINT('Ctrl Pts',(0.379665889922516,-0.0675259946344044,
-9.4542429440736E-17));
#34859=CARTESIAN_POINT('Ctrl Pts',(0.380989312850641,-0.0618656873003285,
-1.05884448624796E-16));
#34860=CARTESIAN_POINT('Ctrl Pts',(0.382191821778051,-0.0561713465087971,
-2.82818896685015E-16));
#34861=CARTESIAN_POINT('Ctrl Pts',(0.383271604327089,-0.0504471153025764,
-3.25260651745651E-16));
#34862=CARTESIAN_POINT('Ctrl Pts',(0.384221568788495,-0.0454110863172686,
-3.62599798431484E-16));
#34863=CARTESIAN_POINT('Ctrl Pts',(0.385074753570206,-0.0403613371122496,
2.29496281791598E-18));
#34864=CARTESIAN_POINT('Ctrl Pts',(0.385830757252302,-0.0353015274382432,
4.33680868994202E-18));
#34865=CARTESIAN_POINT('Ctrl Pts',(0.389216753731649,-0.0126396037623478,
1.34818473951543E-17));
#34866=CARTESIAN_POINT('Ctrl Pts',(0.390658467045214,0.0102261533125763,
-1.65967614351841E-16));
#34867=CARTESIAN_POINT('Ctrl Pts',(0.390095953236443,0.0330330050049388,
-2.19008838842072E-16));
#34868=CARTESIAN_POINT('Ctrl Pts',(0.389567451361758,0.0544608591964589,
-2.68842969385262E-16));
#34869=CARTESIAN_POINT('Ctrl Pts',(0.387269745794741,0.0758382323114046,
-4.68604663216744E-18));
#34870=CARTESIAN_POINT('Ctrl Pts',(0.38310379834931,0.0969520739608447,
1.7130394325271E-17));
#34871=CARTESIAN_POINT('Ctrl Pts',(0.38283569725694,0.0983108630681218,
1.8534399471502E-17));
#34872=CARTESIAN_POINT('Ctrl Pts',(0.382559840678217,0.0996685580786185,
-1.11708830315621E-16));
#34873=CARTESIAN_POINT('Ctrl Pts',(0.382276194676387,0.101025100760854,
-1.12757025938492E-16));
#34874=CARTESIAN_POINT('Ctrl Pts',(0.382276194676389,0.101025100760849,
-2.50371428041207E-16));
#34875=CARTESIAN_POINT('Ctrl Pts',(0.415519069700669,-0.0247650213838198,
-0.00392781188253294));
#34876=CARTESIAN_POINT('Ctrl Pts',(0.381625287221089,-0.1671839432739,-0.00785562376506566));
#34877=CARTESIAN_POINT('Ctrl Pts',(0.295469016141844,-0.263640218879391,
-0.0117834356475983));
#34878=CARTESIAN_POINT('Ctrl Pts',(0.209312745062596,-0.360096494484885,
-0.0157112475301311));
#34879=CARTESIAN_POINT('Ctrl Pts',(0.0708939853836822,-0.41059012380579,
-0.0196390594126638));
#34880=CARTESIAN_POINT('Ctrl Pts',(-0.0573246293048418,-0.391918911525354,
-0.0235668712951966));
#34881=CARTESIAN_POINT('Ctrl Pts',(-0.185543243993364,-0.373247699244919,
-0.0274946831777294));
#34882=CARTESIAN_POINT('Ctrl Pts',(-0.303561713691496,-0.285411645363141,
-0.0314224950602622));
#34883=CARTESIAN_POINT('Ctrl Pts',(-0.358538584069218,-0.168091694879883,
-0.0353503069427949));
#34884=CARTESIAN_POINT('Ctrl Pts',(-0.382957007318537,-0.115983086535923,
-0.0370948764741711));
#34885=CARTESIAN_POINT('Ctrl Pts',(-0.394938808705564,-0.058058000231184,
-0.0388394460055472));
#34886=CARTESIAN_POINT('Ctrl Pts',(-0.394794988713166,-8.02750947288822E-5,
-0.0405840155369234));
#34887=CARTESIAN_POINT('Origin',(-0.5,0.5,0.1));
#34888=CARTESIAN_POINT('',(-0.58,0.5,0.));
#34889=CARTESIAN_POINT('Origin',(-0.5,0.5,0.));
#34890=CARTESIAN_POINT('',(-0.58,0.5,0.2));
#34891=CARTESIAN_POINT('',(-0.58,0.5,0.1));
#34892=CARTESIAN_POINT('Origin',(-0.5,0.5,0.2));
#34893=CARTESIAN_POINT('Origin',(0.5,0.5,0.1));
#34894=CARTESIAN_POINT('',(0.42,0.5,0.));
#34895=CARTESIAN_POINT('Origin',(0.5,0.5,0.));
#34896=CARTESIAN_POINT('',(0.42,0.5,0.2));
#34897=CARTESIAN_POINT('',(0.42,0.5,0.1));
#34898=CARTESIAN_POINT('Origin',(0.5,0.5,0.2));
#34899=CARTESIAN_POINT('Origin',(0.5,-0.5,0.1));
#34900=CARTESIAN_POINT('',(0.42,-0.5,0.));
#34901=CARTESIAN_POINT('Origin',(0.5,-0.5,0.));
#34902=CARTESIAN_POINT('',(0.42,-0.5,0.2));
#34903=CARTESIAN_POINT('',(0.42,-0.5,0.1));
#34904=CARTESIAN_POINT('Origin',(0.5,-0.5,0.2));
#34905=CARTESIAN_POINT('Origin',(-0.5,-0.5,0.1));
#34906=CARTESIAN_POINT('',(-0.58,-0.5,0.));
#34907=CARTESIAN_POINT('Origin',(-0.5,-0.5,0.));
#34908=CARTESIAN_POINT('',(-0.58,-0.5,0.2));
#34909=CARTESIAN_POINT('',(-0.58,-0.5,0.1));
#34910=CARTESIAN_POINT('Origin',(-0.5,-0.5,0.2));
#34911=CARTESIAN_POINT('Origin',(0.463644396618753,-0.12423314164921,0.66));
#34912=CARTESIAN_POINT('',(0.479742226065207,-0.140880788363777,0.66));
#34913=CARTESIAN_POINT('',(0.479742226065207,-0.140880788363777,1.34));
#34914=CARTESIAN_POINT('',(0.479742226065207,-0.140880788363777,1.));
#34915=CARTESIAN_POINT('',(0.463644396618753,-0.12423314164921,0.66));
#34916=CARTESIAN_POINT('',(0.463644396618753,-0.12423314164921,0.66));
#34917=CARTESIAN_POINT('',(0.463644396618753,-0.12423314164921,1.34));
#34918=CARTESIAN_POINT('',(0.463644396618753,-0.12423314164921,0.66));
#34919=CARTESIAN_POINT('',(0.463644396618753,-0.12423314164921,1.34));
#34920=CARTESIAN_POINT('Origin',(0.492622171407425,-0.131997713002286,1.34));
#34921=CARTESIAN_POINT('',(0.485909349222455,-0.117864771404394,1.34));
#34922=CARTESIAN_POINT('Origin',(0.,0.,1.34));
#34923=CARTESIAN_POINT('',(0.530916762985404,-0.104991450732855,1.34));
#34924=CARTESIAN_POINT('Origin',(0.530916762985404,-0.104991450732855,0.66));
#34925=CARTESIAN_POINT('',(0.485909349222455,-0.117864771404394,0.66));
#34926=CARTESIAN_POINT('',(0.485909349222455,-0.117864771404394,1.));
#34927=CARTESIAN_POINT('',(0.530916762985404,-0.104991450732855,0.66));
#34928=CARTESIAN_POINT('Origin',(0.492622171407425,-0.131997713002286,0.66));
#34929=CARTESIAN_POINT('Origin',(0.,0.,0.66));
#34930=CARTESIAN_POINT('Origin',(0.41569219381653,-0.24,0.66));
#34931=CARTESIAN_POINT('',(0.42693277500019,-0.260246816754091,0.66));
#34932=CARTESIAN_POINT('',(0.42693277500019,-0.260246816754091,1.34));
#34933=CARTESIAN_POINT('',(0.42693277500019,-0.260246816754091,1.));
#34934=CARTESIAN_POINT('',(0.41569219381653,-0.24,0.66));
#34935=CARTESIAN_POINT('',(0.41569219381653,-0.24,0.66));
#34936=CARTESIAN_POINT('',(0.41569219381653,-0.24,1.34));
#34937=CARTESIAN_POINT('',(0.41569219381653,-0.24,0.66));
#34938=CARTESIAN_POINT('',(0.41569219381653,-0.24,1.34));
#34939=CARTESIAN_POINT('Origin',(0.441672955930064,-0.255,1.34));
#34940=CARTESIAN_POINT('',(0.438846742063171,-0.239611220481305,1.34));
#34941=CARTESIAN_POINT('Origin',(0.,0.,1.34));
#34942=CARTESIAN_POINT('',(0.485652425954788,-0.238825323427225,1.34));
#34943=CARTESIAN_POINT('Origin',(0.485652425954788,-0.238825323427225,0.66));
#34944=CARTESIAN_POINT('',(0.438846742063171,-0.239611220481305,0.66));
#34945=CARTESIAN_POINT('',(0.438846742063171,-0.239611220481305,1.));
#34946=CARTESIAN_POINT('',(0.485652425954788,-0.238825323427225,0.66));
#34947=CARTESIAN_POINT('Origin',(0.441672955930064,-0.255,0.66));
#34948=CARTESIAN_POINT('Origin',(0.,0.,0.66));
#34949=CARTESIAN_POINT('Origin',(0.339411254969543,-0.339411254969543,0.66));
#34950=CARTESIAN_POINT('',(0.345028560858678,-0.361877454660814,0.66));
#34951=CARTESIAN_POINT('',(0.345028560858678,-0.361877454660814,1.34));
#34952=CARTESIAN_POINT('',(0.345028560858678,-0.361877454660814,1.));
#34953=CARTESIAN_POINT('',(0.339411254969543,-0.339411254969543,0.66));
#34954=CARTESIAN_POINT('',(0.339411254969543,-0.339411254969543,0.66));
#34955=CARTESIAN_POINT('',(0.339411254969543,-0.339411254969543,1.34));
#34956=CARTESIAN_POINT('',(0.339411254969543,-0.339411254969543,0.66));
#34957=CARTESIAN_POINT('',(0.339411254969543,-0.339411254969543,1.34));
#34958=CARTESIAN_POINT('Origin',(0.360624458405139,-0.360624458405139,1.34));
#34959=CARTESIAN_POINT('',(0.361877454660813,-0.345028560858679,1.34));
#34960=CARTESIAN_POINT('Origin',(0.,0.,1.34));
#34961=CARTESIAN_POINT('',(0.407291678673935,-0.356383645007537,1.34));
#34962=CARTESIAN_POINT('Origin',(0.407291678673935,-0.356383645007537,0.66));
#34963=CARTESIAN_POINT('',(0.361877454660813,-0.345028560858679,0.66));
#34964=CARTESIAN_POINT('',(0.361877454660813,-0.345028560858679,1.));
#34965=CARTESIAN_POINT('',(0.407291678673935,-0.356383645007537,0.66));
#34966=CARTESIAN_POINT('Origin',(0.360624458405139,-0.360624458405139,0.66));
#34967=CARTESIAN_POINT('Origin',(0.,0.,0.66));
#34968=CARTESIAN_POINT('Origin',(0.24,-0.415692193816531,0.66));
#34969=CARTESIAN_POINT('',(0.239611220481304,-0.438846742063172,0.66));
#34970=CARTESIAN_POINT('',(0.239611220481304,-0.438846742063172,1.34));
#34971=CARTESIAN_POINT('',(0.239611220481304,-0.438846742063172,1.));
#34972=CARTESIAN_POINT('',(0.24,-0.415692193816531,0.66));
#34973=CARTESIAN_POINT('',(0.24,-0.415692193816531,0.66));
#34974=CARTESIAN_POINT('',(0.24,-0.415692193816531,1.34));
#34975=CARTESIAN_POINT('',(0.24,-0.415692193816531,0.66));
#34976=CARTESIAN_POINT('',(0.24,-0.415692193816531,1.34));
#34977=CARTESIAN_POINT('Origin',(0.255,-0.441672955930064,1.34));
#34978=CARTESIAN_POINT('',(0.260246816754091,-0.42693277500019,1.34));
#34979=CARTESIAN_POINT('Origin',(0.,0.,1.34));
#34980=CARTESIAN_POINT('',(0.301174676572775,-0.449655010132406,1.34));
#34981=CARTESIAN_POINT('Origin',(0.301174676572775,-0.449655010132406,0.66));
#34982=CARTESIAN_POINT('',(0.260246816754091,-0.42693277500019,0.66));
#34983=CARTESIAN_POINT('',(0.260246816754091,-0.42693277500019,1.));
#34984=CARTESIAN_POINT('',(0.301174676572775,-0.449655010132406,0.66));
#34985=CARTESIAN_POINT('Origin',(0.255,-0.441672955930064,0.66));
#34986=CARTESIAN_POINT('Origin',(0.,0.,0.66));
#34987=CARTESIAN_POINT('Origin',(0.12423314164921,-0.463644396618753,0.66));
#34988=CARTESIAN_POINT('',(0.117864771404394,-0.485909349222455,0.66));
#34989=CARTESIAN_POINT('',(0.117864771404394,-0.485909349222455,1.34));
#34990=CARTESIAN_POINT('',(0.117864771404394,-0.485909349222455,1.));
#34991=CARTESIAN_POINT('',(0.12423314164921,-0.463644396618753,0.66));
#34992=CARTESIAN_POINT('',(0.12423314164921,-0.463644396618753,0.66));
#34993=CARTESIAN_POINT('',(0.12423314164921,-0.463644396618753,1.34));
#34994=CARTESIAN_POINT('',(0.12423314164921,-0.463644396618753,0.66));
#34995=CARTESIAN_POINT('',(0.12423314164921,-0.463644396618753,1.34));
#34996=CARTESIAN_POINT('Origin',(0.131997713002285,-0.492622171407425,1.34));
#34997=CARTESIAN_POINT('',(0.140880788363777,-0.479742226065208,1.34));
#34998=CARTESIAN_POINT('Origin',(0.,0.,1.34));
#34999=CARTESIAN_POINT('',(0.174533117977867,-0.512283129406789,1.34));
#35000=CARTESIAN_POINT('Origin',(0.174533117977867,-0.512283129406789,0.66));
#35001=CARTESIAN_POINT('',(0.140880788363777,-0.479742226065208,0.66));
#35002=CARTESIAN_POINT('',(0.140880788363777,-0.479742226065208,1.));
#35003=CARTESIAN_POINT('',(0.174533117977867,-0.512283129406789,0.66));
#35004=CARTESIAN_POINT('Origin',(0.131997713002285,-0.492622171407425,0.66));
#35005=CARTESIAN_POINT('Origin',(0.,0.,0.66));
#35006=CARTESIAN_POINT('Origin',(-6.93889390390723E-17,-0.48,0.66));
#35007=CARTESIAN_POINT('',(-0.0119139670629818,-0.499858037235396,0.66));
#35008=CARTESIAN_POINT('',(-0.0119139670629818,-0.499858037235396,1.34));
#35009=CARTESIAN_POINT('',(-0.0119139670629818,-0.499858037235396,1.));
#35010=CARTESIAN_POINT('',(-6.93889390390723E-17,-0.48,0.66));
#35011=CARTESIAN_POINT('',(-6.93889390390723E-17,-0.48,0.66));
#35012=CARTESIAN_POINT('',(-6.93889390390723E-17,-0.48,1.34));
#35013=CARTESIAN_POINT('',(-6.93889390390723E-17,-0.48,0.66));
#35014=CARTESIAN_POINT('',(-6.93889390390723E-17,-0.48,1.34));
#35015=CARTESIAN_POINT('Origin',(-8.32667268468867E-17,-0.51,1.34));
#35016=CARTESIAN_POINT('',(0.0119139670629816,-0.499858037235396,1.34));
#35017=CARTESIAN_POINT('Origin',(0.,0.,1.34));
#35018=CARTESIAN_POINT('',(0.0359974158223829,-0.54,1.34));
#35019=CARTESIAN_POINT('Origin',(0.0359974158223829,-0.54,0.66));
#35020=CARTESIAN_POINT('',(0.0119139670629816,-0.499858037235396,0.66));
#35021=CARTESIAN_POINT('',(0.0119139670629816,-0.499858037235396,1.));
#35022=CARTESIAN_POINT('',(0.0359974158223829,-0.54,0.66));
#35023=CARTESIAN_POINT('Origin',(-8.32667268468867E-17,-0.51,0.66));
#35024=CARTESIAN_POINT('Origin',(0.,0.,0.66));
#35025=CARTESIAN_POINT('Origin',(-0.12423314164921,-0.463644396618753,0.66));
#35026=CARTESIAN_POINT('',(-0.140880788363777,-0.479742226065207,0.66));
#35027=CARTESIAN_POINT('',(-0.140880788363777,-0.479742226065207,1.34));
#35028=CARTESIAN_POINT('',(-0.140880788363777,-0.479742226065207,1.));
#35029=CARTESIAN_POINT('',(-0.12423314164921,-0.463644396618753,0.66));
#35030=CARTESIAN_POINT('',(-0.12423314164921,-0.463644396618753,0.66));
#35031=CARTESIAN_POINT('',(-0.12423314164921,-0.463644396618753,1.34));
#35032=CARTESIAN_POINT('',(-0.12423314164921,-0.463644396618753,0.66));
#35033=CARTESIAN_POINT('',(-0.12423314164921,-0.463644396618753,1.34));
#35034=CARTESIAN_POINT('Origin',(-0.131997713002286,-0.492622171407425,
1.34));
#35035=CARTESIAN_POINT('',(-0.117864771404394,-0.485909349222455,1.34));
#35036=CARTESIAN_POINT('Origin',(0.,0.,1.34));
#35037=CARTESIAN_POINT('',(-0.104991450732855,-0.530916762985404,1.34));
#35038=CARTESIAN_POINT('Origin',(-0.104991450732855,-0.530916762985404,
0.66));
#35039=CARTESIAN_POINT('',(-0.117864771404394,-0.485909349222455,0.66));
#35040=CARTESIAN_POINT('',(-0.117864771404394,-0.485909349222455,1.));
#35041=CARTESIAN_POINT('',(-0.104991450732855,-0.530916762985404,0.66));
#35042=CARTESIAN_POINT('Origin',(-0.131997713002286,-0.492622171407425,
0.66));
#35043=CARTESIAN_POINT('Origin',(0.,0.,0.66));
#35044=CARTESIAN_POINT('Origin',(-0.24,-0.41569219381653,0.66));
#35045=CARTESIAN_POINT('',(-0.260246816754091,-0.42693277500019,0.66));
#35046=CARTESIAN_POINT('',(-0.260246816754091,-0.42693277500019,1.34));
#35047=CARTESIAN_POINT('',(-0.260246816754091,-0.42693277500019,1.));
#35048=CARTESIAN_POINT('',(-0.24,-0.41569219381653,0.66));
#35049=CARTESIAN_POINT('',(-0.24,-0.41569219381653,0.66));
#35050=CARTESIAN_POINT('',(-0.24,-0.41569219381653,1.34));
#35051=CARTESIAN_POINT('',(-0.24,-0.41569219381653,0.66));
#35052=CARTESIAN_POINT('',(-0.24,-0.41569219381653,1.34));
#35053=CARTESIAN_POINT('Origin',(-0.255,-0.441672955930064,1.34));
#35054=CARTESIAN_POINT('',(-0.239611220481305,-0.438846742063171,1.34));
#35055=CARTESIAN_POINT('Origin',(0.,0.,1.34));
#35056=CARTESIAN_POINT('',(-0.238825323427225,-0.485652425954788,1.34));
#35057=CARTESIAN_POINT('Origin',(-0.238825323427225,-0.485652425954788,
0.66));
#35058=CARTESIAN_POINT('',(-0.239611220481305,-0.438846742063171,0.66));
#35059=CARTESIAN_POINT('',(-0.239611220481305,-0.438846742063171,1.));
#35060=CARTESIAN_POINT('',(-0.238825323427225,-0.485652425954788,0.66));
#35061=CARTESIAN_POINT('Origin',(-0.255,-0.441672955930064,0.66));
#35062=CARTESIAN_POINT('Origin',(0.,0.,0.66));
#35063=CARTESIAN_POINT('Origin',(-0.339411254969543,-0.339411254969543,
0.66));
#35064=CARTESIAN_POINT('',(-0.361877454660814,-0.345028560858678,0.66));
#35065=CARTESIAN_POINT('',(-0.361877454660814,-0.345028560858678,1.34));
#35066=CARTESIAN_POINT('',(-0.361877454660814,-0.345028560858678,1.));
#35067=CARTESIAN_POINT('',(-0.339411254969543,-0.339411254969543,0.66));
#35068=CARTESIAN_POINT('',(-0.339411254969543,-0.339411254969543,0.66));
#35069=CARTESIAN_POINT('',(-0.339411254969543,-0.339411254969543,1.34));
#35070=CARTESIAN_POINT('',(-0.339411254969543,-0.339411254969543,0.66));
#35071=CARTESIAN_POINT('',(-0.339411254969543,-0.339411254969543,1.34));
#35072=CARTESIAN_POINT('Origin',(-0.360624458405139,-0.360624458405139,
1.34));
#35073=CARTESIAN_POINT('',(-0.345028560858679,-0.361877454660813,1.34));
#35074=CARTESIAN_POINT('Origin',(0.,0.,1.34));
#35075=CARTESIAN_POINT('',(-0.356383645007537,-0.407291678673934,1.34));
#35076=CARTESIAN_POINT('Origin',(-0.356383645007537,-0.407291678673934,
0.66));
#35077=CARTESIAN_POINT('',(-0.345028560858679,-0.361877454660813,0.66));
#35078=CARTESIAN_POINT('',(-0.345028560858679,-0.361877454660813,1.));
#35079=CARTESIAN_POINT('',(-0.356383645007537,-0.407291678673934,0.66));
#35080=CARTESIAN_POINT('Origin',(-0.360624458405139,-0.360624458405139,
0.66));
#35081=CARTESIAN_POINT('Origin',(0.,0.,0.66));
#35082=CARTESIAN_POINT('Origin',(-0.415692193816531,-0.24,0.66));
#35083=CARTESIAN_POINT('',(-0.438846742063171,-0.239611220481304,0.66));
#35084=CARTESIAN_POINT('',(-0.438846742063171,-0.239611220481304,1.34));
#35085=CARTESIAN_POINT('',(-0.438846742063171,-0.239611220481304,1.));
#35086=CARTESIAN_POINT('',(-0.415692193816531,-0.24,0.66));
#35087=CARTESIAN_POINT('',(-0.415692193816531,-0.24,0.66));
#35088=CARTESIAN_POINT('',(-0.415692193816531,-0.24,1.34));
#35089=CARTESIAN_POINT('',(-0.415692193816531,-0.24,0.66));
#35090=CARTESIAN_POINT('',(-0.415692193816531,-0.24,1.34));
#35091=CARTESIAN_POINT('Origin',(-0.441672955930064,-0.255,1.34));
#35092=CARTESIAN_POINT('',(-0.42693277500019,-0.260246816754091,1.34));
#35093=CARTESIAN_POINT('Origin',(0.,0.,1.34));
#35094=CARTESIAN_POINT('',(-0.449655010132406,-0.301174676572776,1.34));
#35095=CARTESIAN_POINT('Origin',(-0.449655010132406,-0.301174676572776,
0.66));
#35096=CARTESIAN_POINT('',(-0.42693277500019,-0.260246816754091,0.66));
#35097=CARTESIAN_POINT('',(-0.42693277500019,-0.260246816754091,1.));
#35098=CARTESIAN_POINT('',(-0.449655010132406,-0.301174676572776,0.66));
#35099=CARTESIAN_POINT('Origin',(-0.441672955930064,-0.255,0.66));
#35100=CARTESIAN_POINT('Origin',(0.,0.,0.66));
#35101=CARTESIAN_POINT('Origin',(-0.463644396618753,-0.12423314164921,0.66));
#35102=CARTESIAN_POINT('',(-0.485909349222455,-0.117864771404394,0.66));
#35103=CARTESIAN_POINT('',(-0.485909349222455,-0.117864771404394,1.34));
#35104=CARTESIAN_POINT('',(-0.485909349222455,-0.117864771404394,1.));
#35105=CARTESIAN_POINT('',(-0.463644396618753,-0.12423314164921,0.66));
#35106=CARTESIAN_POINT('',(-0.463644396618753,-0.12423314164921,0.66));
#35107=CARTESIAN_POINT('',(-0.463644396618753,-0.12423314164921,1.34));
#35108=CARTESIAN_POINT('',(-0.463644396618753,-0.12423314164921,0.66));
#35109=CARTESIAN_POINT('',(-0.463644396618753,-0.12423314164921,1.34));
#35110=CARTESIAN_POINT('Origin',(-0.492622171407425,-0.131997713002285,
1.34));
#35111=CARTESIAN_POINT('',(-0.479742226065208,-0.140880788363777,1.34));
#35112=CARTESIAN_POINT('Origin',(0.,0.,1.34));
#35113=CARTESIAN_POINT('',(-0.512283129406789,-0.174533117977868,1.34));
#35114=CARTESIAN_POINT('Origin',(-0.512283129406789,-0.174533117977868,
0.66));
#35115=CARTESIAN_POINT('',(-0.479742226065208,-0.140880788363777,0.66));
#35116=CARTESIAN_POINT('',(-0.479742226065208,-0.140880788363777,1.));
#35117=CARTESIAN_POINT('',(-0.512283129406789,-0.174533117977868,0.66));
#35118=CARTESIAN_POINT('Origin',(-0.492622171407425,-0.131997713002285,
0.66));
#35119=CARTESIAN_POINT('Origin',(0.,0.,0.66));
#35120=CARTESIAN_POINT('Origin',(-0.48,5.55111512312578E-17,0.66));
#35121=CARTESIAN_POINT('',(-0.499858037235396,0.0119139670629818,0.66));
#35122=CARTESIAN_POINT('',(-0.499858037235396,0.0119139670629818,1.34));
#35123=CARTESIAN_POINT('',(-0.499858037235396,0.0119139670629818,1.));
#35124=CARTESIAN_POINT('',(-0.48,5.55111512312578E-17,0.66));
#35125=CARTESIAN_POINT('',(-0.48,5.55111512312578E-17,0.66));
#35126=CARTESIAN_POINT('',(-0.48,5.55111512312578E-17,1.34));
#35127=CARTESIAN_POINT('',(-0.48,5.55111512312578E-17,0.66));
#35128=CARTESIAN_POINT('',(-0.48,5.55111512312578E-17,1.34));
#35129=CARTESIAN_POINT('Origin',(-0.51,5.55111512312578E-17,1.34));
#35130=CARTESIAN_POINT('',(-0.5,-6.12323399573677E-17,1.34));
#35131=CARTESIAN_POINT('Origin',(0.,0.,1.34));
#35132=CARTESIAN_POINT('',(-0.499858037235396,-0.0119139670629816,1.34));
#35133=CARTESIAN_POINT('',(-0.54,-0.035997415822383,1.34));
#35134=CARTESIAN_POINT('Origin',(0.,0.,1.34));
#35135=CARTESIAN_POINT('Origin',(-0.54,-0.035997415822383,0.66));
#35136=CARTESIAN_POINT('',(-0.499858037235396,-0.0119139670629816,0.66));
#35137=CARTESIAN_POINT('',(-0.499858037235396,-0.0119139670629816,1.));
#35138=CARTESIAN_POINT('',(-0.54,-0.035997415822383,0.66));
#35139=CARTESIAN_POINT('Origin',(-0.51,5.55111512312578E-17,0.66));
#35140=CARTESIAN_POINT('',(-0.5,-6.12323399573677E-17,0.66));
#35141=CARTESIAN_POINT('Origin',(0.,0.,0.66));
#35142=CARTESIAN_POINT('Origin',(0.,0.,0.66));
#35143=CARTESIAN_POINT('Origin',(-0.463644396618753,0.12423314164921,0.66));
#35144=CARTESIAN_POINT('',(-0.479742226065208,0.140880788363777,0.66));
#35145=CARTESIAN_POINT('',(-0.479742226065208,0.140880788363777,1.34));
#35146=CARTESIAN_POINT('',(-0.479742226065208,0.140880788363777,1.));
#35147=CARTESIAN_POINT('',(-0.463644396618753,0.12423314164921,0.66));
#35148=CARTESIAN_POINT('',(-0.463644396618753,0.12423314164921,0.66));
#35149=CARTESIAN_POINT('',(-0.463644396618753,0.12423314164921,1.34));
#35150=CARTESIAN_POINT('',(-0.463644396618753,0.12423314164921,0.66));
#35151=CARTESIAN_POINT('',(-0.463644396618753,0.12423314164921,1.34));
#35152=CARTESIAN_POINT('Origin',(-0.492622171407425,0.131997713002286,1.34));
#35153=CARTESIAN_POINT('',(-0.485909349222455,0.117864771404394,1.34));
#35154=CARTESIAN_POINT('Origin',(0.,0.,1.34));
#35155=CARTESIAN_POINT('',(-0.530916762985404,0.104991450732855,1.34));
#35156=CARTESIAN_POINT('Origin',(-0.530916762985404,0.104991450732855,0.66));
#35157=CARTESIAN_POINT('',(-0.485909349222455,0.117864771404394,0.66));
#35158=CARTESIAN_POINT('',(-0.485909349222455,0.117864771404394,1.));
#35159=CARTESIAN_POINT('',(-0.530916762985404,0.104991450732855,0.66));
#35160=CARTESIAN_POINT('Origin',(-0.492622171407425,0.131997713002286,0.66));
#35161=CARTESIAN_POINT('Origin',(0.,0.,0.66));
#35162=CARTESIAN_POINT('Origin',(-0.41569219381653,0.24,0.66));
#35163=CARTESIAN_POINT('',(-0.42693277500019,0.260246816754091,0.66));
#35164=CARTESIAN_POINT('',(-0.42693277500019,0.260246816754091,1.34));
#35165=CARTESIAN_POINT('',(-0.42693277500019,0.260246816754091,1.));
#35166=CARTESIAN_POINT('',(-0.41569219381653,0.24,0.66));
#35167=CARTESIAN_POINT('',(-0.41569219381653,0.24,0.66));
#35168=CARTESIAN_POINT('',(-0.41569219381653,0.24,1.34));
#35169=CARTESIAN_POINT('',(-0.41569219381653,0.24,0.66));
#35170=CARTESIAN_POINT('',(-0.41569219381653,0.24,1.34));
#35171=CARTESIAN_POINT('Origin',(-0.441672955930064,0.255,1.34));
#35172=CARTESIAN_POINT('',(-0.438846742063171,0.239611220481305,1.34));
#35173=CARTESIAN_POINT('Origin',(0.,0.,1.34));
#35174=CARTESIAN_POINT('',(-0.485652425954788,0.238825323427225,1.34));
#35175=CARTESIAN_POINT('Origin',(-0.485652425954788,0.238825323427225,0.66));
#35176=CARTESIAN_POINT('',(-0.438846742063171,0.239611220481305,0.66));
#35177=CARTESIAN_POINT('',(-0.438846742063171,0.239611220481305,1.));
#35178=CARTESIAN_POINT('',(-0.485652425954788,0.238825323427225,0.66));
#35179=CARTESIAN_POINT('Origin',(-0.441672955930064,0.255,0.66));
#35180=CARTESIAN_POINT('Origin',(0.,0.,0.66));
#35181=CARTESIAN_POINT('Origin',(-0.339411254969543,0.339411254969543,0.66));
#35182=CARTESIAN_POINT('',(-0.345028560858679,0.361877454660814,0.66));
#35183=CARTESIAN_POINT('',(-0.345028560858679,0.361877454660814,1.34));
#35184=CARTESIAN_POINT('',(-0.345028560858679,0.361877454660814,1.));
#35185=CARTESIAN_POINT('',(-0.339411254969543,0.339411254969543,0.66));
#35186=CARTESIAN_POINT('',(-0.339411254969543,0.339411254969543,0.66));
#35187=CARTESIAN_POINT('',(-0.339411254969543,0.339411254969543,1.34));
#35188=CARTESIAN_POINT('',(-0.339411254969543,0.339411254969543,0.66));
#35189=CARTESIAN_POINT('',(-0.339411254969543,0.339411254969543,1.34));
#35190=CARTESIAN_POINT('Origin',(-0.360624458405139,0.360624458405139,1.34));
#35191=CARTESIAN_POINT('',(-0.361877454660814,0.345028560858679,1.34));
#35192=CARTESIAN_POINT('Origin',(0.,0.,1.34));
#35193=CARTESIAN_POINT('',(-0.407291678673935,0.356383645007537,1.34));
#35194=CARTESIAN_POINT('Origin',(-0.407291678673935,0.356383645007537,0.66));
#35195=CARTESIAN_POINT('',(-0.361877454660814,0.345028560858679,0.66));
#35196=CARTESIAN_POINT('',(-0.361877454660814,0.345028560858679,1.));
#35197=CARTESIAN_POINT('',(-0.407291678673935,0.356383645007537,0.66));
#35198=CARTESIAN_POINT('Origin',(-0.360624458405139,0.360624458405139,0.66));
#35199=CARTESIAN_POINT('Origin',(0.,0.,0.66));
#35200=CARTESIAN_POINT('Origin',(-0.24,0.415692193816531,0.66));
#35201=CARTESIAN_POINT('',(-0.239611220481305,0.438846742063171,0.66));
#35202=CARTESIAN_POINT('',(-0.239611220481305,0.438846742063171,1.34));
#35203=CARTESIAN_POINT('',(-0.239611220481305,0.438846742063171,1.));
#35204=CARTESIAN_POINT('',(-0.24,0.415692193816531,0.66));
#35205=CARTESIAN_POINT('',(-0.24,0.415692193816531,0.66));
#35206=CARTESIAN_POINT('',(-0.24,0.415692193816531,1.34));
#35207=CARTESIAN_POINT('',(-0.24,0.415692193816531,0.66));
#35208=CARTESIAN_POINT('',(-0.24,0.415692193816531,1.34));
#35209=CARTESIAN_POINT('Origin',(-0.255,0.441672955930064,1.34));
#35210=CARTESIAN_POINT('',(-0.260246816754091,0.42693277500019,1.34));
#35211=CARTESIAN_POINT('Origin',(0.,0.,1.34));
#35212=CARTESIAN_POINT('',(-0.301174676572776,0.449655010132405,1.34));
#35213=CARTESIAN_POINT('Origin',(-0.301174676572776,0.449655010132405,0.66));
#35214=CARTESIAN_POINT('',(-0.260246816754091,0.42693277500019,0.66));
#35215=CARTESIAN_POINT('',(-0.260246816754091,0.42693277500019,1.));
#35216=CARTESIAN_POINT('',(-0.301174676572776,0.449655010132405,0.66));
#35217=CARTESIAN_POINT('Origin',(-0.255,0.441672955930064,0.66));
#35218=CARTESIAN_POINT('Origin',(0.,0.,0.66));
#35219=CARTESIAN_POINT('Origin',(-0.12423314164921,0.463644396618753,0.66));
#35220=CARTESIAN_POINT('',(-0.117864771404394,0.485909349222455,0.66));
#35221=CARTESIAN_POINT('',(-0.117864771404394,0.485909349222455,1.34));
#35222=CARTESIAN_POINT('',(-0.117864771404394,0.485909349222455,1.));
#35223=CARTESIAN_POINT('',(-0.12423314164921,0.463644396618753,0.66));
#35224=CARTESIAN_POINT('',(-0.12423314164921,0.463644396618753,0.66));
#35225=CARTESIAN_POINT('',(-0.12423314164921,0.463644396618753,1.34));
#35226=CARTESIAN_POINT('',(-0.12423314164921,0.463644396618753,0.66));
#35227=CARTESIAN_POINT('',(-0.12423314164921,0.463644396618753,1.34));
#35228=CARTESIAN_POINT('Origin',(-0.131997713002286,0.492622171407425,1.34));
#35229=CARTESIAN_POINT('',(-0.140880788363777,0.479742226065208,1.34));
#35230=CARTESIAN_POINT('Origin',(0.,0.,1.34));
#35231=CARTESIAN_POINT('',(-0.174533117977868,0.512283129406789,1.34));
#35232=CARTESIAN_POINT('Origin',(-0.174533117977868,0.512283129406789,0.66));
#35233=CARTESIAN_POINT('',(-0.140880788363777,0.479742226065208,0.66));
#35234=CARTESIAN_POINT('',(-0.140880788363777,0.479742226065208,1.));
#35235=CARTESIAN_POINT('',(-0.174533117977868,0.512283129406789,0.66));
#35236=CARTESIAN_POINT('Origin',(-0.131997713002286,0.492622171407425,0.66));
#35237=CARTESIAN_POINT('Origin',(0.,0.,0.66));
#35238=CARTESIAN_POINT('Origin',(2.77555756156289E-17,0.48,0.66));
#35239=CARTESIAN_POINT('',(0.0119139670629818,0.499858037235396,0.66));
#35240=CARTESIAN_POINT('',(0.0119139670629818,0.499858037235396,1.34));
#35241=CARTESIAN_POINT('',(0.0119139670629818,0.499858037235396,1.));
#35242=CARTESIAN_POINT('',(2.77555756156289E-17,0.48,0.66));
#35243=CARTESIAN_POINT('',(2.77555756156289E-17,0.48,0.66));
#35244=CARTESIAN_POINT('',(2.77555756156289E-17,0.48,1.34));
#35245=CARTESIAN_POINT('',(2.77555756156289E-17,0.48,0.66));
#35246=CARTESIAN_POINT('',(2.77555756156289E-17,0.48,1.34));
#35247=CARTESIAN_POINT('Origin',(2.77555756156289E-17,0.51,1.34));
#35248=CARTESIAN_POINT('',(-0.0119139670629817,0.499858037235396,1.34));
#35249=CARTESIAN_POINT('Origin',(0.,0.,1.34));
#35250=CARTESIAN_POINT('',(-0.035997415822383,0.54,1.34));
#35251=CARTESIAN_POINT('Origin',(-0.035997415822383,0.54,0.66));
#35252=CARTESIAN_POINT('',(-0.0119139670629817,0.499858037235396,0.66));
#35253=CARTESIAN_POINT('',(-0.0119139670629817,0.499858037235396,1.));
#35254=CARTESIAN_POINT('',(-0.035997415822383,0.54,0.66));
#35255=CARTESIAN_POINT('Origin',(2.77555756156289E-17,0.51,0.66));
#35256=CARTESIAN_POINT('Origin',(0.,0.,0.66));
#35257=CARTESIAN_POINT('Origin',(0.12423314164921,0.463644396618753,0.66));
#35258=CARTESIAN_POINT('',(0.140880788363777,0.479742226065208,0.66));
#35259=CARTESIAN_POINT('',(0.140880788363777,0.479742226065208,1.34));
#35260=CARTESIAN_POINT('',(0.140880788363777,0.479742226065208,1.));
#35261=CARTESIAN_POINT('',(0.12423314164921,0.463644396618753,0.66));
#35262=CARTESIAN_POINT('',(0.12423314164921,0.463644396618753,0.66));
#35263=CARTESIAN_POINT('',(0.12423314164921,0.463644396618753,1.34));
#35264=CARTESIAN_POINT('',(0.12423314164921,0.463644396618753,0.66));
#35265=CARTESIAN_POINT('',(0.12423314164921,0.463644396618753,1.34));
#35266=CARTESIAN_POINT('Origin',(0.131997713002286,0.492622171407425,1.34));
#35267=CARTESIAN_POINT('',(0.117864771404394,0.485909349222455,1.34));
#35268=CARTESIAN_POINT('Origin',(0.,0.,1.34));
#35269=CARTESIAN_POINT('',(0.104991450732855,0.530916762985404,1.34));
#35270=CARTESIAN_POINT('Origin',(0.104991450732855,0.530916762985404,0.66));
#35271=CARTESIAN_POINT('',(0.117864771404394,0.485909349222455,0.66));
#35272=CARTESIAN_POINT('',(0.117864771404394,0.485909349222455,1.));
#35273=CARTESIAN_POINT('',(0.104991450732855,0.530916762985404,0.66));
#35274=CARTESIAN_POINT('Origin',(0.131997713002286,0.492622171407425,0.66));
#35275=CARTESIAN_POINT('Origin',(0.,0.,0.66));
#35276=CARTESIAN_POINT('Origin',(0.24,0.415692193816531,0.66));
#35277=CARTESIAN_POINT('',(0.260246816754091,0.42693277500019,0.66));
#35278=CARTESIAN_POINT('',(0.260246816754091,0.42693277500019,1.34));
#35279=CARTESIAN_POINT('',(0.260246816754091,0.42693277500019,1.));
#35280=CARTESIAN_POINT('',(0.24,0.415692193816531,0.66));
#35281=CARTESIAN_POINT('',(0.24,0.415692193816531,0.66));
#35282=CARTESIAN_POINT('',(0.24,0.415692193816531,1.34));
#35283=CARTESIAN_POINT('',(0.24,0.415692193816531,0.66));
#35284=CARTESIAN_POINT('',(0.24,0.415692193816531,1.34));
#35285=CARTESIAN_POINT('Origin',(0.255,0.441672955930064,1.34));
#35286=CARTESIAN_POINT('',(0.239611220481305,0.438846742063171,1.34));
#35287=CARTESIAN_POINT('Origin',(0.,0.,1.34));
#35288=CARTESIAN_POINT('',(0.238825323427224,0.485652425954788,1.34));
#35289=CARTESIAN_POINT('Origin',(0.238825323427224,0.485652425954788,0.66));
#35290=CARTESIAN_POINT('',(0.239611220481305,0.438846742063171,0.66));
#35291=CARTESIAN_POINT('',(0.239611220481305,0.438846742063171,1.));
#35292=CARTESIAN_POINT('',(0.238825323427224,0.485652425954788,0.66));
#35293=CARTESIAN_POINT('Origin',(0.255,0.441672955930064,0.66));
#35294=CARTESIAN_POINT('Origin',(0.,0.,0.66));
#35295=CARTESIAN_POINT('Origin',(0.339411254969543,0.339411254969543,0.66));
#35296=CARTESIAN_POINT('',(0.361877454660814,0.345028560858679,0.66));
#35297=CARTESIAN_POINT('',(0.361877454660814,0.345028560858679,1.34));
#35298=CARTESIAN_POINT('',(0.361877454660814,0.345028560858679,1.));
#35299=CARTESIAN_POINT('',(0.339411254969543,0.339411254969543,0.66));
#35300=CARTESIAN_POINT('',(0.339411254969543,0.339411254969543,0.66));
#35301=CARTESIAN_POINT('',(0.339411254969543,0.339411254969543,1.34));
#35302=CARTESIAN_POINT('',(0.339411254969543,0.339411254969543,0.66));
#35303=CARTESIAN_POINT('',(0.339411254969543,0.339411254969543,1.34));
#35304=CARTESIAN_POINT('Origin',(0.360624458405139,0.360624458405139,1.34));
#35305=CARTESIAN_POINT('',(0.345028560858679,0.361877454660814,1.34));
#35306=CARTESIAN_POINT('Origin',(0.,0.,1.34));
#35307=CARTESIAN_POINT('',(0.356383645007537,0.407291678673935,1.34));
#35308=CARTESIAN_POINT('Origin',(0.356383645007537,0.407291678673935,0.66));
#35309=CARTESIAN_POINT('',(0.345028560858679,0.361877454660814,0.66));
#35310=CARTESIAN_POINT('',(0.345028560858679,0.361877454660814,1.));
#35311=CARTESIAN_POINT('',(0.356383645007537,0.407291678673935,0.66));
#35312=CARTESIAN_POINT('Origin',(0.360624458405139,0.360624458405139,0.66));
#35313=CARTESIAN_POINT('Origin',(0.,0.,0.66));
#35314=CARTESIAN_POINT('Origin',(0.415692193816531,0.24,0.66));
#35315=CARTESIAN_POINT('',(0.438846742063171,0.239611220481305,0.66));
#35316=CARTESIAN_POINT('',(0.438846742063171,0.239611220481305,1.34));
#35317=CARTESIAN_POINT('',(0.438846742063171,0.239611220481305,1.));
#35318=CARTESIAN_POINT('',(0.415692193816531,0.24,0.66));
#35319=CARTESIAN_POINT('',(0.415692193816531,0.24,0.66));
#35320=CARTESIAN_POINT('',(0.415692193816531,0.24,1.34));
#35321=CARTESIAN_POINT('',(0.415692193816531,0.24,0.66));
#35322=CARTESIAN_POINT('',(0.415692193816531,0.24,1.34));
#35323=CARTESIAN_POINT('Origin',(0.441672955930064,0.255,1.34));
#35324=CARTESIAN_POINT('',(0.42693277500019,0.260246816754091,1.34));
#35325=CARTESIAN_POINT('Origin',(0.,0.,1.34));
#35326=CARTESIAN_POINT('',(0.449655010132405,0.301174676572776,1.34));
#35327=CARTESIAN_POINT('Origin',(0.449655010132405,0.301174676572776,0.66));
#35328=CARTESIAN_POINT('',(0.42693277500019,0.260246816754091,0.66));
#35329=CARTESIAN_POINT('',(0.42693277500019,0.260246816754091,1.));
#35330=CARTESIAN_POINT('',(0.449655010132405,0.301174676572776,0.66));
#35331=CARTESIAN_POINT('Origin',(0.441672955930064,0.255,0.66));
#35332=CARTESIAN_POINT('Origin',(0.,0.,0.66));
#35333=CARTESIAN_POINT('Origin',(0.463644396618753,0.12423314164921,0.66));
#35334=CARTESIAN_POINT('',(0.485909349222455,0.117864771404394,0.66));
#35335=CARTESIAN_POINT('',(0.485909349222455,0.117864771404394,1.34));
#35336=CARTESIAN_POINT('',(0.485909349222455,0.117864771404394,1.));
#35337=CARTESIAN_POINT('',(0.463644396618753,0.12423314164921,0.66));
#35338=CARTESIAN_POINT('',(0.463644396618753,0.12423314164921,0.66));
#35339=CARTESIAN_POINT('',(0.463644396618753,0.12423314164921,1.34));
#35340=CARTESIAN_POINT('',(0.463644396618753,0.12423314164921,0.66));
#35341=CARTESIAN_POINT('',(0.463644396618753,0.12423314164921,1.34));
#35342=CARTESIAN_POINT('Origin',(0.492622171407425,0.131997713002286,1.34));
#35343=CARTESIAN_POINT('',(0.479742226065208,0.140880788363777,1.34));
#35344=CARTESIAN_POINT('Origin',(0.,0.,1.34));
#35345=CARTESIAN_POINT('',(0.512283129406789,0.174533117977868,1.34));
#35346=CARTESIAN_POINT('Origin',(0.512283129406789,0.174533117977868,0.66));
#35347=CARTESIAN_POINT('',(0.479742226065208,0.140880788363777,0.66));
#35348=CARTESIAN_POINT('',(0.479742226065208,0.140880788363777,1.));
#35349=CARTESIAN_POINT('',(0.512283129406789,0.174533117977868,0.66));
#35350=CARTESIAN_POINT('Origin',(0.492622171407425,0.131997713002286,0.66));
#35351=CARTESIAN_POINT('Origin',(0.,0.,0.66));
#35352=CARTESIAN_POINT('Origin',(0.48,0.,0.66));
#35353=CARTESIAN_POINT('',(0.499858037235396,-0.0119139670629817,0.66));
#35354=CARTESIAN_POINT('',(0.499858037235396,-0.0119139670629817,1.34));
#35355=CARTESIAN_POINT('',(0.499858037235396,-0.0119139670629817,1.));
#35356=CARTESIAN_POINT('',(0.48,0.,0.66));
#35357=CARTESIAN_POINT('',(0.48,0.,0.66));
#35358=CARTESIAN_POINT('',(0.48,0.,1.34));
#35359=CARTESIAN_POINT('',(0.48,0.,0.66));
#35360=CARTESIAN_POINT('',(0.48,0.,1.34));
#35361=CARTESIAN_POINT('Origin',(0.51,0.,1.34));
#35362=CARTESIAN_POINT('',(0.499858037235396,0.0119139670629817,1.34));
#35363=CARTESIAN_POINT('Origin',(0.,0.,1.34));
#35364=CARTESIAN_POINT('',(0.54,0.035997415822383,1.34));
#35365=CARTESIAN_POINT('Origin',(0.54,0.035997415822383,0.66));
#35366=CARTESIAN_POINT('',(0.499858037235396,0.0119139670629817,0.66));
#35367=CARTESIAN_POINT('',(0.499858037235396,0.0119139670629817,1.));
#35368=CARTESIAN_POINT('',(0.54,0.035997415822383,0.66));
#35369=CARTESIAN_POINT('Origin',(0.51,0.,0.66));
#35370=CARTESIAN_POINT('Origin',(0.,0.,0.66));
#35371=CARTESIAN_POINT('Origin',(0.,0.,1.43));
#35372=CARTESIAN_POINT('',(-0.06,-7.34788079488412E-18,1.66));
#35373=CARTESIAN_POINT('Origin',(0.,0.,1.66));
#35374=CARTESIAN_POINT('',(-0.06,-7.34788079488412E-18,1.2));
#35375=CARTESIAN_POINT('',(-0.06,-7.34788079488412E-18,1.43));
#35376=CARTESIAN_POINT('Origin',(0.,0.,1.2));
#35377=CARTESIAN_POINT('Origin',(0.,0.,1.68));
#35378=CARTESIAN_POINT('',(-0.0300000000000001,-3.67394039744207E-18,1.7));
#35379=CARTESIAN_POINT('Origin',(0.,0.,1.7));
#35380=CARTESIAN_POINT('',(-0.045,-5.51091059616309E-18,1.68));
#35381=CARTESIAN_POINT('Origin',(0.,0.,1.7));
#35382=CARTESIAN_POINT('Origin',(0.25,0.,1.2));
#35383=CARTESIAN_POINT('',(-0.25,-3.06161699786838E-17,1.2));
#35384=CARTESIAN_POINT('Origin',(0.,0.,1.2));
#35385=CARTESIAN_POINT('Origin',(0.,0.,1.525));
#35386=CARTESIAN_POINT('',(-0.25,3.06161699786838E-17,1.8));
#35387=CARTESIAN_POINT('',(-0.25,-3.06161699786838E-17,1.525));
#35388=CARTESIAN_POINT('Origin',(0.,0.,1.8));
#35389=CARTESIAN_POINT('Origin',(0.,0.,1.));
#35390=CARTESIAN_POINT('',(-0.5,-6.12323399573677E-17,1.4));
#35391=CARTESIAN_POINT('Origin',(0.,0.,1.4));
#35392=CARTESIAN_POINT('',(-0.5,-6.12323399573677E-17,1.));
#35393=CARTESIAN_POINT('',(-0.5,-6.12323399573677E-17,0.6));
#35394=CARTESIAN_POINT('',(-0.5,-6.12323399573677E-17,1.));
#35395=CARTESIAN_POINT('Origin',(0.,0.,0.6));
#35396=CARTESIAN_POINT('Origin',(0.52,0.,1.4));
#35397=CARTESIAN_POINT('',(-0.52,-6.36816335556624E-17,1.4));
#35398=CARTESIAN_POINT('Origin',(0.,0.,1.4));
#35399=CARTESIAN_POINT('Origin',(0.,0.,1.58));
#35400=CARTESIAN_POINT('',(-0.52,-6.36816335556624E-17,1.76));
#35401=CARTESIAN_POINT('Origin',(0.,0.,1.76));
#35402=CARTESIAN_POINT('',(-0.52,-6.36816335556624E-17,1.58));
#35403=CARTESIAN_POINT('Origin',(0.,0.,1.78));
#35404=CARTESIAN_POINT('',(-0.48,-5.8783046359073E-17,1.8));
#35405=CARTESIAN_POINT('Origin',(0.,0.,1.8));
#35406=CARTESIAN_POINT('',(-0.5,-6.12323399573677E-17,1.78));
#35407=CARTESIAN_POINT('Origin',(0.,0.,1.8));
#35408=CARTESIAN_POINT('Origin',(-0.317542648054294,-0.55,0.2));
#35409=CARTESIAN_POINT('',(0.317542648054294,-0.55,0.2));
#35410=CARTESIAN_POINT('',(-0.317542648054294,-0.55,0.2));
#35411=CARTESIAN_POINT('',(-0.158771324027147,-0.55,0.2));
#35412=CARTESIAN_POINT('',(0.317542648054294,-0.55,0.6));
#35413=CARTESIAN_POINT('',(0.317542648054294,-0.55,0.2));
#35414=CARTESIAN_POINT('',(-0.317542648054294,-0.55,0.6));
#35415=CARTESIAN_POINT('',(-0.317542648054294,-0.55,0.6));
#35416=CARTESIAN_POINT('',(-0.317542648054294,-0.55,0.2));
#35417=CARTESIAN_POINT('Origin',(-0.635085296108588,7.77755175064932E-17,
0.2));
#35418=CARTESIAN_POINT('',(-0.635085296108588,7.77755175064932E-17,0.2));
#35419=CARTESIAN_POINT('',(-0.555699634095015,-0.1375,0.2));
#35420=CARTESIAN_POINT('',(-0.635085296108588,1.11022302462516E-16,0.6));
#35421=CARTESIAN_POINT('',(-0.635085296108588,7.77755175064932E-17,0.6));
#35422=CARTESIAN_POINT('',(-0.635085296108588,7.77755175064932E-17,0.2));
#35423=CARTESIAN_POINT('Origin',(-0.317542648054294,0.55,0.2));
#35424=CARTESIAN_POINT('',(-0.317542648054294,0.55,0.2));
#35425=CARTESIAN_POINT('',(-0.396928310067868,0.4125,0.2));
#35426=CARTESIAN_POINT('',(-0.317542648054294,0.55,0.6));
#35427=CARTESIAN_POINT('',(-0.317542648054294,0.55,0.6));
#35428=CARTESIAN_POINT('',(-0.317542648054294,0.55,0.2));
#35429=CARTESIAN_POINT('Origin',(0.317542648054294,0.55,0.2));
#35430=CARTESIAN_POINT('',(0.317542648054294,0.55,0.2));
#35431=CARTESIAN_POINT('',(0.158771324027147,0.55,0.2));
#35432=CARTESIAN_POINT('',(0.317542648054294,0.55,0.6));
#35433=CARTESIAN_POINT('',(0.317542648054294,0.55,0.6));
#35434=CARTESIAN_POINT('',(0.317542648054294,0.55,0.2));
#35435=CARTESIAN_POINT('Origin',(0.635085296108588,0.,0.2));
#35436=CARTESIAN_POINT('',(0.635085296108588,0.,0.2));
#35437=CARTESIAN_POINT('',(0.555699634095015,0.1375,0.2));
#35438=CARTESIAN_POINT('',(0.635085296108588,0.,0.6));
#35439=CARTESIAN_POINT('',(0.635085296108588,0.,0.6));
#35440=CARTESIAN_POINT('',(0.635085296108588,0.,0.2));
#35441=CARTESIAN_POINT('Origin',(0.317542648054294,-0.55,0.2));
#35442=CARTESIAN_POINT('',(0.396928310067868,-0.4125,0.2));
#35443=CARTESIAN_POINT('',(0.317542648054294,-0.55,0.6));
#35444=CARTESIAN_POINT('Origin',(0.,1.11022302462516E-16,0.6));
#35445=CARTESIAN_POINT('Origin',(0.,0.,0.));
#35446=CARTESIAN_POINT('',(-0.7,0.7,0.));
#35447=CARTESIAN_POINT('',(-0.7,-0.7,0.));
#35448=CARTESIAN_POINT('',(-0.7,0.7,0.));
#35449=CARTESIAN_POINT('',(0.7,0.7,0.));
#35450=CARTESIAN_POINT('',(0.7,0.7,0.));
#35451=CARTESIAN_POINT('',(0.7,-0.7,0.));
#35452=CARTESIAN_POINT('',(0.7,-0.7,0.));
#35453=CARTESIAN_POINT('',(-0.7,-0.7,0.));
#35454=CARTESIAN_POINT('Origin',(0.,0.,0.));
#35455=CARTESIAN_POINT('Origin',(0.7,0.7,0.));
#35456=CARTESIAN_POINT('',(-0.7,0.7,0.2));
#35457=CARTESIAN_POINT('',(-0.7,0.7,0.));
#35458=CARTESIAN_POINT('',(0.7,0.7,0.2));
#35459=CARTESIAN_POINT('',(0.7,0.7,0.2));
#35460=CARTESIAN_POINT('',(0.7,0.7,0.));
#35461=CARTESIAN_POINT('Origin',(0.7,-0.7,0.));
#35462=CARTESIAN_POINT('',(0.7,-0.7,0.2));
#35463=CARTESIAN_POINT('',(0.7,-0.7,0.2));
#35464=CARTESIAN_POINT('',(0.7,-0.7,0.));
#35465=CARTESIAN_POINT('Origin',(-0.7,-0.7,0.));
#35466=CARTESIAN_POINT('',(-0.7,-0.7,0.2));
#35467=CARTESIAN_POINT('',(-0.7,-0.7,0.2));
#35468=CARTESIAN_POINT('',(-0.7,-0.7,0.));
#35469=CARTESIAN_POINT('Origin',(-0.7,0.7,0.));
#35470=CARTESIAN_POINT('',(-0.7,0.7,0.2));
#35471=CARTESIAN_POINT('Origin',(0.,0.,0.2));
#35472=CARTESIAN_POINT('Origin',(0.36,0.,-1.));
#35473=CARTESIAN_POINT('',(-0.36,-4.40872847693047E-17,-1.));
#35474=CARTESIAN_POINT('Origin',(0.,0.,-1.));
#35475=CARTESIAN_POINT('Origin',(0.,0.,-0.98));
#35476=CARTESIAN_POINT('',(-0.38,-4.65365783675994E-17,-0.98));
#35477=CARTESIAN_POINT('Origin',(0.,0.,-0.48));
#35478=CARTESIAN_POINT('',(0.,0.,0.));
#35479=CARTESIAN_POINT('Origin',(0.,0.,1.175));
#35480=CARTESIAN_POINT('',(3.7,-4.53119315684521E-16,1.2));
#35481=CARTESIAN_POINT('Origin',(0.,0.,1.2));
#35482=CARTESIAN_POINT('',(3.75,4.59242549680257E-16,1.15));
#35483=CARTESIAN_POINT('',(3.725,4.56180932682389E-16,1.175));
#35484=CARTESIAN_POINT('',(-3.75,-4.59242549680257E-16,1.15));
#35485=CARTESIAN_POINT('Origin',(0.,0.,1.15));
#35486=CARTESIAN_POINT('Origin',(0.,0.,1.15));
#35487=CARTESIAN_POINT('Origin',(0.,0.,0.6));
#35488=CARTESIAN_POINT('',(-3.75,-4.59242549680257E-16,0.05));
#35489=CARTESIAN_POINT('',(-3.75,-4.59242549680257E-16,0.6));
#35490=CARTESIAN_POINT('',(3.75,-4.59242549680257E-16,0.05));
#35491=CARTESIAN_POINT('Origin',(0.,0.,0.05));
#35492=CARTESIAN_POINT('Origin',(0.,0.,0.05));
#35493=CARTESIAN_POINT('Origin',(0.,0.,1.2));
#35494=CARTESIAN_POINT('Origin',(0.,0.,0.025));
#35495=CARTESIAN_POINT('',(3.7,4.53119315684521E-16,0.));
#35496=CARTESIAN_POINT('',(3.725,4.56180932682389E-16,0.025));
#35497=CARTESIAN_POINT('Origin',(0.,0.,0.));
#35498=CARTESIAN_POINT('Origin',(3.75,0.,0.));
#35499=CARTESIAN_POINT('',(0.,0.,0.));
#35500=CARTESIAN_POINT('Origin',(0.,0.,1.48));
#35501=CARTESIAN_POINT('',(-0.385,-4.71489017671731E-17,1.46));
#35502=CARTESIAN_POINT('Origin',(0.,0.,1.46));
#35503=CARTESIAN_POINT('',(-0.385,-4.71489017671731E-17,1.5));
#35504=CARTESIAN_POINT('',(-0.385,-4.71489017671731E-17,1.48));
#35505=CARTESIAN_POINT('Origin',(0.,0.,1.5));
#35506=CARTESIAN_POINT('Origin',(0.41,0.,1.46));
#35507=CARTESIAN_POINT('',(-0.4,4.89858719658941E-17,1.46));
#35508=CARTESIAN_POINT('Origin',(0.,0.,1.46));
#35509=CARTESIAN_POINT('Origin',(0.385,0.,1.5));
#35510=CARTESIAN_POINT('',(-0.4,-4.89858719658941E-17,1.5));
#35511=CARTESIAN_POINT('Origin',(0.,0.,1.5));
#35512=CARTESIAN_POINT('Origin',(0.,0.,0.8));
#35513=CARTESIAN_POINT('',(0.4,4.89858719658941E-17,1.58));
#35514=CARTESIAN_POINT('',(-0.4,-4.89858719658941E-17,1.58));
#35515=CARTESIAN_POINT('Origin',(0.,0.,1.58));
#35516=CARTESIAN_POINT('Origin',(0.,0.,1.58));
#35517=CARTESIAN_POINT('',(-0.4,-4.89858719658941E-17,0.8));
#35518=CARTESIAN_POINT('Origin',(0.,0.,0.12));
#35519=CARTESIAN_POINT('',(-0.385,-4.71489017671731E-17,0.1));
#35520=CARTESIAN_POINT('Origin',(0.,0.,0.1));
#35521=CARTESIAN_POINT('',(-0.385,-4.71489017671731E-17,0.14));
#35522=CARTESIAN_POINT('',(-0.385,-4.71489017671731E-17,0.12));
#35523=CARTESIAN_POINT('Origin',(0.,0.,0.14));
#35524=CARTESIAN_POINT('Origin',(0.41,0.,0.1));
#35525=CARTESIAN_POINT('',(-0.4,4.89858719658941E-17,0.1));
#35526=CARTESIAN_POINT('Origin',(0.,0.,0.1));
#35527=CARTESIAN_POINT('Origin',(0.385,0.,0.14));
#35528=CARTESIAN_POINT('',(-0.4,-4.89858719658941E-17,0.14));
#35529=CARTESIAN_POINT('Origin',(0.,0.,0.14));
#35530=CARTESIAN_POINT('Origin',(0.,0.,0.8));
#35531=CARTESIAN_POINT('',(-0.4,-4.89858719658941E-17,0.8));
#35532=CARTESIAN_POINT('Origin',(0.,0.,1.59));
#35533=CARTESIAN_POINT('',(0.38,-4.65365783675994E-17,1.6));
#35534=CARTESIAN_POINT('Origin',(0.,0.,1.6));
#35535=CARTESIAN_POINT('',(0.39,4.77612251667468E-17,1.59));
#35536=CARTESIAN_POINT('Origin',(0.,0.,0.8));
#35537=CARTESIAN_POINT('',(-0.4,-4.89858719658941E-17,0.02));
#35538=CARTESIAN_POINT('',(-0.4,-4.89858719658941E-17,0.8));
#35539=CARTESIAN_POINT('',(0.4,-4.89858719658941E-17,0.02));
#35540=CARTESIAN_POINT('Origin',(0.,0.,0.02));
#35541=CARTESIAN_POINT('Origin',(0.,0.,0.02));
#35542=CARTESIAN_POINT('Origin',(0.25,0.,1.6));
#35543=CARTESIAN_POINT('',(-0.25,-3.06161699786838E-17,1.6));
#35544=CARTESIAN_POINT('Origin',(0.,0.,1.6));
#35545=CARTESIAN_POINT('Origin',(0.,0.,0.01));
#35546=CARTESIAN_POINT('',(0.38,4.65365783675994E-17,0.));
#35547=CARTESIAN_POINT('',(0.39,4.77612251667468E-17,0.01));
#35548=CARTESIAN_POINT('Origin',(0.,0.,0.));
#35549=CARTESIAN_POINT('Origin',(0.4,0.,0.));
#35550=CARTESIAN_POINT('',(-0.25,-3.06161699786838E-17,0.));
#35551=CARTESIAN_POINT('Origin',(0.,0.,0.));
#35552=CARTESIAN_POINT('Origin',(0.,0.,0.8));
#35553=CARTESIAN_POINT('',(-0.25,-3.06161699786838E-17,0.8));
#35554=CARTESIAN_POINT('',(0.,0.,0.));
#35555=CARTESIAN_POINT('Origin',(0.,-1.77202349450337E-17,5.1056066017178));
#35556=CARTESIAN_POINT('',(0.578786796564404,-7.08809397801347E-17,5.1312132034356));
#35557=CARTESIAN_POINT('',(-0.578786796564404,-7.08809397801347E-17,5.1312132034356));
#35558=CARTESIAN_POINT('Origin',(0.,-3.54404698900674E-17,5.1312132034356));
#35559=CARTESIAN_POINT('Origin',(0.,-3.54404698900674E-17,5.1312132034356));
#35560=CARTESIAN_POINT('',(0.6,7.34788079488412E-17,5.08));
#35561=CARTESIAN_POINT('',(0.589393398282202,7.2179873864488E-17,5.1056066017178));
#35562=CARTESIAN_POINT('',(-0.6,-7.34788079488412E-17,5.08));
#35563=CARTESIAN_POINT('Origin',(0.,0.,5.08));
#35564=CARTESIAN_POINT('Origin',(0.,0.,5.08));
#35565=CARTESIAN_POINT('Origin',(0.,0.,4.93));
#35566=CARTESIAN_POINT('',(-0.6,-7.34788079488412E-17,4.78));
#35567=CARTESIAN_POINT('',(-0.6,-7.34788079488412E-17,4.93));
#35568=CARTESIAN_POINT('',(0.6,-7.34788079488412E-17,4.78));
#35569=CARTESIAN_POINT('Origin',(0.,0.,4.78));
#35570=CARTESIAN_POINT('Origin',(0.,0.,4.78));
#35571=CARTESIAN_POINT('Origin',(0.,0.,5.13));
#35572=CARTESIAN_POINT('',(-0.56,-6.85802207522518E-17,5.15));
#35573=CARTESIAN_POINT('Origin',(0.,0.,5.15));
#35574=CARTESIAN_POINT('',(-0.58,-7.10295143505465E-17,5.13));
#35575=CARTESIAN_POINT('Origin',(0.,0.,4.765));
#35576=CARTESIAN_POINT('',(0.57,6.98048675513991E-17,4.75));
#35577=CARTESIAN_POINT('',(0.585,7.16418377501202E-17,4.765));
#35578=CARTESIAN_POINT('Origin',(0.,0.,4.75));
#35579=CARTESIAN_POINT('Origin',(0.6,0.,4.75));
#35580=CARTESIAN_POINT('',(-0.4,-4.89858719658941E-17,4.75));
#35581=CARTESIAN_POINT('Origin',(0.,0.,4.75));
#35582=CARTESIAN_POINT('Origin',(0.263113933820054,-0.0957656401311874,
5.25));
#35583=CARTESIAN_POINT('',(0.278507289184601,-0.111506456633887,5.25));
#35584=CARTESIAN_POINT('',(0.278507289184601,-0.111506456633887,5.75));
#35585=CARTESIAN_POINT('',(0.278507289184601,-0.111506456633887,5.475));
#35586=CARTESIAN_POINT('',(0.263113933820054,-0.0957656401311874,5.25));
#35587=CARTESIAN_POINT('',(0.263113933820054,-0.0957656401311874,5.25));
#35588=CARTESIAN_POINT('',(0.263113933820054,-0.0957656401311874,5.75));
#35589=CARTESIAN_POINT('',(0.263113933820054,-0.0957656401311874,5.25));
#35590=CARTESIAN_POINT('',(0.263113933820054,-0.0957656401311874,5.75));
#35591=CARTESIAN_POINT('Origin',(0.291304712443632,-0.106026244430958,5.75));
#35592=CARTESIAN_POINT('',(0.285023929972306,-0.0936021332189712,5.75));
#35593=CARTESIAN_POINT('Origin',(0.,0.,5.75));
#35594=CARTESIAN_POINT('',(0.329344964122349,-0.0892256439182034,5.75));
#35595=CARTESIAN_POINT('Origin',(0.329344964122349,-0.0892256439182034,
5.25));
#35596=CARTESIAN_POINT('',(0.285023929972306,-0.0936021332189712,5.25));
#35597=CARTESIAN_POINT('',(0.285023929972306,-0.0936021332189712,5.475));
#35598=CARTESIAN_POINT('',(0.329344964122349,-0.0892256439182034,5.25));
#35599=CARTESIAN_POINT('Origin',(0.291304712443632,-0.106026244430958,5.25));
#35600=CARTESIAN_POINT('Origin',(0.,0.,5.25));
#35601=CARTESIAN_POINT('Origin',(0.214492444073314,-0.179980530712231,5.25));
#35602=CARTESIAN_POINT('',(0.223573790202197,-0.200036897433009,5.25));
#35603=CARTESIAN_POINT('',(0.223573790202197,-0.200036897433009,5.75));
#35604=CARTESIAN_POINT('',(0.223573790202197,-0.200036897433009,5.475));
#35605=CARTESIAN_POINT('',(0.214492444073314,-0.179980530712231,5.25));
#35606=CARTESIAN_POINT('',(0.214492444073314,-0.179980530712231,5.25));
#35607=CARTESIAN_POINT('',(0.214492444073314,-0.179980530712231,5.75));
#35608=CARTESIAN_POINT('',(0.214492444073314,-0.179980530712231,5.25));
#35609=CARTESIAN_POINT('',(0.214492444073314,-0.179980530712231,5.75));
#35610=CARTESIAN_POINT('Origin',(0.237473777366883,-0.199264159002827,5.75));
#35611=CARTESIAN_POINT('',(0.235821068723235,-0.18544115925606,5.75));
#35612=CARTESIAN_POINT('Origin',(0.,0.,5.75));
#35613=CARTESIAN_POINT('',(0.278966064957542,-0.19648729100752,5.75));
#35614=CARTESIAN_POINT('Origin',(0.278966064957542,-0.19648729100752,5.25));
#35615=CARTESIAN_POINT('',(0.235821068723235,-0.18544115925606,5.25));
#35616=CARTESIAN_POINT('',(0.235821068723235,-0.18544115925606,5.475));
#35617=CARTESIAN_POINT('',(0.278966064957542,-0.19648729100752,5.25));
#35618=CARTESIAN_POINT('Origin',(0.237473777366883,-0.199264159002827,5.25));
#35619=CARTESIAN_POINT('Origin',(0.,0.,5.25));
#35620=CARTESIAN_POINT('Origin',(0.14,-0.242487113059643,5.25));
#35621=CARTESIAN_POINT('',(0.141673992523682,-0.264439936171524,5.25));
#35622=CARTESIAN_POINT('',(0.141673992523682,-0.264439936171524,5.75));
#35623=CARTESIAN_POINT('',(0.141673992523682,-0.264439936171524,5.475));
#35624=CARTESIAN_POINT('',(0.14,-0.242487113059643,5.25));
#35625=CARTESIAN_POINT('',(0.14,-0.242487113059643,5.25));
#35626=CARTESIAN_POINT('',(0.14,-0.242487113059643,5.75));
#35627=CARTESIAN_POINT('',(0.14,-0.242487113059643,5.25));
#35628=CARTESIAN_POINT('',(0.14,-0.242487113059643,5.75));
#35629=CARTESIAN_POINT('Origin',(0.155,-0.268467875173176,5.75));
#35630=CARTESIAN_POINT('',(0.158174706237834,-0.254913244666837,5.75));
#35631=CARTESIAN_POINT('Origin',(0.,0.,5.75));
#35632=CARTESIAN_POINT('',(0.194939741258221,-0.280049670957756,5.75));
#35633=CARTESIAN_POINT('Origin',(0.194939741258221,-0.280049670957756,5.25));
#35634=CARTESIAN_POINT('',(0.158174706237834,-0.254913244666837,5.25));
#35635=CARTESIAN_POINT('',(0.158174706237834,-0.254913244666837,5.475));
#35636=CARTESIAN_POINT('',(0.194939741258221,-0.280049670957756,5.25));
#35637=CARTESIAN_POINT('Origin',(0.155,-0.268467875173176,5.25));
#35638=CARTESIAN_POINT('Origin',(0.,0.,5.25));
#35639=CARTESIAN_POINT('Origin',(0.0486214897467404,-0.275746170843418,
5.25));
#35640=CARTESIAN_POINT('',(0.0426862204613663,-0.296947615889947,5.25));
#35641=CARTESIAN_POINT('',(0.0426862204613663,-0.296947615889947,5.75));
#35642=CARTESIAN_POINT('',(0.0426862204613663,-0.296947615889947,5.475));
#35643=CARTESIAN_POINT('',(0.0486214897467404,-0.275746170843418,5.25));
#35644=CARTESIAN_POINT('',(0.0486214897467404,-0.275746170843418,5.25));
#35645=CARTESIAN_POINT('',(0.0486214897467404,-0.275746170843418,5.75));
#35646=CARTESIAN_POINT('',(0.0486214897467404,-0.275746170843418,5.25));
#35647=CARTESIAN_POINT('',(0.0486214897467404,-0.275746170843418,5.75));
#35648=CARTESIAN_POINT('Origin',(0.0538309350767483,-0.305290403433784,
5.75));
#35649=CARTESIAN_POINT('',(0.0614501397701088,-0.293639030651979,5.75));
#35650=CARTESIAN_POINT('Origin',(0.,0.,5.75));
#35651=CARTESIAN_POINT('',(0.0874008077589859,-0.32983392749753,5.75));
#35652=CARTESIAN_POINT('Origin',(0.0874008077589859,-0.32983392749753,5.25));
#35653=CARTESIAN_POINT('',(0.0614501397701088,-0.293639030651979,5.25));
#35654=CARTESIAN_POINT('',(0.0614501397701088,-0.293639030651979,5.475));
#35655=CARTESIAN_POINT('',(0.0874008077589859,-0.32983392749753,5.25));
#35656=CARTESIAN_POINT('Origin',(0.0538309350767483,-0.305290403433784,
5.25));
#35657=CARTESIAN_POINT('Origin',(0.,0.,5.25));
#35658=CARTESIAN_POINT('Origin',(-0.0486214897467405,-0.275746170843418,
5.25));
#35659=CARTESIAN_POINT('',(-0.0614501397701088,-0.293639030651979,5.25));
#35660=CARTESIAN_POINT('',(-0.0614501397701088,-0.293639030651979,5.75));
#35661=CARTESIAN_POINT('',(-0.0614501397701088,-0.293639030651979,5.475));
#35662=CARTESIAN_POINT('',(-0.0486214897467405,-0.275746170843418,5.25));
#35663=CARTESIAN_POINT('',(-0.0486214897467405,-0.275746170843418,5.25));
#35664=CARTESIAN_POINT('',(-0.0486214897467405,-0.275746170843418,5.75));
#35665=CARTESIAN_POINT('',(-0.0486214897467405,-0.275746170843418,5.25));
#35666=CARTESIAN_POINT('',(-0.0486214897467405,-0.275746170843418,5.75));
#35667=CARTESIAN_POINT('Origin',(-0.0538309350767484,-0.305290403433785,
5.75));
#35668=CARTESIAN_POINT('',(-0.0426862204613664,-0.296947615889947,5.75));
#35669=CARTESIAN_POINT('Origin',(0.,0.,5.75));
#35670=CARTESIAN_POINT('',(-0.0306799530545266,-0.339835344550771,5.75));
#35671=CARTESIAN_POINT('Origin',(-0.0306799530545266,-0.339835344550771,
5.25));
#35672=CARTESIAN_POINT('',(-0.0426862204613664,-0.296947615889947,5.25));
#35673=CARTESIAN_POINT('',(-0.0426862204613664,-0.296947615889947,5.475));
#35674=CARTESIAN_POINT('',(-0.0306799530545266,-0.339835344550771,5.25));
#35675=CARTESIAN_POINT('Origin',(-0.0538309350767484,-0.305290403433785,
5.25));
#35676=CARTESIAN_POINT('Origin',(0.,0.,5.25));
#35677=CARTESIAN_POINT('Origin',(-0.14,-0.242487113059643,5.25));
#35678=CARTESIAN_POINT('',(-0.158174706237835,-0.254913244666837,5.25));
#35679=CARTESIAN_POINT('',(-0.158174706237835,-0.254913244666837,5.75));
#35680=CARTESIAN_POINT('',(-0.158174706237835,-0.254913244666837,5.475));
#35681=CARTESIAN_POINT('',(-0.14,-0.242487113059643,5.25));
#35682=CARTESIAN_POINT('',(-0.14,-0.242487113059643,5.25));
#35683=CARTESIAN_POINT('',(-0.14,-0.242487113059643,5.75));
#35684=CARTESIAN_POINT('',(-0.14,-0.242487113059643,5.25));
#35685=CARTESIAN_POINT('',(-0.14,-0.242487113059643,5.75));
#35686=CARTESIAN_POINT('Origin',(-0.155,-0.268467875173176,5.75));
#35687=CARTESIAN_POINT('',(-0.141673992523682,-0.264439936171524,5.75));
#35688=CARTESIAN_POINT('Origin',(0.,0.,5.75));
#35689=CARTESIAN_POINT('',(-0.14506025874178,-0.308847603615662,5.75));
#35690=CARTESIAN_POINT('Origin',(-0.14506025874178,-0.308847603615662,5.25));
#35691=CARTESIAN_POINT('',(-0.141673992523682,-0.264439936171524,5.25));
#35692=CARTESIAN_POINT('',(-0.141673992523682,-0.264439936171524,5.475));
#35693=CARTESIAN_POINT('',(-0.14506025874178,-0.308847603615662,5.25));
#35694=CARTESIAN_POINT('Origin',(-0.155,-0.268467875173176,5.25));
#35695=CARTESIAN_POINT('Origin',(0.,0.,5.25));
#35696=CARTESIAN_POINT('Origin',(-0.214492444073314,-0.179980530712231,
5.25));
#35697=CARTESIAN_POINT('',(-0.235821068723235,-0.18544115925606,5.25));
#35698=CARTESIAN_POINT('',(-0.235821068723235,-0.18544115925606,5.75));
#35699=CARTESIAN_POINT('',(-0.235821068723235,-0.18544115925606,5.475));
#35700=CARTESIAN_POINT('',(-0.214492444073314,-0.179980530712231,5.25));
#35701=CARTESIAN_POINT('',(-0.214492444073314,-0.179980530712231,5.25));
#35702=CARTESIAN_POINT('',(-0.214492444073314,-0.179980530712231,5.75));
#35703=CARTESIAN_POINT('',(-0.214492444073314,-0.179980530712231,5.25));
#35704=CARTESIAN_POINT('',(-0.214492444073314,-0.179980530712231,5.75));
#35705=CARTESIAN_POINT('Origin',(-0.237473777366883,-0.199264159002827,
5.75));
#35706=CARTESIAN_POINT('',(-0.223573790202197,-0.200036897433008,5.75));
#35707=CARTESIAN_POINT('Origin',(0.,0.,5.75));
#35708=CARTESIAN_POINT('',(-0.241944156363363,-0.240608283579327,5.75));
#35709=CARTESIAN_POINT('Origin',(-0.241944156363363,-0.240608283579327,
5.25));
#35710=CARTESIAN_POINT('',(-0.223573790202197,-0.200036897433008,5.25));
#35711=CARTESIAN_POINT('',(-0.223573790202197,-0.200036897433008,5.475));
#35712=CARTESIAN_POINT('',(-0.241944156363363,-0.240608283579327,5.25));
#35713=CARTESIAN_POINT('Origin',(-0.237473777366883,-0.199264159002827,
5.25));
#35714=CARTESIAN_POINT('Origin',(0.,0.,5.25));
#35715=CARTESIAN_POINT('Origin',(-0.263113933820054,-0.0957656401311872,
5.25));
#35716=CARTESIAN_POINT('',(-0.285023929972306,-0.0936021332189709,5.25));
#35717=CARTESIAN_POINT('',(-0.285023929972306,-0.0936021332189709,5.75));
#35718=CARTESIAN_POINT('',(-0.285023929972306,-0.0936021332189709,5.475));
#35719=CARTESIAN_POINT('',(-0.263113933820054,-0.0957656401311872,5.25));
#35720=CARTESIAN_POINT('',(-0.263113933820054,-0.0957656401311872,5.25));
#35721=CARTESIAN_POINT('',(-0.263113933820054,-0.0957656401311872,5.75));
#35722=CARTESIAN_POINT('',(-0.263113933820054,-0.0957656401311872,5.25));
#35723=CARTESIAN_POINT('',(-0.263113933820054,-0.0957656401311872,5.75));
#35724=CARTESIAN_POINT('Origin',(-0.291304712443632,-0.106026244430957,
5.75));
#35725=CARTESIAN_POINT('',(-0.278507289184601,-0.111506456633887,5.75));
#35726=CARTESIAN_POINT('Origin',(0.,0.,5.75));
#35727=CARTESIAN_POINT('',(-0.309646018012069,-0.143348053543252,5.75));
#35728=CARTESIAN_POINT('Origin',(-0.309646018012069,-0.143348053543252,
5.25));
#35729=CARTESIAN_POINT('',(-0.278507289184601,-0.111506456633887,5.25));
#35730=CARTESIAN_POINT('',(-0.278507289184601,-0.111506456633887,5.475));
#35731=CARTESIAN_POINT('',(-0.309646018012069,-0.143348053543252,5.25));
#35732=CARTESIAN_POINT('Origin',(-0.291304712443632,-0.106026244430957,
5.25));
#35733=CARTESIAN_POINT('Origin',(0.,0.,5.25));
#35734=CARTESIAN_POINT('Origin',(-0.28,1.38777878078145E-17,5.25));
#35735=CARTESIAN_POINT('',(-0.299848698761516,0.00952669150468696,5.25));
#35736=CARTESIAN_POINT('',(-0.299848698761516,0.00952669150468696,5.75));
#35737=CARTESIAN_POINT('',(-0.299848698761516,0.00952669150468698,5.475));
#35738=CARTESIAN_POINT('',(-0.28,1.38777878078145E-17,5.25));
#35739=CARTESIAN_POINT('',(-0.28,1.38777878078145E-17,5.25));
#35740=CARTESIAN_POINT('',(-0.28,1.38777878078145E-17,5.75));
#35741=CARTESIAN_POINT('',(-0.28,1.38777878078145E-17,5.25));
#35742=CARTESIAN_POINT('',(-0.28,1.38777878078145E-17,5.75));
#35743=CARTESIAN_POINT('Origin',(-0.31,2.77555756156289E-17,5.75));
#35744=CARTESIAN_POINT('',(-0.3,-3.67394039744206E-17,5.75));
#35745=CARTESIAN_POINT('Origin',(0.,0.,5.75));
#35746=CARTESIAN_POINT('',(-0.299848698761516,-0.00952669150468687,5.75));
#35747=CARTESIAN_POINT('',(-0.34,-0.0287979326579064,5.75));
#35748=CARTESIAN_POINT('Origin',(0.,0.,5.75));
#35749=CARTESIAN_POINT('Origin',(-0.34,-0.0287979326579064,5.25));
#35750=CARTESIAN_POINT('',(-0.299848698761516,-0.00952669150468687,5.25));
#35751=CARTESIAN_POINT('',(-0.299848698761516,-0.00952669150468689,5.475));
#35752=CARTESIAN_POINT('',(-0.34,-0.0287979326579064,5.25));
#35753=CARTESIAN_POINT('Origin',(-0.31,2.77555756156289E-17,5.25));
#35754=CARTESIAN_POINT('',(-0.3,-3.67394039744206E-17,5.25));
#35755=CARTESIAN_POINT('Origin',(0.,0.,5.25));
#35756=CARTESIAN_POINT('Origin',(0.,0.,5.25));
#35757=CARTESIAN_POINT('Origin',(-0.263113933820054,0.0957656401311873,
5.25));
#35758=CARTESIAN_POINT('',(-0.278507289184601,0.111506456633887,5.25));
#35759=CARTESIAN_POINT('',(-0.278507289184601,0.111506456633887,5.75));
#35760=CARTESIAN_POINT('',(-0.278507289184601,0.111506456633887,5.475));
#35761=CARTESIAN_POINT('',(-0.263113933820054,0.0957656401311873,5.25));
#35762=CARTESIAN_POINT('',(-0.263113933820054,0.0957656401311873,5.25));
#35763=CARTESIAN_POINT('',(-0.263113933820054,0.0957656401311873,5.75));
#35764=CARTESIAN_POINT('',(-0.263113933820054,0.0957656401311873,5.25));
#35765=CARTESIAN_POINT('',(-0.263113933820054,0.0957656401311873,5.75));
#35766=CARTESIAN_POINT('Origin',(-0.291304712443632,0.106026244430957,5.75));
#35767=CARTESIAN_POINT('',(-0.285023929972306,0.093602133218971,5.75));
#35768=CARTESIAN_POINT('Origin',(0.,0.,5.75));
#35769=CARTESIAN_POINT('',(-0.329344964122349,0.0892256439182032,5.75));
#35770=CARTESIAN_POINT('Origin',(-0.329344964122349,0.0892256439182032,
5.25));
#35771=CARTESIAN_POINT('',(-0.285023929972306,0.093602133218971,5.25));
#35772=CARTESIAN_POINT('',(-0.285023929972306,0.093602133218971,5.475));
#35773=CARTESIAN_POINT('',(-0.329344964122349,0.0892256439182032,5.25));
#35774=CARTESIAN_POINT('Origin',(-0.291304712443632,0.106026244430957,5.25));
#35775=CARTESIAN_POINT('Origin',(0.,0.,5.25));
#35776=CARTESIAN_POINT('Origin',(-0.214492444073314,0.179980530712231,5.25));
#35777=CARTESIAN_POINT('',(-0.223573790202197,0.200036897433008,5.25));
#35778=CARTESIAN_POINT('',(-0.223573790202197,0.200036897433008,5.75));
#35779=CARTESIAN_POINT('',(-0.223573790202197,0.200036897433008,5.475));
#35780=CARTESIAN_POINT('',(-0.214492444073314,0.179980530712231,5.25));
#35781=CARTESIAN_POINT('',(-0.214492444073314,0.179980530712231,5.25));
#35782=CARTESIAN_POINT('',(-0.214492444073314,0.179980530712231,5.75));
#35783=CARTESIAN_POINT('',(-0.214492444073314,0.179980530712231,5.25));
#35784=CARTESIAN_POINT('',(-0.214492444073314,0.179980530712231,5.75));
#35785=CARTESIAN_POINT('Origin',(-0.237473777366883,0.199264159002827,5.75));
#35786=CARTESIAN_POINT('',(-0.235821068723235,0.18544115925606,5.75));
#35787=CARTESIAN_POINT('Origin',(0.,0.,5.75));
#35788=CARTESIAN_POINT('',(-0.278966064957542,0.19648729100752,5.75));
#35789=CARTESIAN_POINT('Origin',(-0.278966064957542,0.19648729100752,5.25));
#35790=CARTESIAN_POINT('',(-0.235821068723235,0.18544115925606,5.25));
#35791=CARTESIAN_POINT('',(-0.235821068723235,0.18544115925606,5.475));
#35792=CARTESIAN_POINT('',(-0.278966064957542,0.19648729100752,5.25));
#35793=CARTESIAN_POINT('Origin',(-0.237473777366883,0.199264159002827,5.25));
#35794=CARTESIAN_POINT('Origin',(0.,0.,5.25));
#35795=CARTESIAN_POINT('Origin',(-0.14,0.242487113059643,5.25));
#35796=CARTESIAN_POINT('',(-0.141673992523682,0.264439936171524,5.25));
#35797=CARTESIAN_POINT('',(-0.141673992523682,0.264439936171524,5.75));
#35798=CARTESIAN_POINT('',(-0.141673992523682,0.264439936171524,5.475));
#35799=CARTESIAN_POINT('',(-0.14,0.242487113059643,5.25));
#35800=CARTESIAN_POINT('',(-0.14,0.242487113059643,5.25));
#35801=CARTESIAN_POINT('',(-0.14,0.242487113059643,5.75));
#35802=CARTESIAN_POINT('',(-0.14,0.242487113059643,5.25));
#35803=CARTESIAN_POINT('',(-0.14,0.242487113059643,5.75));
#35804=CARTESIAN_POINT('Origin',(-0.155,0.268467875173176,5.75));
#35805=CARTESIAN_POINT('',(-0.158174706237834,0.254913244666837,5.75));
#35806=CARTESIAN_POINT('Origin',(0.,0.,5.75));
#35807=CARTESIAN_POINT('',(-0.19493974125822,0.280049670957756,5.75));
#35808=CARTESIAN_POINT('Origin',(-0.19493974125822,0.280049670957756,5.25));
#35809=CARTESIAN_POINT('',(-0.158174706237834,0.254913244666837,5.25));
#35810=CARTESIAN_POINT('',(-0.158174706237834,0.254913244666837,5.475));
#35811=CARTESIAN_POINT('',(-0.19493974125822,0.280049670957756,5.25));
#35812=CARTESIAN_POINT('Origin',(-0.155,0.268467875173176,5.25));
#35813=CARTESIAN_POINT('Origin',(0.,0.,5.25));
#35814=CARTESIAN_POINT('Origin',(-0.0486214897467405,0.275746170843418,
5.25));
#35815=CARTESIAN_POINT('',(-0.0426862204613664,0.296947615889947,5.25));
#35816=CARTESIAN_POINT('',(-0.0426862204613664,0.296947615889947,5.75));
#35817=CARTESIAN_POINT('',(-0.0426862204613664,0.296947615889947,5.475));
#35818=CARTESIAN_POINT('',(-0.0486214897467405,0.275746170843418,5.25));
#35819=CARTESIAN_POINT('',(-0.0486214897467405,0.275746170843418,5.25));
#35820=CARTESIAN_POINT('',(-0.0486214897467405,0.275746170843418,5.75));
#35821=CARTESIAN_POINT('',(-0.0486214897467405,0.275746170843418,5.25));
#35822=CARTESIAN_POINT('',(-0.0486214897467405,0.275746170843418,5.75));
#35823=CARTESIAN_POINT('Origin',(-0.0538309350767484,0.305290403433784,
5.75));
#35824=CARTESIAN_POINT('',(-0.0614501397701089,0.293639030651979,5.75));
#35825=CARTESIAN_POINT('Origin',(0.,0.,5.75));
#35826=CARTESIAN_POINT('',(-0.0874008077589861,0.32983392749753,5.75));
#35827=CARTESIAN_POINT('Origin',(-0.0874008077589861,0.32983392749753,5.25));
#35828=CARTESIAN_POINT('',(-0.0614501397701089,0.293639030651979,5.25));
#35829=CARTESIAN_POINT('',(-0.0614501397701089,0.293639030651979,5.475));
#35830=CARTESIAN_POINT('',(-0.0874008077589861,0.32983392749753,5.25));
#35831=CARTESIAN_POINT('Origin',(-0.0538309350767484,0.305290403433784,
5.25));
#35832=CARTESIAN_POINT('Origin',(0.,0.,5.25));
#35833=CARTESIAN_POINT('Origin',(0.0486214897467405,0.275746170843418,5.25));
#35834=CARTESIAN_POINT('',(0.0614501397701089,0.293639030651979,5.25));
#35835=CARTESIAN_POINT('',(0.0614501397701089,0.293639030651979,5.75));
#35836=CARTESIAN_POINT('',(0.0614501397701089,0.293639030651979,5.475));
#35837=CARTESIAN_POINT('',(0.0486214897467405,0.275746170843418,5.25));
#35838=CARTESIAN_POINT('',(0.0486214897467405,0.275746170843418,5.25));
#35839=CARTESIAN_POINT('',(0.0486214897467405,0.275746170843418,5.75));
#35840=CARTESIAN_POINT('',(0.0486214897467405,0.275746170843418,5.25));
#35841=CARTESIAN_POINT('',(0.0486214897467405,0.275746170843418,5.75));
#35842=CARTESIAN_POINT('Origin',(0.0538309350767484,0.305290403433784,5.75));
#35843=CARTESIAN_POINT('',(0.0426862204613665,0.296947615889947,5.75));
#35844=CARTESIAN_POINT('Origin',(0.,0.,5.75));
#35845=CARTESIAN_POINT('',(0.0306799530545266,0.339835344550771,5.75));
#35846=CARTESIAN_POINT('Origin',(0.0306799530545266,0.339835344550771,5.25));
#35847=CARTESIAN_POINT('',(0.0426862204613665,0.296947615889947,5.25));
#35848=CARTESIAN_POINT('',(0.0426862204613665,0.296947615889947,5.475));
#35849=CARTESIAN_POINT('',(0.0306799530545266,0.339835344550771,5.25));
#35850=CARTESIAN_POINT('Origin',(0.0538309350767484,0.305290403433784,5.25));
#35851=CARTESIAN_POINT('Origin',(0.,0.,5.25));
#35852=CARTESIAN_POINT('Origin',(0.14,0.242487113059643,5.25));
#35853=CARTESIAN_POINT('',(0.158174706237834,0.254913244666837,5.25));
#35854=CARTESIAN_POINT('',(0.158174706237834,0.254913244666837,5.75));
#35855=CARTESIAN_POINT('',(0.158174706237834,0.254913244666837,5.475));
#35856=CARTESIAN_POINT('',(0.14,0.242487113059643,5.25));
#35857=CARTESIAN_POINT('',(0.14,0.242487113059643,5.25));
#35858=CARTESIAN_POINT('',(0.14,0.242487113059643,5.75));
#35859=CARTESIAN_POINT('',(0.14,0.242487113059643,5.25));
#35860=CARTESIAN_POINT('',(0.14,0.242487113059643,5.75));
#35861=CARTESIAN_POINT('Origin',(0.155,0.268467875173176,5.75));
#35862=CARTESIAN_POINT('',(0.141673992523682,0.264439936171524,5.75));
#35863=CARTESIAN_POINT('Origin',(0.,0.,5.75));
#35864=CARTESIAN_POINT('',(0.14506025874178,0.308847603615662,5.75));
#35865=CARTESIAN_POINT('Origin',(0.14506025874178,0.308847603615662,5.25));
#35866=CARTESIAN_POINT('',(0.141673992523682,0.264439936171524,5.25));
#35867=CARTESIAN_POINT('',(0.141673992523682,0.264439936171524,5.475));
#35868=CARTESIAN_POINT('',(0.14506025874178,0.308847603615662,5.25));
#35869=CARTESIAN_POINT('Origin',(0.155,0.268467875173176,5.25));
#35870=CARTESIAN_POINT('Origin',(0.,0.,5.25));
#35871=CARTESIAN_POINT('Origin',(0.214492444073314,0.179980530712231,5.25));
#35872=CARTESIAN_POINT('',(0.235821068723235,0.18544115925606,5.25));
#35873=CARTESIAN_POINT('',(0.235821068723235,0.18544115925606,5.75));
#35874=CARTESIAN_POINT('',(0.235821068723235,0.18544115925606,5.475));
#35875=CARTESIAN_POINT('',(0.214492444073314,0.179980530712231,5.25));
#35876=CARTESIAN_POINT('',(0.214492444073314,0.179980530712231,5.25));
#35877=CARTESIAN_POINT('',(0.214492444073314,0.179980530712231,5.75));
#35878=CARTESIAN_POINT('',(0.214492444073314,0.179980530712231,5.25));
#35879=CARTESIAN_POINT('',(0.214492444073314,0.179980530712231,5.75));
#35880=CARTESIAN_POINT('Origin',(0.237473777366883,0.199264159002827,5.75));
#35881=CARTESIAN_POINT('',(0.223573790202197,0.200036897433008,5.75));
#35882=CARTESIAN_POINT('Origin',(0.,0.,5.75));
#35883=CARTESIAN_POINT('',(0.241944156363363,0.240608283579327,5.75));
#35884=CARTESIAN_POINT('Origin',(0.241944156363363,0.240608283579327,5.25));
#35885=CARTESIAN_POINT('',(0.223573790202197,0.200036897433008,5.25));
#35886=CARTESIAN_POINT('',(0.223573790202197,0.200036897433008,5.475));
#35887=CARTESIAN_POINT('',(0.241944156363363,0.240608283579327,5.25));
#35888=CARTESIAN_POINT('Origin',(0.237473777366883,0.199264159002827,5.25));
#35889=CARTESIAN_POINT('Origin',(0.,0.,5.25));
#35890=CARTESIAN_POINT('Origin',(0.263113933820054,0.0957656401311872,5.25));
#35891=CARTESIAN_POINT('',(0.285023929972306,0.0936021332189709,5.25));
#35892=CARTESIAN_POINT('',(0.285023929972306,0.0936021332189709,5.75));
#35893=CARTESIAN_POINT('',(0.285023929972306,0.0936021332189709,5.475));
#35894=CARTESIAN_POINT('',(0.263113933820054,0.0957656401311872,5.25));
#35895=CARTESIAN_POINT('',(0.263113933820054,0.0957656401311872,5.25));
#35896=CARTESIAN_POINT('',(0.263113933820054,0.0957656401311872,5.75));
#35897=CARTESIAN_POINT('',(0.263113933820054,0.0957656401311872,5.25));
#35898=CARTESIAN_POINT('',(0.263113933820054,0.0957656401311872,5.75));
#35899=CARTESIAN_POINT('Origin',(0.291304712443632,0.106026244430957,5.75));
#35900=CARTESIAN_POINT('',(0.278507289184601,0.111506456633887,5.75));
#35901=CARTESIAN_POINT('Origin',(0.,0.,5.75));
#35902=CARTESIAN_POINT('',(0.309646018012069,0.143348053543252,5.75));
#35903=CARTESIAN_POINT('Origin',(0.309646018012069,0.143348053543252,5.25));
#35904=CARTESIAN_POINT('',(0.278507289184601,0.111506456633887,5.25));
#35905=CARTESIAN_POINT('',(0.278507289184601,0.111506456633887,5.475));
#35906=CARTESIAN_POINT('',(0.309646018012069,0.143348053543252,5.25));
#35907=CARTESIAN_POINT('Origin',(0.291304712443632,0.106026244430957,5.25));
#35908=CARTESIAN_POINT('Origin',(0.,0.,5.25));
#35909=CARTESIAN_POINT('Origin',(0.28,0.,5.25));
#35910=CARTESIAN_POINT('',(0.299848698761516,-0.00952669150468695,5.25));
#35911=CARTESIAN_POINT('',(0.299848698761516,-0.00952669150468695,5.75));
#35912=CARTESIAN_POINT('',(0.299848698761516,-0.00952669150468696,5.475));
#35913=CARTESIAN_POINT('',(0.28,0.,5.25));
#35914=CARTESIAN_POINT('',(0.28,0.,5.25));
#35915=CARTESIAN_POINT('',(0.28,0.,5.75));
#35916=CARTESIAN_POINT('',(0.28,0.,5.25));
#35917=CARTESIAN_POINT('',(0.28,0.,5.75));
#35918=CARTESIAN_POINT('Origin',(0.31,0.,5.75));
#35919=CARTESIAN_POINT('',(0.299848698761516,0.00952669150468695,5.75));
#35920=CARTESIAN_POINT('Origin',(0.,0.,5.75));
#35921=CARTESIAN_POINT('',(0.34,0.0287979326579064,5.75));
#35922=CARTESIAN_POINT('Origin',(0.34,0.0287979326579064,5.25));
#35923=CARTESIAN_POINT('',(0.299848698761516,0.00952669150468695,5.25));
#35924=CARTESIAN_POINT('',(0.299848698761516,0.00952669150468693,5.475));
#35925=CARTESIAN_POINT('',(0.34,0.0287979326579064,5.25));
#35926=CARTESIAN_POINT('Origin',(0.31,0.,5.25));
#35927=CARTESIAN_POINT('Origin',(0.,0.,5.25));
#35928=CARTESIAN_POINT('Origin',(0.,0.,-0.005));
#35929=CARTESIAN_POINT('',(-0.24,2.93915231795365E-17,0.));
#35930=CARTESIAN_POINT('Origin',(0.,0.,0.));
#35931=CARTESIAN_POINT('',(-0.24,-2.93915231795365E-17,0.04));
#35932=CARTESIAN_POINT('',(-0.24,-2.93915231795365E-17,-0.005));
#35933=CARTESIAN_POINT('Origin',(0.,0.,0.04));
#35934=CARTESIAN_POINT('Origin',(0.,0.,-0.005));
#35935=CARTESIAN_POINT('',(-0.28,-3.42901103761259E-17,0.));
#35936=CARTESIAN_POINT('Origin',(0.,0.,0.));
#35937=CARTESIAN_POINT('',(-0.28,-3.42901103761259E-17,0.04));
#35938=CARTESIAN_POINT('',(-0.28,-3.42901103761259E-17,-0.005));
#35939=CARTESIAN_POINT('Origin',(0.,0.,0.04));
#35940=CARTESIAN_POINT('Origin',(0.24,0.,0.04));
#35941=CARTESIAN_POINT('Origin',(0.38,0.,0.));
#35942=CARTESIAN_POINT('',(-0.38,-4.65365783675994E-17,-1.05818132034585E-16));
#35943=CARTESIAN_POINT('Origin',(0.,0.,0.));
#35944=CARTESIAN_POINT('Origin',(0.38,0.,0.));
#35945=CARTESIAN_POINT('Origin',(0.,0.,0.00999999999999979));
#35946=CARTESIAN_POINT('',(-0.4,-4.89858719658941E-17,0.0199999999999997));
#35947=CARTESIAN_POINT('Origin',(0.,0.,0.0199999999999996));
#35948=CARTESIAN_POINT('',(-0.39,-4.77612251667468E-17,0.00999999999999979));
#35949=CARTESIAN_POINT('Origin',(0.,0.,2.385));
#35950=CARTESIAN_POINT('',(-0.4,-4.89858719658941E-17,2.385));
#35951=CARTESIAN_POINT('Origin',(0.3,0.,5.15));
#35952=CARTESIAN_POINT('',(-0.3,-3.67394039744206E-17,5.15));
#35953=CARTESIAN_POINT('Origin',(0.,0.,5.15));
#35954=CARTESIAN_POINT('Origin',(0.,0.,5.475));
#35955=CARTESIAN_POINT('',(-0.3,-3.67394039744206E-17,5.8));
#35956=CARTESIAN_POINT('Origin',(0.,0.,5.8));
#35957=CARTESIAN_POINT('',(-0.3,-3.67394039744206E-17,5.475));
#35958=CARTESIAN_POINT('',(-0.3,-3.67394039744206E-17,5.475));
#35959=CARTESIAN_POINT('Origin',(0.18,0.,5.8));
#35960=CARTESIAN_POINT('',(-0.18,-2.20436423846524E-17,5.8));
#35961=CARTESIAN_POINT('Origin',(0.,0.,5.8));
#35962=CARTESIAN_POINT('Origin',(0.,0.,5.95));
#35963=CARTESIAN_POINT('',(-0.18,-2.20436423846524E-17,6.1));
#35964=CARTESIAN_POINT('Origin',(0.,0.,6.1));
#35965=CARTESIAN_POINT('',(-0.18,-2.20436423846524E-17,5.95));
#35966=CARTESIAN_POINT('Origin',(0.,0.,6.1));
#35967=CARTESIAN_POINT('',(0.,0.,0.));
#35968=CARTESIAN_POINT('Origin',(0.,0.,0.05));
#35969=CARTESIAN_POINT('',(-3.35,-4.10256677714363E-16,0.1));
#35970=CARTESIAN_POINT('Origin',(0.,0.,0.1));
#35971=CARTESIAN_POINT('',(-3.35,-4.10256677714363E-16,0.));
#35972=CARTESIAN_POINT('',(-3.35,-4.10256677714363E-16,0.05));
#35973=CARTESIAN_POINT('Origin',(0.,0.,0.));
#35974=CARTESIAN_POINT('Origin',(3.75,0.,0.));
#35975=CARTESIAN_POINT('',(-3.75,-4.59242549680257E-16,0.));
#35976=CARTESIAN_POINT('Origin',(0.,0.,0.));
#35977=CARTESIAN_POINT('Origin',(0.,0.,0.05));
#35978=CARTESIAN_POINT('',(-3.75,-4.59242549680257E-16,0.1));
#35979=CARTESIAN_POINT('Origin',(0.,0.,0.1));
#35980=CARTESIAN_POINT('',(-3.75,-4.59242549680257E-16,0.05));
#35981=CARTESIAN_POINT('Origin',(3.35,0.,0.1));
#35982=CARTESIAN_POINT('',(0.,0.,0.));
#35983=CARTESIAN_POINT('Origin',(4.6,0.,0.115));
#35984=CARTESIAN_POINT('',(4.345,3.12284933782576E-17,0.1));
#35985=CARTESIAN_POINT('Origin',(4.6,0.,0.1));
#35986=CARTESIAN_POINT('',(4.375,-2.75545529808155E-17,0.13));
#35987=CARTESIAN_POINT('',(4.36,2.93915231795366E-17,0.115));
#35988=CARTESIAN_POINT('Origin',(4.6,0.,0.13));
#35989=CARTESIAN_POINT('Origin',(4.6,0.,0.17));
#35990=CARTESIAN_POINT('',(4.375,-2.75545529808155E-17,0.27));
#35991=CARTESIAN_POINT('',(4.375,-2.75545529808155E-17,0.17));
#35992=CARTESIAN_POINT('',(4.825,-2.75545529808155E-17,0.27));
#35993=CARTESIAN_POINT('Origin',(4.6,0.,0.27));
#35994=CARTESIAN_POINT('Origin',(4.6,0.,0.27));
#35995=CARTESIAN_POINT('Origin',(4.55,0.,0.1));
#35996=CARTESIAN_POINT('',(3.8,-0.37,0.1));
#35997=CARTESIAN_POINT('',(5.25,-0.37,0.1));
#35998=CARTESIAN_POINT('',(4.,-0.37,0.1));
#35999=CARTESIAN_POINT('',(3.48,-0.05,0.1));
#36000=CARTESIAN_POINT('Origin',(3.8,-0.05,0.1));
#36001=CARTESIAN_POINT('',(3.48,0.05,0.1));
#36002=CARTESIAN_POINT('',(3.48,0.2,0.1));
#36003=CARTESIAN_POINT('',(3.8,0.37,0.1));
#36004=CARTESIAN_POINT('Origin',(3.8,0.05,0.1));
#36005=CARTESIAN_POINT('',(5.25,0.37,0.1));
#36006=CARTESIAN_POINT('',(5.1,0.37,0.1));
#36007=CARTESIAN_POINT('',(5.25,0.2,0.1));
#36008=CARTESIAN_POINT('Origin',(4.6,0.,0.285));
#36009=CARTESIAN_POINT('',(4.855,3.12284933782576E-17,0.3));
#36010=CARTESIAN_POINT('Origin',(4.6,0.,0.3));
#36011=CARTESIAN_POINT('',(4.84,2.93915231795366E-17,0.285));
#36012=CARTESIAN_POINT('Origin',(4.55,0.,0.3));
#36013=CARTESIAN_POINT('',(5.62,-0.2,0.3));
#36014=CARTESIAN_POINT('',(5.45,-0.37,0.3));
#36015=CARTESIAN_POINT('Origin',(5.45,-0.2,0.3));
#36016=CARTESIAN_POINT('',(5.62,0.2,0.3));
#36017=CARTESIAN_POINT('',(5.62,-0.2,0.3));
#36018=CARTESIAN_POINT('',(5.45,0.37,0.3));
#36019=CARTESIAN_POINT('Origin',(5.45,0.2,0.3));
#36020=CARTESIAN_POINT('',(3.8,0.37,0.3));
#36021=CARTESIAN_POINT('',(5.1,0.37,0.3));
#36022=CARTESIAN_POINT('',(3.48,0.05,0.3));
#36023=CARTESIAN_POINT('Origin',(3.8,0.05,0.3));
#36024=CARTESIAN_POINT('',(3.48,-0.05,0.3));
#36025=CARTESIAN_POINT('',(3.48,0.2,0.3));
#36026=CARTESIAN_POINT('',(3.8,-0.37,0.3));
#36027=CARTESIAN_POINT('Origin',(3.8,-0.05,0.3));
#36028=CARTESIAN_POINT('',(4.,-0.37,0.3));
#36029=CARTESIAN_POINT('Origin',(5.1,0.385,0.115));
#36030=CARTESIAN_POINT('',(5.25,0.4,0.13));
#36031=CARTESIAN_POINT('',(5.25,0.36,0.09));
#36032=CARTESIAN_POINT('',(3.8,0.4,0.13));
#36033=CARTESIAN_POINT('',(3.8,0.37,0.1));
#36034=CARTESIAN_POINT('',(5.1,0.4,0.13));
#36035=CARTESIAN_POINT('Origin',(3.8,0.05,0.115));
#36036=CARTESIAN_POINT('',(3.45,0.05,0.13));
#36037=CARTESIAN_POINT('',(3.48,0.05,0.1));
#36038=CARTESIAN_POINT('Origin',(3.8,0.05,0.13));
#36039=CARTESIAN_POINT('Origin',(3.465,0.2,0.115));
#36040=CARTESIAN_POINT('',(3.45,-0.05,0.13));
#36041=CARTESIAN_POINT('',(3.48,-0.05,0.1));
#36042=CARTESIAN_POINT('',(3.45,0.2,0.13));
#36043=CARTESIAN_POINT('Origin',(3.8,-0.05,0.115));
#36044=CARTESIAN_POINT('',(3.8,-0.4,0.13));
#36045=CARTESIAN_POINT('',(3.8,-0.37,0.1));
#36046=CARTESIAN_POINT('Origin',(3.8,-0.05,0.13));
#36047=CARTESIAN_POINT('Origin',(4.,-0.385,0.115));
#36048=CARTESIAN_POINT('',(5.25,-0.4,0.13));
#36049=CARTESIAN_POINT('',(5.25,-0.16,-0.11));
#36050=CARTESIAN_POINT('',(4.,-0.4,0.13));
#36051=CARTESIAN_POINT('Origin',(5.265,0.2,0.015));
#36052=CARTESIAN_POINT('',(5.25,-0.4,0.03));
#36053=CARTESIAN_POINT('',(5.25,0.4,0.03));
#36054=CARTESIAN_POINT('',(5.25,0.2,0.03));
#36055=CARTESIAN_POINT('',(5.28,0.37,0.));
#36056=CARTESIAN_POINT('',(5.25,0.4,0.03));
#36057=CARTESIAN_POINT('',(5.28,-0.37,0.));
#36058=CARTESIAN_POINT('',(5.28,0.2,0.));
#36059=CARTESIAN_POINT('',(5.28,-0.37,0.));
#36060=CARTESIAN_POINT('Origin',(4.45,-0.385,0.015));
#36061=CARTESIAN_POINT('',(5.45,-0.37,0.));
#36062=CARTESIAN_POINT('',(4.45,-0.37,0.));
#36063=CARTESIAN_POINT('',(5.45,-0.4,0.03));
#36064=CARTESIAN_POINT('',(5.45,-0.37,0.));
#36065=CARTESIAN_POINT('',(4.45,-0.4,0.03));
#36066=CARTESIAN_POINT('Origin',(5.45,-0.2,0.015));
#36067=CARTESIAN_POINT('',(5.62,-0.2,0.));
#36068=CARTESIAN_POINT('',(5.65,-0.2,0.03));
#36069=CARTESIAN_POINT('',(5.62,-0.2,0.));
#36070=CARTESIAN_POINT('Origin',(5.45,-0.2,0.03));
#36071=CARTESIAN_POINT('Origin',(5.45,-0.2,0.));
#36072=CARTESIAN_POINT('Origin',(5.635,-0.2,0.015));
#36073=CARTESIAN_POINT('',(5.62,0.2,0.));
#36074=CARTESIAN_POINT('',(5.65,0.2,0.03));
#36075=CARTESIAN_POINT('',(5.62,0.2,0.));
#36076=CARTESIAN_POINT('',(5.65,-0.2,0.03));
#36077=CARTESIAN_POINT('',(5.62,-0.2,0.));
#36078=CARTESIAN_POINT('Origin',(5.45,0.2,0.015));
#36079=CARTESIAN_POINT('',(5.45,0.37,0.));
#36080=CARTESIAN_POINT('',(5.45,0.4,0.03));
#36081=CARTESIAN_POINT('',(5.45,0.37,0.));
#36082=CARTESIAN_POINT('Origin',(5.45,0.2,0.03));
#36083=CARTESIAN_POINT('Origin',(5.45,0.2,0.));
#36084=CARTESIAN_POINT('Origin',(5.55,0.385,0.015));
#36085=CARTESIAN_POINT('',(5.55,0.4,0.03));
#36086=CARTESIAN_POINT('',(5.55,0.37,0.));
#36087=CARTESIAN_POINT('Origin',(5.45,0.2,0.1));
#36088=CARTESIAN_POINT('',(5.45,0.4,0.27));
#36089=CARTESIAN_POINT('',(5.45,0.4,0.1));
#36090=CARTESIAN_POINT('',(5.65,0.2,0.27));
#36091=CARTESIAN_POINT('Origin',(5.45,0.2,0.27));
#36092=CARTESIAN_POINT('',(5.65,0.2,0.1));
#36093=CARTESIAN_POINT('Origin',(5.65,0.4,0.1));
#36094=CARTESIAN_POINT('',(3.8,0.4,0.27));
#36095=CARTESIAN_POINT('',(3.8,0.4,0.1));
#36096=CARTESIAN_POINT('',(5.1,0.4,0.27));
#36097=CARTESIAN_POINT('',(5.25,0.4,0.));
#36098=CARTESIAN_POINT('Origin',(5.25,0.4,0.));
#36099=CARTESIAN_POINT('',(5.25,-0.4,0.));
#36100=CARTESIAN_POINT('Origin',(5.45,0.,0.));
#36101=CARTESIAN_POINT('Origin',(5.45,-0.2,0.285));
#36102=CARTESIAN_POINT('',(5.45,-0.4,0.27));
#36103=CARTESIAN_POINT('',(5.45,-0.37,0.3));
#36104=CARTESIAN_POINT('',(5.65,-0.2,0.27));
#36105=CARTESIAN_POINT('Origin',(5.45,-0.2,0.27));
#36106=CARTESIAN_POINT('',(5.65,-0.2,0.27));
#36107=CARTESIAN_POINT('Origin',(4.,-0.385,0.285));
#36108=CARTESIAN_POINT('',(3.8,-0.4,0.27));
#36109=CARTESIAN_POINT('',(3.8,-0.37,0.3));
#36110=CARTESIAN_POINT('',(4.,-0.4,0.27));
#36111=CARTESIAN_POINT('Origin',(3.8,-0.05,0.285));
#36112=CARTESIAN_POINT('',(3.45,-0.05,0.27));
#36113=CARTESIAN_POINT('',(3.48,-0.05,0.3));
#36114=CARTESIAN_POINT('Origin',(3.8,-0.05,0.27));
#36115=CARTESIAN_POINT('Origin',(3.465,0.2,0.285));
#36116=CARTESIAN_POINT('',(3.45,0.05,0.27));
#36117=CARTESIAN_POINT('',(3.48,0.05,0.3));
#36118=CARTESIAN_POINT('',(3.45,0.2,0.27));
#36119=CARTESIAN_POINT('Origin',(3.8,0.05,0.285));
#36120=CARTESIAN_POINT('',(3.8,0.37,0.3));
#36121=CARTESIAN_POINT('Origin',(3.8,0.05,0.27));
#36122=CARTESIAN_POINT('Origin',(5.1,0.385,0.285));
#36123=CARTESIAN_POINT('',(5.45,0.37,0.3));
#36124=CARTESIAN_POINT('Origin',(5.45,0.2,0.285));
#36125=CARTESIAN_POINT('',(5.62,0.2,0.3));
#36126=CARTESIAN_POINT('Origin',(5.635,-0.2,0.285));
#36127=CARTESIAN_POINT('',(5.65,-0.2,0.27));
#36128=CARTESIAN_POINT('Origin',(5.65,-0.4,0.1));
#36129=CARTESIAN_POINT('',(5.65,-0.2,0.1));
#36130=CARTESIAN_POINT('Origin',(5.45,-0.2,0.1));
#36131=CARTESIAN_POINT('',(5.45,-0.4,0.1));
#36132=CARTESIAN_POINT('Origin',(3.45,-0.4,0.1));
#36133=CARTESIAN_POINT('',(3.8,-0.4,0.1));
#36134=CARTESIAN_POINT('Origin',(3.8,-0.05,0.1));
#36135=CARTESIAN_POINT('',(3.45,-0.05,0.1));
#36136=CARTESIAN_POINT('Origin',(3.45,0.4,0.1));
#36137=CARTESIAN_POINT('',(3.45,0.05,0.1));
#36138=CARTESIAN_POINT('Origin',(3.8,0.05,0.1));
#36139=CARTESIAN_POINT('',(0.,0.,0.));
#36140=CARTESIAN_POINT('Origin',(0.,0.,0.04));
#36141=CARTESIAN_POINT('',(-0.21,-2.57175827820944E-17,0.06));
#36142=CARTESIAN_POINT('Origin',(0.,0.,0.06));
#36143=CARTESIAN_POINT('',(-0.21,-2.57175827820944E-17,0.02));
#36144=CARTESIAN_POINT('',(-0.21,-2.57175827820944E-17,0.04));
#36145=CARTESIAN_POINT('Origin',(0.,0.,0.02));
#36146=CARTESIAN_POINT('Origin',(0.,0.,0.01));
#36147=CARTESIAN_POINT('',(-0.4,-4.89858719658941E-17,3.46944695195361E-18));
#36148=CARTESIAN_POINT('',(-0.305,-3.73517273739943E-17,0.01));
#36149=CARTESIAN_POINT('Origin',(0.,0.,0.));
#36150=CARTESIAN_POINT('Origin',(0.,0.,0.02));
#36151=CARTESIAN_POINT('',(-0.4,-4.89858719658941E-17,0.04));
#36152=CARTESIAN_POINT('Origin',(0.,0.,0.04));
#36153=CARTESIAN_POINT('',(-0.4,-4.89858719658941E-17,0.02));
#36154=CARTESIAN_POINT('Origin',(0.,0.,0.05));
#36155=CARTESIAN_POINT('',(-0.305,-3.73517273739943E-17,0.05));
#36156=CARTESIAN_POINT('',(0.,0.,0.));
#36157=CARTESIAN_POINT('Origin',(0.,0.,-0.56));
#36158=CARTESIAN_POINT('',(-0.195084575036282,1.57151725016375E-5,-0.962013030787577));
#36159=CARTESIAN_POINT('',(-0.195110174310067,3.211721741748E-6,-0.972186969212424));
#36160=CARTESIAN_POINT('',(-0.1954,-2.39295984553393E-17,-0.56));
#36161=CARTESIAN_POINT('',(0.188713086871761,-0.0519137165493658,-1.));
#36162=CARTESIAN_POINT('Ctrl Pts',(-0.195084575036282,1.57151725016375E-5,
-0.962013030787577));
#36163=CARTESIAN_POINT('Ctrl Pts',(-0.195109875732101,0.0316848016664486,
-0.963811747031453));
#36164=CARTESIAN_POINT('Ctrl Pts',(-0.187839688942379,0.0633440313364852,
-0.96561046327533));
#36165=CARTESIAN_POINT('Ctrl Pts',(-0.173214336083063,0.0911354430469698,
-0.967409179519207));
#36166=CARTESIAN_POINT('Ctrl Pts',(-0.143076407955131,0.148404185672271,
-0.97111572809974));
#36167=CARTESIAN_POINT('Ctrl Pts',(-0.0817059931899262,0.189248884082378,
-0.974822276680274));
#36168=CARTESIAN_POINT('Ctrl Pts',(-0.0172563726780756,0.194958105016696,
-0.978528825260807));
#36169=CARTESIAN_POINT('Ctrl Pts',(0.0471932478337753,0.200667325951015,
-0.98223537384134));
#36170=CARTESIAN_POINT('Ctrl Pts',(0.114722074092272,0.171241069409545,
-0.985941922421872));
#36171=CARTESIAN_POINT('Ctrl Pts',(0.154471393616461,0.120160647611379,
-0.989648471002406));
#36172=CARTESIAN_POINT('Ctrl Pts',(0.191474931611372,0.0726087309639927,
-0.993098980668271));
#36173=CARTESIAN_POINT('Ctrl Pts',(0.204404282404944,0.00629095093881454,
-0.996549490334136));
#36174=CARTESIAN_POINT('Ctrl Pts',(0.188715001522267,-0.0519146961985303,
-1.));
#36175=CARTESIAN_POINT('',(-0.1954,-2.39295984553393E-17,-1.));
#36176=CARTESIAN_POINT('Origin',(0.,0.,-1.));
#36177=CARTESIAN_POINT('',(-0.1954,-2.39295984553393E-17,-1.1246));
#36178=CARTESIAN_POINT('',(-0.1954,-2.39295984553393E-17,-0.56));
#36179=CARTESIAN_POINT('Origin',(0.,0.,-1.1246));
#36180=CARTESIAN_POINT('',(0.156132246633334,0.117489921104866,-1.));
#36181=CARTESIAN_POINT('Origin',(0.,0.,-1.));
#36182=CARTESIAN_POINT('Ctrl Pts',(0.156132246633334,0.117489921104866,
-1.));
#36183=CARTESIAN_POINT('Ctrl Pts',(0.117043464717142,0.169434966955124,
-0.996293451419467));
#36184=CARTESIAN_POINT('Ctrl Pts',(0.050333107650634,0.199889556663511,
-0.992586902838933));
#36185=CARTESIAN_POINT('Ctrl Pts',(-0.0141001197016129,0.195197543652393,
-0.9888803542584));
#36186=CARTESIAN_POINT('Ctrl Pts',(-0.0785333470538611,0.190505530641275,
-0.985173805677867));
#36187=CARTESIAN_POINT('Ctrl Pts',(-0.140689444691848,0.15066691491065,
-0.981467257097333));
#36188=CARTESIAN_POINT('Ctrl Pts',(-0.17177246279413,0.0938911568835147,
-0.9777607085168));
#36189=CARTESIAN_POINT('Ctrl Pts',(-0.187352872792911,0.06543222200327,
-0.975902795415341));
#36190=CARTESIAN_POINT('Ctrl Pts',(-0.19512607572876,0.0327177778867662,
-0.974044882313883));
#36191=CARTESIAN_POINT('Ctrl Pts',(-0.195110174310067,3.211721741748E-6,
-0.972186969212424));
#36192=CARTESIAN_POINT('Origin',(0.,0.,-0.56));
#36193=CARTESIAN_POINT('',(-0.195426264375126,-0.000177548476699763,-0.892013030787577));
#36194=CARTESIAN_POINT('',(-0.195457760643607,-0.000174238830481377,-0.902186969212424));
#36195=CARTESIAN_POINT('',(-0.1954,-2.39295984553393E-17,-0.56));
#36196=CARTESIAN_POINT('Ctrl Pts',(-0.195426264375126,-0.000177548476699763,
-0.892013030787577));
#36197=CARTESIAN_POINT('Ctrl Pts',(-0.194957410957457,0.050526042153958,
-0.894905788881586));
#36198=CARTESIAN_POINT('Ctrl Pts',(-0.174765431648993,0.101560768688629,
-0.897798546975596));
#36199=CARTESIAN_POINT('Ctrl Pts',(-0.139284034569977,0.137501909669616,
-0.900691305069606));
#36200=CARTESIAN_POINT('Ctrl Pts',(-0.09382101356905,0.183554009691976,
-0.904397853650139));
#36201=CARTESIAN_POINT('Ctrl Pts',(-0.0232561208383973,0.204825751547922,
-0.908104402230672));
#36202=CARTESIAN_POINT('Ctrl Pts',(0.0400842191953776,0.191572593489572,
-0.911810950811206));
#36203=CARTESIAN_POINT('Ctrl Pts',(0.103424559229153,0.178319435431222,
-0.915517499391739));
#36204=CARTESIAN_POINT('Ctrl Pts',(0.159540346566049,0.130541377458575,
-0.919224047972273));
#36205=CARTESIAN_POINT('Ctrl Pts',(0.182726664407761,0.0701254468485091,
-0.922930596552806));
#36206=CARTESIAN_POINT('Ctrl Pts',(0.205912982249472,0.00970951623844284,
-0.92663714513334));
#36207=CARTESIAN_POINT('Ctrl Pts',(0.196169830595998,-0.063344287009043,
-0.930343693713872));
#36208=CARTESIAN_POINT('Ctrl Pts',(0.157957512983411,-0.115570247816891,
-0.934050242294406));
#36209=CARTESIAN_POINT('Ctrl Pts',(0.119745195370824,-0.167796208624739,
-0.937756790874939));
#36210=CARTESIAN_POINT('Ctrl Pts',(0.0530637117991234,-0.199194326992949,
-0.941463339455473));
#36211=CARTESIAN_POINT('Ctrl Pts',(-0.0115345925566828,-0.195381124160082,
-0.945169888036006));
#36212=CARTESIAN_POINT('Ctrl Pts',(-0.0761328969124891,-0.191567921327216,
-0.94887643661654));
#36213=CARTESIAN_POINT('Ctrl Pts',(-0.138648022052401,-0.152543397293271,
-0.952582985197073));
#36214=CARTESIAN_POINT('Ctrl Pts',(-0.170452863877028,-0.0961847418560505,
-0.956289533777606));
#36215=CARTESIAN_POINT('Ctrl Pts',(-0.18682343190734,-0.0671758504419905,
-0.958197366114263));
#36216=CARTESIAN_POINT('Ctrl Pts',(-0.195057739516345,-0.0335745231384176,
-0.96010519845092));
#36217=CARTESIAN_POINT('Ctrl Pts',(-0.195084575036282,1.57151725016375E-5,
-0.962013030787577));
#36218=CARTESIAN_POINT('Ctrl Pts',(-0.195110174310067,3.211721741748E-6,
-0.972186969212424));
#36219=CARTESIAN_POINT('Ctrl Pts',(-0.195094352296248,-0.0325479919097508,
-0.970338333733349));
#36220=CARTESIAN_POINT('Ctrl Pts',(-0.187367022603641,-0.0650993163738915,
-0.968489698254274));
#36221=CARTESIAN_POINT('Ctrl Pts',(-0.171946018101075,-0.0934588054226745,
-0.9666410627752));
#36222=CARTESIAN_POINT('Ctrl Pts',(-0.14102661673916,-0.150320109378084,
-0.962934514194666));
#36223=CARTESIAN_POINT('Ctrl Pts',(-0.0791778754487514,-0.190329816965257,
-0.959227965614133));
#36224=CARTESIAN_POINT('Ctrl Pts',(-0.0146572328544997,-0.195170717064559,
-0.9555214170336));
#36225=CARTESIAN_POINT('Ctrl Pts',(0.049863409739752,-0.200011617163861,
-0.951814868453067));
#36226=CARTESIAN_POINT('Ctrl Pts',(0.117055953637847,-0.169683709775292,
-0.948108319872533));
#36227=CARTESIAN_POINT('Ctrl Pts',(0.156100413855611,-0.11807427426149,
-0.944401771292));
#36228=CARTESIAN_POINT('Ctrl Pts',(0.195144874073376,-0.0664648387476884,
-0.940695222711466));
#36229=CARTESIAN_POINT('Ctrl Pts',(0.206041250610809,0.00642612489134668,
-0.936988674130933));
#36230=CARTESIAN_POINT('Ctrl Pts',(0.183818523921417,0.0672043779064316,
-0.933282125550399));
#36231=CARTESIAN_POINT('Ctrl Pts',(0.161595797232025,0.127982630921516,
-0.929575576969866));
#36232=CARTESIAN_POINT('Ctrl Pts',(0.106253967315808,0.176648173312651,
-0.925869028389332));
#36233=CARTESIAN_POINT('Ctrl Pts',(0.0431341771381354,0.190909062306829,
-0.922162479808799));
#36234=CARTESIAN_POINT('Ctrl Pts',(-0.0199856130395371,0.205169951301007,
-0.918455931228266));
#36235=CARTESIAN_POINT('Ctrl Pts',(-0.0908833634786639,0.185026186898227,
-0.914749382647733));
#36236=CARTESIAN_POINT('Ctrl Pts',(-0.137075323273913,0.139704726559351,
-0.9110428340672));
#36237=CARTESIAN_POINT('Ctrl Pts',(-0.173863343578693,0.103609986033525,
-0.908090879115608));
#36238=CARTESIAN_POINT('Ctrl Pts',(-0.194981009616801,0.0515455718136115,
-0.905138924164016));
#36239=CARTESIAN_POINT('Ctrl Pts',(-0.195457760643607,-0.000174238830481377,
-0.902186969212424));
#36240=CARTESIAN_POINT('Origin',(0.,0.,-0.56));
#36241=CARTESIAN_POINT('',(-0.195673584877587,8.71017904331833E-5,-0.822013030787576));
#36242=CARTESIAN_POINT('',(-0.195653454845991,0.000103118138519916,-0.832186969212424));
#36243=CARTESIAN_POINT('',(-0.1954,-2.39295984553393E-17,-0.56));
#36244=CARTESIAN_POINT('Ctrl Pts',(-0.195673584877587,8.71017904331833E-5,
-0.822013030787576));
#36245=CARTESIAN_POINT('Ctrl Pts',(-0.195700838558998,0.00498315558351734,
-0.822293282151186));
#36246=CARTESIAN_POINT('Ctrl Pts',(-0.195533017114237,0.00987731022659859,
-0.822573533514795));
#36247=CARTESIAN_POINT('Ctrl Pts',(-0.195164122119264,0.0147562617970676,
-0.822853784878405));
#36248=CARTESIAN_POINT('Ctrl Pts',(-0.190285190568779,0.0792843011439578,
-0.826560333458938));
#36249=CARTESIAN_POINT('Ctrl Pts',(-0.150234112753965,0.141152991744968,
-0.830266882039473));
#36250=CARTESIAN_POINT('Ctrl Pts',(-0.0933581745971609,0.172020446737902,
-0.833973430620006));
#36251=CARTESIAN_POINT('Ctrl Pts',(-0.0364822364403571,0.202887901730835,
-0.83767997920054));
#36252=CARTESIAN_POINT('Ctrl Pts',(0.0372185620584375,0.202754121115692,
-0.841386527781072));
#36253=CARTESIAN_POINT('Ctrl Pts',(0.0939820585112729,0.171680389196942,
-0.845093076361605));
#36254=CARTESIAN_POINT('Ctrl Pts',(0.150745554964109,0.140606657278192,
-0.848799624942138));
#36255=CARTESIAN_POINT('Ctrl Pts',(0.190571749370985,0.0785929740558366,
-0.852506173522672));
#36256=CARTESIAN_POINT('Ctrl Pts',(0.195216398313037,0.0140476477414276,
-0.856212722103206));
#36257=CARTESIAN_POINT('Ctrl Pts',(0.199861047255089,-0.0504976785729813,
-0.859919270683739));
#36258=CARTESIAN_POINT('Ctrl Pts',(0.169324150732317,-0.117574647979443,
-0.863625819264272));
#36259=CARTESIAN_POINT('Ctrl Pts',(0.117594518889292,-0.156455475350819,
-0.867332367844806));
#36260=CARTESIAN_POINT('Ctrl Pts',(0.0658648870462679,-0.195336302722196,
-0.871038916425339));
#36261=CARTESIAN_POINT('Ctrl Pts',(-0.00705748011700841,-0.206020988058488,
-0.874745465005873));
#36262=CARTESIAN_POINT('Ctrl Pts',(-0.0677669148374835,-0.183614902949219,
-0.878452013586406));
#36263=CARTESIAN_POINT('Ctrl Pts',(-0.128476349557959,-0.161208817839951,
-0.882158562166939));
#36264=CARTESIAN_POINT('Ctrl Pts',(-0.176972851835633,-0.105711962285121,
-0.885865110747472));
#36265=CARTESIAN_POINT('Ctrl Pts',(-0.19104052833887,-0.0425473054133194,
-0.889571659328006));
#36266=CARTESIAN_POINT('Ctrl Pts',(-0.194129154066305,-0.0286792025866717,
-0.890385449814529));
#36267=CARTESIAN_POINT('Ctrl Pts',(-0.195558162182849,-0.0144414787283386,
-0.891199240301053));
#36268=CARTESIAN_POINT('Ctrl Pts',(-0.195426264375126,-0.000177548476699763,
-0.892013030787577));
#36269=CARTESIAN_POINT('Ctrl Pts',(-0.195457760643607,-0.000174238830481377,
-0.902186969212424));
#36270=CARTESIAN_POINT('Ctrl Pts',(-0.195579630148162,-0.0133951179570571,
-0.901432375583482));
#36271=CARTESIAN_POINT('Ctrl Pts',(-0.194352736283242,-0.0265934792504939,
-0.900677781954541));
#36272=CARTESIAN_POINT('Ctrl Pts',(-0.191694052762859,-0.0394968154586175,
-0.899923188325599));
#36273=CARTESIAN_POINT('Ctrl Pts',(-0.178634653305186,-0.102877740862738,
-0.896216639745066));
#36274=CARTESIAN_POINT('Ctrl Pts',(-0.13102968523847,-0.159140435396007,
-0.892510091164533));
#36275=CARTESIAN_POINT('Ctrl Pts',(-0.0706852958104853,-0.182511338506239,
-0.888803542584));
#36276=CARTESIAN_POINT('Ctrl Pts',(-0.0103409063825001,-0.20588224161647,
-0.885096994003466));
#36277=CARTESIAN_POINT('Ctrl Pts',(0.0627429044067541,-0.196361353303663,
-0.881390445422932));
#36278=CARTESIAN_POINT('Ctrl Pts',(0.115085809889437,-0.15831004487468,
-0.877683896842399));
#36279=CARTESIAN_POINT('Ctrl Pts',(0.167428715372121,-0.120258736445697,
-0.873977348261865));
#36280=CARTESIAN_POINT('Ctrl Pts',(0.199030715548233,-0.0536770079005367,
-0.870270799681332));
#36281=CARTESIAN_POINT('Ctrl Pts',(0.195415447752892,0.0109341586965677,
-0.866564251100799));
#36282=CARTESIAN_POINT('Ctrl Pts',(0.191800179957551,0.0755453252936721,
-0.862857702520266));
#36283=CARTESIAN_POINT('Ctrl Pts',(0.152967644190756,0.138185929942721,
-0.859151153939732));
#36284=CARTESIAN_POINT('Ctrl Pts',(0.0967066977677326,0.170160507747372,
-0.855444605359199));
#36285=CARTESIAN_POINT('Ctrl Pts',(0.0404457513447093,0.202135085552022,
-0.851738056778666));
#36286=CARTESIAN_POINT('Ctrl Pts',(-0.0332436057345425,0.203443636512275,
-0.848031508198133));
#36287=CARTESIAN_POINT('Ctrl Pts',(-0.0906043506555229,0.173486699003936,
-0.844324959617599));
#36288=CARTESIAN_POINT('Ctrl Pts',(-0.147965095576503,0.143529761495597,
-0.840618411037066));
#36289=CARTESIAN_POINT('Ctrl Pts',(-0.188997228339212,0.0823073355186673,
-0.836911862456532));
#36290=CARTESIAN_POINT('Ctrl Pts',(-0.194904097710687,0.0178652652725652,
-0.833205313875999));
#36291=CARTESIAN_POINT('Ctrl Pts',(-0.195445052795288,0.0119636169764026,
-0.832865865654807));
#36292=CARTESIAN_POINT('Ctrl Pts',(-0.195691411591684,0.00603496545921146,
-0.832526417433615));
#36293=CARTESIAN_POINT('Ctrl Pts',(-0.195653454845991,0.000103118138519916,
-0.832186969212424));
#36294=CARTESIAN_POINT('Origin',(0.,0.,-0.56));
#36295=CARTESIAN_POINT('',(-0.195164384848501,0.000125606292110517,-0.752013030787577));
#36296=CARTESIAN_POINT('',(-0.195145082735841,0.000112707534856574,-0.762186969212424));
#36297=CARTESIAN_POINT('',(-0.1954,-2.39295984553393E-17,-0.56));
#36298=CARTESIAN_POINT('Ctrl Pts',(-0.195164384848501,0.000125606292110517,
-0.752013030787577));
#36299=CARTESIAN_POINT('Ctrl Pts',(-0.195306581362487,0.0242959090730286,
-0.753387324001319));
#36300=CARTESIAN_POINT('Ctrl Pts',(-0.191149350064068,0.0484190333677505,
-0.754761617215062));
#36301=CARTESIAN_POINT('Ctrl Pts',(-0.182471342534317,0.0707883572077772,
-0.756135910428805));
#36302=CARTESIAN_POINT('Ctrl Pts',(-0.15906625243447,0.131119722230631,
-0.759842459009338));
#36303=CARTESIAN_POINT('Ctrl Pts',(-0.102776483832904,0.178693728526212,
-0.763549007589872));
#36304=CARTESIAN_POINT('Ctrl Pts',(-0.0393882338062579,0.191716846977238,
-0.767255556170405));
#36305=CARTESIAN_POINT('Ctrl Pts',(0.0240000162203877,0.204739965428263,
-0.770962104750938));
#36306=CARTESIAN_POINT('Ctrl Pts',(0.0944867476721127,0.183212196034733,
-0.774668653331471));
#36307=CARTESIAN_POINT('Ctrl Pts',(0.139782170988598,0.136995354217524,
-0.778375201912005));
#36308=CARTESIAN_POINT('Ctrl Pts',(0.185077594305083,0.0907785124003164,
-0.782081750492538));
#36309=CARTESIAN_POINT('Ctrl Pts',(0.205181709486329,0.0198725981594313,
-0.785788299073072));
#36310=CARTESIAN_POINT('Ctrl Pts',(0.190884874109968,-0.0432405727492172,
-0.789494847653606));
#36311=CARTESIAN_POINT('Ctrl Pts',(0.176588038733607,-0.106353743657866,
-0.793201396234139));
#36312=CARTESIAN_POINT('Ctrl Pts',(0.127890252799637,-0.161674171234278,
-0.796907944814671));
#36313=CARTESIAN_POINT('Ctrl Pts',(0.06709984464803,-0.183859710843263,
-0.800614493395204));
#36314=CARTESIAN_POINT('Ctrl Pts',(0.00630943649642266,-0.206045250452247,
-0.804321041975738));
#36315=CARTESIAN_POINT('Ctrl Pts',(-0.0665735938728228,-0.195095902093804,
-0.808027590556272));
#36316=CARTESIAN_POINT('Ctrl Pts',(-0.118161716414366,-0.156027533868197,
-0.811734139136806));
#36317=CARTESIAN_POINT('Ctrl Pts',(-0.165849271791013,-0.119913116799936,
-0.81516043635373));
#36318=CARTESIAN_POINT('Ctrl Pts',(-0.195340386810088,-0.0597710743450758,
-0.818586733570653));
#36319=CARTESIAN_POINT('Ctrl Pts',(-0.195673584877587,8.71017904331833E-5,
-0.822013030787576));
#36320=CARTESIAN_POINT('Ctrl Pts',(-0.195653454845991,0.000103118138519916,
-0.832186969212424));
#36321=CARTESIAN_POINT('Ctrl Pts',(-0.19527694919923,-0.0587368580291033,
-0.828819868853082));
#36322=CARTESIAN_POINT('Ctrl Pts',(-0.166925729961675,-0.117891279502673,
-0.825452768493741));
#36323=CARTESIAN_POINT('Ctrl Pts',(-0.120633753452604,-0.154124226937434,
-0.822085668134399));
#36324=CARTESIAN_POINT('Ctrl Pts',(-0.0696749338428048,-0.194009934386057,
-0.818379119553866));
#36325=CARTESIAN_POINT('Ctrl Pts',(0.00302431135703297,-0.206119634768027,
-0.814672570973332));
#36326=CARTESIAN_POINT('Ctrl Pts',(0.0641606288751104,-0.184905903107813,
-0.810966022392799));
#36327=CARTESIAN_POINT('Ctrl Pts',(0.125296946393188,-0.163692171447599,
-0.807259473812265));
#36328=CARTESIAN_POINT('Ctrl Pts',(0.174870336229504,-0.109155007745201,
-0.803552925231732));
#36329=CARTESIAN_POINT('Ctrl Pts',(0.19017136590337,-0.0462777468575458,
-0.799846376651198));
#36330=CARTESIAN_POINT('Ctrl Pts',(0.205472395577236,0.0165995140301098,
-0.796139828070665));
#36331=CARTESIAN_POINT('Ctrl Pts',(0.186501065088651,0.0878168721030228,
-0.792433279490132));
#36332=CARTESIAN_POINT('Ctrl Pts',(0.141948087059648,0.134749840714092,
-0.788726730909599));
#36333=CARTESIAN_POINT('Ctrl Pts',(0.0973951090306438,0.181682809325161,
-0.785020182329065));
#36334=CARTESIAN_POINT('Ctrl Pts',(0.0272604834612217,0.204331388474385,
-0.781313633748532));
#36335=CARTESIAN_POINT('Ctrl Pts',(-0.0363272967462341,0.192320322314275,
-0.777607085167998));
#36336=CARTESIAN_POINT('Ctrl Pts',(-0.0999150769536897,0.180309256154165,
-0.773900536587465));
#36337=CARTESIAN_POINT('Ctrl Pts',(-0.156956011799179,0.133638544684719,
-0.770193988006932));
#36338=CARTESIAN_POINT('Ctrl Pts',(-0.181319798015859,0.0736879202010541,
-0.766487439426399));
#36339=CARTESIAN_POINT('Ctrl Pts',(-0.190742376698605,0.050502300722489,
-0.765053949355074));
#36340=CARTESIAN_POINT('Ctrl Pts',(-0.195277372458642,0.025330379538085,
-0.763620459283749));
#36341=CARTESIAN_POINT('Ctrl Pts',(-0.195145082735841,0.000112707534856574,
-0.762186969212424));
#36342=CARTESIAN_POINT('Origin',(0.,0.,-0.56));
#36343=CARTESIAN_POINT('',(-0.195216518518634,-0.000150737487880678,-0.682013030787577));
#36344=CARTESIAN_POINT('',(-0.195242183955992,-0.000159443835737465,-0.692186969212424));
#36345=CARTESIAN_POINT('',(-0.1954,-2.39295984553393E-17,-0.56));
#36346=CARTESIAN_POINT('Ctrl Pts',(-0.195216518518634,-0.000150737487880678,
-0.682013030787577));
#36347=CARTESIAN_POINT('Ctrl Pts',(-0.194904732781107,0.0432318296131434,
-0.684481365851453));
#36348=CARTESIAN_POINT('Ctrl Pts',(-0.180636578142957,0.0868005498567561,
-0.686949700915328));
#36349=CARTESIAN_POINT('Ctrl Pts',(-0.154055925496942,0.120720976604095,
-0.689418035979204));
#36350=CARTESIAN_POINT('Ctrl Pts',(-0.114141376707916,0.171657217575372,
-0.693124584559738));
#36351=CARTESIAN_POINT('Ctrl Pts',(-0.0464631280272487,0.200837327099895,
-0.696831133140271));
#36352=CARTESIAN_POINT('Ctrl Pts',(0.0179755900401639,0.1948939725487,-0.700537681720805));
#36353=CARTESIAN_POINT('Ctrl Pts',(0.0824143081075773,0.188950617997505,
-0.704244230301338));
#36354=CARTESIAN_POINT('Ctrl Pts',(0.143613495561735,0.14788379937059,-0.707950778881872));
#36355=CARTESIAN_POINT('Ctrl Pts',(0.173537963060344,0.0905061199632647,
-0.711657327462405));
#36356=CARTESIAN_POINT('Ctrl Pts',(0.203462430558953,0.0331284405559403,
-0.715363876042938));
#36357=CARTESIAN_POINT('Ctrl Pts',(0.202112178102014,-0.0405600996317941,
-0.719070424623471));
#36358=CARTESIAN_POINT('Ctrl Pts',(0.17010575285896,-0.0968029711114258,
-0.722776973204005));
#36359=CARTESIAN_POINT('Ctrl Pts',(0.138099327615907,-0.153045842591058,
-0.726483521784538));
#36360=CARTESIAN_POINT('Ctrl Pts',(0.0754367295867393,-0.191843045362587,
-0.730190070365071));
#36361=CARTESIAN_POINT('Ctrl Pts',(0.0108235326741567,-0.195421681278553,
-0.733896618945605));
#36362=CARTESIAN_POINT('Ctrl Pts',(-0.0537896642384258,-0.199000317194519,
-0.737603167526138));
#36363=CARTESIAN_POINT('Ctrl Pts',(-0.120353460034423,-0.167360386254922,
-0.741309716106672));
#36364=CARTESIAN_POINT('Ctrl Pts',(-0.158375152133358,-0.114996058910061,
-0.745016264687205));
#36365=CARTESIAN_POINT('Ctrl Pts',(-0.182299375309043,-0.082047082031722,
-0.747348520053995));
#36366=CARTESIAN_POINT('Ctrl Pts',(-0.194923069109207,-0.0408928007072448,
-0.749680775420786));
#36367=CARTESIAN_POINT('Ctrl Pts',(-0.195164384848501,0.000125606292110517,
-0.752013030787577));
#36368=CARTESIAN_POINT('Ctrl Pts',(-0.195145082735841,0.000112707534856574,
-0.762186969212424));
#36369=CARTESIAN_POINT('Ctrl Pts',(-0.194935313386121,-0.0398744853142615,
-0.759913910703216));
#36370=CARTESIAN_POINT('Ctrl Pts',(-0.182990189434058,-0.079976713355511,
-0.757640852194007));
#36371=CARTESIAN_POINT('Ctrl Pts',(-0.160188039888451,-0.11245697275395,
-0.755367793684799));
#36372=CARTESIAN_POINT('Ctrl Pts',(-0.12300585795649,-0.165420703727406,
-0.751661245104265));
#36373=CARTESIAN_POINT('Ctrl Pts',(-0.0569548565046961,-0.198117628176434,
-0.747954696523731));
#36374=CARTESIAN_POINT('Ctrl Pts',(0.00770717133859991,-0.195569369605572,
-0.744248147943198));
#36375=CARTESIAN_POINT('Ctrl Pts',(0.0723691991818959,-0.19302111103471,
-0.740541599362665));
#36376=CARTESIAN_POINT('Ctrl Pts',(0.135642253416694,-0.155227669443958,
-0.736835050782132));
#36377=CARTESIAN_POINT('Ctrl Pts',(0.168541111895386,-0.0995021226113438,
-0.733128502201599));
#36378=CARTESIAN_POINT('Ctrl Pts',(0.201439970374078,-0.0437765757787303,
-0.729421953621065));
#36379=CARTESIAN_POINT('Ctrl Pts',(0.203964633096664,0.0298810762957444,
-0.725715405040532));
#36380=CARTESIAN_POINT('Ctrl Pts',(0.174958558506099,0.0877284539034402,
-0.722008856459998));
#36381=CARTESIAN_POINT('Ctrl Pts',(0.145952483915533,0.145575831511137,
-0.718302307879465));
#36382=CARTESIAN_POINT('Ctrl Pts',(0.0854156720118136,0.187612934652054,
-0.714595759298931));
#36383=CARTESIAN_POINT('Ctrl Pts',(0.0210798796572213,0.194582675199021,
-0.710889210718398));
#36384=CARTESIAN_POINT('Ctrl Pts',(-0.0432559126973706,0.201552415745988,
-0.707182662137865));
#36385=CARTESIAN_POINT('Ctrl Pts',(-0.111390685502836,0.173454793699006,
-0.703476113557332));
#36386=CARTESIAN_POINT('Ctrl Pts',(-0.152112075758141,0.123161256980201,
-0.699769564976798));
#36387=CARTESIAN_POINT('Ctrl Pts',(-0.179880392163595,0.0888655997837939,
-0.69724203305534));
#36388=CARTESIAN_POINT('Ctrl Pts',(-0.194901457733376,0.0442488196347122,
-0.694714501133882));
#36389=CARTESIAN_POINT('Ctrl Pts',(-0.195242183955992,-0.000159443835737465,
-0.692186969212424));
#36390=CARTESIAN_POINT('Origin',(0.,0.,-0.56));
#36391=CARTESIAN_POINT('',(-0.195707701541145,-4.64929517365598E-5,-0.612013030787577));
#36392=CARTESIAN_POINT('',(-0.195716357106892,-2.76508156398553E-5,-0.622186969212424));
#36393=CARTESIAN_POINT('',(-0.1954,-2.39295984553393E-17,-0.56));
#36394=CARTESIAN_POINT('Ctrl Pts',(-0.195707701541145,-4.64929517365598E-5,
-0.612013030787577));
#36395=CARTESIAN_POINT('Ctrl Pts',(-0.195508230414245,0.0621601619704314,
-0.615575407701586));
#36396=CARTESIAN_POINT('Ctrl Pts',(-0.163290136797982,0.124544569513887,
-0.619137784615595));
#36397=CARTESIAN_POINT('Ctrl Pts',(-0.112366285628439,0.160251677767253,
-0.622700161529604));
#36398=CARTESIAN_POINT('Ctrl Pts',(-0.0593815137123928,0.197403875472946,
-0.626406710110138));
#36399=CARTESIAN_POINT('Ctrl Pts',(0.0138537212886752,0.205675785227547,
-0.630113258690671));
#36400=CARTESIAN_POINT('Ctrl Pts',(0.0737905478189984,0.181278066587556,
-0.633819807271204));
#36401=CARTESIAN_POINT('Ctrl Pts',(0.133727374349322,0.156880347947566,
-0.637526355851737));
#36402=CARTESIAN_POINT('Ctrl Pts',(0.180365792408901,0.0998130009129835,
-0.641232904432271));
#36403=CARTESIAN_POINT('Ctrl Pts',(0.192340863426324,0.0362184294191327,
-0.644939453012805));
#36404=CARTESIAN_POINT('Ctrl Pts',(0.204315934443746,-0.0273761420747171,
-0.648646001593338));
#36405=CARTESIAN_POINT('Ctrl Pts',(0.181627658419013,-0.097497938027835,
-0.652352550173871));
#36406=CARTESIAN_POINT('Ctrl Pts',(0.134669475861856,-0.142024345251873,
-0.656059098754404));
#36407=CARTESIAN_POINT('Ctrl Pts',(0.0877112933047003,-0.186550752475911,
-0.659765647334937));
#36408=CARTESIAN_POINT('Ctrl Pts',(0.0164832042151199,-0.20548177097087,
-0.663472195915471));
#36409=CARTESIAN_POINT('Ctrl Pts',(-0.0463853881973819,-0.190145150174586,
-0.667178744496004));
#36410=CARTESIAN_POINT('Ctrl Pts',(-0.109253980609885,-0.174808529378301,
-0.670885293076538));
#36411=CARTESIAN_POINT('Ctrl Pts',(-0.163763076345309,-0.125204269290772,
-0.674591841657071));
#36412=CARTESIAN_POINT('Ctrl Pts',(-0.18494219976433,-0.0640559530379924,
-0.678298390237604));
#36413=CARTESIAN_POINT('Ctrl Pts',(-0.192017320005872,-0.0436286822063926,
-0.679536603754262));
#36414=CARTESIAN_POINT('Ctrl Pts',(-0.195372922452669,-0.0219131318070045,
-0.680774817270919));
#36415=CARTESIAN_POINT('Ctrl Pts',(-0.195216518518634,-0.000150737487880678,
-0.682013030787577));
#36416=CARTESIAN_POINT('Ctrl Pts',(-0.195242183955992,-0.000159443835737465,
-0.692186969212424));
#36417=CARTESIAN_POINT('Ctrl Pts',(-0.195401122361176,-0.0208745461803437,
-0.691007952553348));
#36418=CARTESIAN_POINT('Ctrl Pts',(-0.192365709442112,-0.0415442765813754,
-0.689828935894273));
#36419=CARTESIAN_POINT('Ctrl Pts',(-0.185939734982374,-0.0610998671791814,
-0.688649919235198));
#36420=CARTESIAN_POINT('Ctrl Pts',(-0.165737996246156,-0.122578003229134,
-0.684943370654664));
#36421=CARTESIAN_POINT('Ctrl Pts',(-0.112026511068576,-0.173044823938413,
-0.681236822074131));
#36422=CARTESIAN_POINT('Ctrl Pts',(-0.0494103717638331,-0.189381609392125,
-0.677530273493598));
#36423=CARTESIAN_POINT('Ctrl Pts',(0.01320576754091,-0.205718394845837,
-0.673823724913065));
#36424=CARTESIAN_POINT('Ctrl Pts',(0.0847265609728156,-0.187925145043982,
-0.670117176332531));
#36425=CARTESIAN_POINT('Ctrl Pts',(0.132388518224354,-0.144152901656579,
-0.666410627751998));
#36426=CARTESIAN_POINT('Ctrl Pts',(0.180050475475893,-0.100380658269176,
-0.662704079171464));
#36427=CARTESIAN_POINT('Ctrl Pts',(0.203853596547065,-0.0306294212962258,
-0.658997530590931));
#36428=CARTESIAN_POINT('Ctrl Pts',(0.192893733296786,0.0331479481837195,
-0.655290982010398));
#36429=CARTESIAN_POINT('Ctrl Pts',(0.181933870046508,0.0969253176636644,
-0.651584433429865));
#36430=CARTESIAN_POINT('Ctrl Pts',(0.136211022474779,0.154728819650604,
-0.647877884849331));
#36431=CARTESIAN_POINT('Ctrl Pts',(0.0766707086837813,0.180078819531201,
-0.644171336268798));
#36432=CARTESIAN_POINT('Ctrl Pts',(0.017130394892783,0.205428819411797,
-0.640464787688264));
#36433=CARTESIAN_POINT('Ctrl Pts',(-0.0562273851174842,0.198325317186049,
-0.636758239107731));
#36434=CARTESIAN_POINT('Ctrl Pts',(-0.10979762224029,0.162022408833456,
-0.633051690527198));
#36435=CARTESIAN_POINT('Ctrl Pts',(-0.16213973013031,0.126551766033109,
-0.629430116755607));
#36436=CARTESIAN_POINT('Ctrl Pts',(-0.195591177290711,0.0632051975665141,
-0.625808542984015));
#36437=CARTESIAN_POINT('Ctrl Pts',(-0.195716357106892,-2.76508156398553E-5,
-0.622186969212424));
#36438=CARTESIAN_POINT('Origin',(0.,0.,-0.56));
#36439=CARTESIAN_POINT('',(-0.195354221420379,0.000178407506690854,-0.542013030787577));
#36440=CARTESIAN_POINT('',(-0.195323759319157,0.000175885597776871,-0.552186969212423));
#36441=CARTESIAN_POINT('',(-0.1954,-2.39295984553393E-17,-0.56));
#36442=CARTESIAN_POINT('Ctrl Pts',(-0.195354221420379,0.000178407506690854,
-0.542013030787577));
#36443=CARTESIAN_POINT('Ctrl Pts',(-0.195503876356803,0.0168432028806296,
-0.542962900971186));
#36444=CARTESIAN_POINT('Ctrl Pts',(-0.193549298846388,0.033473417735259,
-0.543912771154795));
#36445=CARTESIAN_POINT('Ctrl Pts',(-0.189353619137088,0.0495175654979228,
-0.544862641338404));
#36446=CARTESIAN_POINT('Ctrl Pts',(-0.172981391711447,0.112124450250982,
-0.548569189918937));
#36447=CARTESIAN_POINT('Ctrl Pts',(-0.122484173387406,0.165807362599245,
-0.55227573849947));
#36448=CARTESIAN_POINT('Ctrl Pts',(-0.0609946091473485,0.185974299375253,
-0.555982287080004));
#36449=CARTESIAN_POINT('Ctrl Pts',(0.00049495509270836,0.206141236151261,
-0.559688835660537));
#36450=CARTESIAN_POINT('Ctrl Pts',(0.0729768652487818,0.192792197355014,
-0.56339538424107));
#36451=CARTESIAN_POINT('Ctrl Pts',(0.123247345926238,0.15204234309985,-0.567101932821604));
#36452=CARTESIAN_POINT('Ctrl Pts',(0.173517826603694,0.111292488844685,
-0.570808481402137));
#36453=CARTESIAN_POINT('Ctrl Pts',(0.201576877802532,0.043141819130602,
-0.57451502998267));
#36454=CARTESIAN_POINT('Ctrl Pts',(0.194570720810425,-0.0211900206811239,
-0.578221578563204));
#36455=CARTESIAN_POINT('Ctrl Pts',(0.187564563818317,-0.0855218604928506,
-0.581928127143737));
#36456=CARTESIAN_POINT('Ctrl Pts',(0.145493198635262,-0.14603487040222,
-0.58563467572427));
#36457=CARTESIAN_POINT('Ctrl Pts',(0.0876294087333888,-0.175008197231417,
-0.589341224304804));
#36458=CARTESIAN_POINT('Ctrl Pts',(0.0297656188315169,-0.203981524060614,
-0.593047772885337));
#36459=CARTESIAN_POINT('Ctrl Pts',(-0.043890595789172,-0.201415167809638,
-0.596754321465871));
#36460=CARTESIAN_POINT('Ctrl Pts',(-0.099597513898962,-0.168484769633043,
-0.600460870046404));
#36461=CARTESIAN_POINT('Ctrl Pts',(-0.155304432008752,-0.135554371456448,
-0.604167418626937));
#36462=CARTESIAN_POINT('Ctrl Pts',(-0.193062053607643,-0.0722599313542328,
-0.607873967207471));
#36463=CARTESIAN_POINT('Ctrl Pts',(-0.195573709991577,-0.00759646847473161,
-0.611580515788004));
#36464=CARTESIAN_POINT('Ctrl Pts',(-0.195671404566122,-0.00508128784131614,
-0.611724687454528));
#36465=CARTESIAN_POINT('Ctrl Pts',(-0.195715774264914,-0.00256403596459507,
-0.611868859121052));
#36466=CARTESIAN_POINT('Ctrl Pts',(-0.195707701541145,-4.64929517365598E-5,
-0.612013030787577));
#36467=CARTESIAN_POINT('Ctrl Pts',(-0.195716357106892,-2.76508156398553E-5,
-0.622186969212424));
#36468=CARTESIAN_POINT('Ctrl Pts',(-0.195719294263949,-0.00151131497631132,
-0.622101994403482));
#36469=CARTESIAN_POINT('Ctrl Pts',(-0.195703884111172,-0.00299491652998268,
-0.62201701959454));
#36470=CARTESIAN_POINT('Ctrl Pts',(-0.195669940176563,-0.00447809392031211,
-0.621932044785597));
#36471=CARTESIAN_POINT('Ctrl Pts',(-0.194189326754688,-0.0691733738420494,
-0.618225496205064));
#36472=CARTESIAN_POINT('Ctrl Pts',(-0.157445405675594,-0.133061619206086,
-0.614518947624531));
#36473=CARTESIAN_POINT('Ctrl Pts',(-0.102270472059719,-0.166875790210921,
-0.610812399043998));
#36474=CARTESIAN_POINT('Ctrl Pts',(-0.0470955384438438,-0.200689961215756,
-0.607105850463464));
#36475=CARTESIAN_POINT('Ctrl Pts',(0.0265104077088127,-0.20443005786139,
-0.603399301882931));
#36476=CARTESIAN_POINT('Ctrl Pts',(0.084828673023672,-0.176382751557177,
-0.599692753302397));
#36477=CARTESIAN_POINT('Ctrl Pts',(0.143146938338532,-0.148335445252965,
-0.595986204721864));
#36478=CARTESIAN_POINT('Ctrl Pts',(0.186177522815594,-0.0885007359989063,
-0.592279656141331));
#36479=CARTESIAN_POINT('Ctrl Pts',(0.194208227107422,-0.0242887491986593,
-0.588573107560798));
#36480=CARTESIAN_POINT('Ctrl Pts',(0.202238931399251,0.0399232376015871,
-0.584866558980264));
#36481=CARTESIAN_POINT('Ctrl Pts',(0.175269755505846,0.108512501948022,
-0.58116001039973));
#36482=CARTESIAN_POINT('Ctrl Pts',(0.125655209083708,0.15005847941376,-0.577453461819197));
#36483=CARTESIAN_POINT('Ctrl Pts',(0.0760406626615685,0.191604456879499,
-0.573746913238664));
#36484=CARTESIAN_POINT('Ctrl Pts',(0.00378074571069509,0.20610714746454,
-0.570040364658131));
#36485=CARTESIAN_POINT('Ctrl Pts',(-0.0580224608868743,0.186922906157784,
-0.566333816077598));
#36486=CARTESIAN_POINT('Ctrl Pts',(-0.119825667484444,0.167738664851027,
-0.562627267497064));
#36487=CARTESIAN_POINT('Ctrl Pts',(-0.171172163728709,0.114867491652473,
-0.55892071891653));
#36488=CARTESIAN_POINT('Ctrl Pts',(-0.188540252620716,0.0525295341266019,
-0.555214170335997));
#36489=CARTESIAN_POINT('Ctrl Pts',(-0.193268523595349,0.0355587115438646,
-0.554205103294806));
#36490=CARTESIAN_POINT('Ctrl Pts',(-0.195478516591736,0.0178862670678721,
-0.553196036253614));
#36491=CARTESIAN_POINT('Ctrl Pts',(-0.195323759319157,0.000175885597776871,
-0.552186969212423));
#36492=CARTESIAN_POINT('Origin',(0.,0.,-0.56));
#36493=CARTESIAN_POINT('',(-0.195092696479446,-5.43760739497856E-5,-0.472013030787576));
#36494=CARTESIAN_POINT('',(-0.195102639049386,-7.04728118876389E-5,-0.482186969212424));
#36495=CARTESIAN_POINT('',(-0.1954,-2.39295984553393E-17,-0.56));
#36496=CARTESIAN_POINT('Ctrl Pts',(-0.195092696479446,-5.43760739497856E-5,
-0.472013030787576));
#36497=CARTESIAN_POINT('Ctrl Pts',(-0.195003108324315,0.0359258718284784,
-0.474056942821319));
#36498=CARTESIAN_POINT('Ctrl Pts',(-0.185481340256412,0.0719502167704471,
-0.476100854855061));
#36499=CARTESIAN_POINT('Ctrl Pts',(-0.166817881086069,0.102364920373673,
-0.478144766888803));
#36500=CARTESIAN_POINT('Ctrl Pts',(-0.132972482187457,0.157520707221052,
-0.481851315469337));
#36501=CARTESIAN_POINT('Ctrl Pts',(-0.0690634452147766,0.194228460215231,
-0.48555786404987));
#36502=CARTESIAN_POINT('Ctrl Pts',(-0.00436733455159703,0.195672452741996,
-0.489264412630403));
#36503=CARTESIAN_POINT('Ctrl Pts',(0.0603287761115817,0.197116445268761,
-0.492970961210936));
#36504=CARTESIAN_POINT('Ctrl Pts',(0.125811960465259,0.163296677328114,
-0.49667750979147));
#36505=CARTESIAN_POINT('Ctrl Pts',(0.162084541285929,0.109705897057926,
-0.500384058372003));
#36506=CARTESIAN_POINT('Ctrl Pts',(0.198357122106599,0.0561151167877383,
-0.504090606952537));
#36507=CARTESIAN_POINT('Ctrl Pts',(0.205419099394263,-0.0172466758119902,
-0.50779715553307));
#36508=CARTESIAN_POINT('Ctrl Pts',(0.180035399636139,-0.0767726334771048,
-0.511503704113603));
#36509=CARTESIAN_POINT('Ctrl Pts',(0.154651699878015,-0.136298591142221,
-0.515210252694137));
#36510=CARTESIAN_POINT('Ctrl Pts',(0.0968223230741041,-0.181988713872723,
-0.51891680127467));
#36511=CARTESIAN_POINT('Ctrl Pts',(0.0330387570242473,-0.192912474732577,
-0.522623349855203));
#36512=CARTESIAN_POINT('Ctrl Pts',(-0.0307448090256087,-0.20383623559243,
-0.526329898435737));
#36513=CARTESIAN_POINT('Ctrl Pts',(-0.100482564321409,-0.179993634581636,
-0.53003644701627));
#36514=CARTESIAN_POINT('Ctrl Pts',(-0.144227823705689,-0.132306905497313,
-0.533742995596803));
#36515=CARTESIAN_POINT('Ctrl Pts',(-0.176762568331955,-0.0968407641449097,
-0.536499673993728));
#36516=CARTESIAN_POINT('Ctrl Pts',(-0.194919898354602,-0.0481855502101019,
-0.539256352390652));
#36517=CARTESIAN_POINT('Ctrl Pts',(-0.195354221420379,0.000178407506690854,
-0.542013030787577));
#36518=CARTESIAN_POINT('Ctrl Pts',(-0.195323759319157,0.000175885597776871,
-0.552186969212423));
#36519=CARTESIAN_POINT('Ctrl Pts',(-0.194910055502839,-0.0471682700629787,
-0.549489487673081));
#36520=CARTESIAN_POINT('Ctrl Pts',(-0.177597305086522,-0.0947835321655527,
-0.546792006133739));
#36521=CARTESIAN_POINT('Ctrl Pts',(-0.146318441124281,-0.129991125084758,
-0.544094524594397));
#36522=CARTESIAN_POINT('Ctrl Pts',(-0.10333885919609,-0.17836908491706,
-0.540387976013864));
#36523=CARTESIAN_POINT('Ctrl Pts',(-0.0339900137999589,-0.203320262728478,
-0.53668142743333));
#36524=CARTESIAN_POINT('Ctrl Pts',(0.0299595685248398,-0.193414588559514,
-0.532974878852797));
#36525=CARTESIAN_POINT('Ctrl Pts',(0.0939091508496379,-0.183508914390551,
-0.529268330272263));
#36526=CARTESIAN_POINT('Ctrl Pts',(0.152459470103104,-0.138746388241206,
-0.52556178169173));
#36527=CARTESIAN_POINT('Ctrl Pts',(0.178788776615697,-0.0796326074551339,
-0.521855233111197));
#36528=CARTESIAN_POINT('Ctrl Pts',(0.205118083128289,-0.0205188266690613,
-0.518148684530664));
#36529=CARTESIAN_POINT('Ctrl Pts',(0.199226376900009,0.0529462087537386,
-0.51444213595013));
#36530=CARTESIAN_POINT('Ctrl Pts',(0.163812633301037,0.107108356279148,
-0.510735587369597));
#36531=CARTESIAN_POINT('Ctrl Pts',(0.128398889702065,0.161270503804557,
-0.507029038789064));
#36532=CARTESIAN_POINT('Ctrl Pts',(0.0634631087324024,0.196129763432576,
-0.50332249020853));
#36533=CARTESIAN_POINT('Ctrl Pts',(-0.00124779645749392,0.195717198574478,
-0.499615941627997));
#36534=CARTESIAN_POINT('Ctrl Pts',(-0.0659587016473898,0.19530463371638,
-0.495909393047463));
#36535=CARTESIAN_POINT('Ctrl Pts',(-0.13044473105752,0.159620244372166,
-0.49220284446693));
#36536=CARTESIAN_POINT('Ctrl Pts',(-0.16516500156249,0.105010956917379,
-0.488496295886397));
#36537=CARTESIAN_POINT('Ctrl Pts',(-0.184865406945462,0.0740254523436011,
-0.486393186995072));
#36538=CARTESIAN_POINT('Ctrl Pts',(-0.194982821215997,0.0369471372026458,
-0.484290078103748));
#36539=CARTESIAN_POINT('Ctrl Pts',(-0.195102639049386,-7.04728118876389E-5,
-0.482186969212424));
#36540=CARTESIAN_POINT('Origin',(0.,0.,-0.56));
#36541=CARTESIAN_POINT('',(-0.195553853432401,-0.000152262014626814,-0.402013030787576));
#36542=CARTESIAN_POINT('',(-0.195582229504364,-0.000141746448570984,-0.412186969212424));
#36543=CARTESIAN_POINT('',(-0.1954,-2.39295984553393E-17,-0.56));
#36544=CARTESIAN_POINT('Ctrl Pts',(-0.195553853432401,-0.000152262014626814,
-0.402013030787576));
#36545=CARTESIAN_POINT('Ctrl Pts',(-0.195082861820371,0.054756524969974,
-0.405150984671452));
#36546=CARTESIAN_POINT('Ctrl Pts',(-0.170885527056883,0.110028797080402,
-0.408288938555327));
#36547=CARTESIAN_POINT('Ctrl Pts',(-0.129908286827409,0.146392005883943,
-0.411426892439203));
#36548=CARTESIAN_POINT('Ctrl Pts',(-0.0815060039298814,0.189344198606403,
-0.415133441019736));
#36549=CARTESIAN_POINT('Ctrl Pts',(-0.00969186798292979,0.2059138701436,
-0.418839989600269));
#36550=CARTESIAN_POINT('Ctrl Pts',(0.0526362512551988,0.188510496861456,
-0.422546538180803));
#36551=CARTESIAN_POINT('Ctrl Pts',(0.114964370493328,0.171107123579313,
-0.426253086761336));
#36552=CARTESIAN_POINT('Ctrl Pts',(0.167806473022633,0.119730705477828,
-0.42995963534187));
#36553=CARTESIAN_POINT('Ctrl Pts',(0.18695572847696,0.0579166466812693,
-0.433666183922403));
#36554=CARTESIAN_POINT('Ctrl Pts',(0.206104983931288,-0.00389741211528853,
-0.437372732502936));
#36555=CARTESIAN_POINT('Ctrl Pts',(0.191561392310639,-0.0761491116069204,
-0.441079281083469));
#36556=CARTESIAN_POINT('Ctrl Pts',(0.149987335284637,-0.125740135308376,
-0.444785829664003));
#36557=CARTESIAN_POINT('Ctrl Pts',(0.108413278258634,-0.175331159009831,
-0.448492378244536));
#36558=CARTESIAN_POINT('Ctrl Pts',(0.0398087558272775,-0.20226150692111,
-0.45219892682507));
#36559=CARTESIAN_POINT('Ctrl Pts',(-0.0243986778933489,-0.194194456383829,
-0.455905475405603));
#36560=CARTESIAN_POINT('Ctrl Pts',(-0.0886061116139757,-0.186127405846548,
-0.459612023986136));
#36561=CARTESIAN_POINT('Ctrl Pts',(-0.148416456623872,-0.143062956860706,
-0.46331857256667));
#36562=CARTESIAN_POINT('Ctrl Pts',(-0.176430748716548,-0.084728822017495,
-0.467025121147203));
#36563=CARTESIAN_POINT('Ctrl Pts',(-0.18899704451809,-0.0585620357449116,
-0.468687757693994));
#36564=CARTESIAN_POINT('Ctrl Pts',(-0.195165572678823,-0.0293227957209801,
-0.470350394240785));
#36565=CARTESIAN_POINT('Ctrl Pts',(-0.195092696479446,-5.43760739497856E-5,
-0.472013030787576));
#36566=CARTESIAN_POINT('Ctrl Pts',(-0.195102639049386,-7.04728118876389E-5,
-0.482186969212424));
#36567=CARTESIAN_POINT('Ctrl Pts',(-0.195193989844546,-0.0282932174076707,
-0.480583529523215));
#36568=CARTESIAN_POINT('Ctrl Pts',(-0.189473986501732,-0.0564806756233877,
-0.478980089834006));
#36569=CARTESIAN_POINT('Ctrl Pts',(-0.177758887424744,-0.0819057797433008,
-0.477376650144797));
#36570=CARTESIAN_POINT('Ctrl Pts',(-0.150677991182218,-0.140679043383832,
-0.473670101564263));
#36571=CARTESIAN_POINT('Ctrl Pts',(-0.091561687097356,-0.184691385099535,
-0.46996355298373));
#36572=CARTESIAN_POINT('Ctrl Pts',(-0.0274910010256872,-0.193780865093658,
-0.466257004403196));
#36573=CARTESIAN_POINT('Ctrl Pts',(0.0365796850459811,-0.202870345087781,
-0.462550455822663));
#36574=CARTESIAN_POINT('Ctrl Pts',(0.105604753104456,-0.177036963360327,
-0.45884390724213));
#36575=CARTESIAN_POINT('Ctrl Pts',(0.14796399817062,-0.128114925200796,
-0.455137358661597));
#36576=CARTESIAN_POINT('Ctrl Pts',(0.190323243236784,-0.0791928870412662,
-0.451430810081063));
#36577=CARTESIAN_POINT('Ctrl Pts',(0.206016665310636,-0.00718219244966056,
-0.44772426150053));
#36578=CARTESIAN_POINT('Ctrl Pts',(0.187855148368726,0.0549292458095403,
-0.444017712919996));
#36579=CARTESIAN_POINT('Ctrl Pts',(0.169693631426815,0.117040684068742,
-0.440311164339463));
#36580=CARTESIAN_POINT('Ctrl Pts',(0.117677175469141,0.169252865995539,
-0.43660461575893));
#36581=CARTESIAN_POINT('Ctrl Pts',(0.0556343843049091,0.187647526220983,
-0.432898067178396));
#36582=CARTESIAN_POINT('Ctrl Pts',(-0.00640840685932162,0.206042186446427,
-0.429191518597863));
#36583=CARTESIAN_POINT('Ctrl Pts',(-0.0784775332301094,0.19061932497052,
-0.42548497001733));
#36584=CARTESIAN_POINT('Ctrl Pts',(-0.127558314596203,0.148444114707243,
-0.421778421436796));
#36585=CARTESIAN_POINT('Ctrl Pts',(-0.169893833240166,0.112065121734498,
-0.418581270695339));
#36586=CARTESIAN_POINT('Ctrl Pts',(-0.195125475882863,0.0557817443309313,
-0.415384119953881));
#36587=CARTESIAN_POINT('Ctrl Pts',(-0.195582229504364,-0.000141746448570984,
-0.412186969212424));
#36588=CARTESIAN_POINT('Origin',(0.,0.,-0.56));
#36589=CARTESIAN_POINT('',(-0.195574688910705,0.000144757554679794,-0.332013030787576));
#36590=CARTESIAN_POINT('',(-0.195545913560384,0.000154829267465116,-0.342186969212424));
#36591=CARTESIAN_POINT('',(-0.1954,-2.39295984553393E-17,-0.56));
#36592=CARTESIAN_POINT('Ctrl Pts',(-0.195574688910705,0.000144757554679794,
-0.332013030787576));
#36593=CARTESIAN_POINT('Ctrl Pts',(-0.195650878894854,0.00933662874909953,
-0.332538477941052));
#36594=CARTESIAN_POINT('Ctrl Pts',(-0.195058964365449,0.0185186393964773,
-0.333063925094527));
#36595=CARTESIAN_POINT('Ctrl Pts',(-0.19376528178542,0.0276006874476484,
-0.333589372248002));
#36596=CARTESIAN_POINT('Ctrl Pts',(-0.184639535649099,0.0916662211359821,
-0.337295920828535));
#36597=CARTESIAN_POINT('Ctrl Pts',(-0.140593736189925,0.150757605336143,
-0.341002469409069));
#36598=CARTESIAN_POINT('Ctrl Pts',(-0.0818051501088732,0.177805229925724,
-0.344709017989602));
#36599=CARTESIAN_POINT('Ctrl Pts',(-0.0230165640278225,0.204852854515306,
-0.348415566570136));
#36600=CARTESIAN_POINT('Ctrl Pts',(0.0505148086751044,0.199856719494309,
-0.352122115150669));
#36601=CARTESIAN_POINT('Ctrl Pts',(0.105104436528749,0.165105541382207,
-0.355828663731202));
#36602=CARTESIAN_POINT('Ctrl Pts',(0.159694064382394,0.130354363270105,
-0.359535212311736));
#36603=CARTESIAN_POINT('Ctrl Pts',(0.195341947386756,0.0658481420668959,
-0.363241760892269));
#36604=CARTESIAN_POINT('Ctrl Pts',(0.195717882626462,0.00113701070568482,
-0.366948309472803));
#36605=CARTESIAN_POINT('Ctrl Pts',(0.196093817866168,-0.063574120655523,
-0.370654858053336));
#36606=CARTESIAN_POINT('Ctrl Pts',(0.161197805341222,-0.128490162174734,
-0.374361406633869));
#36607=CARTESIAN_POINT('Ctrl Pts',(0.107015618047075,-0.163873243292415,
-0.378067955214402));
#36608=CARTESIAN_POINT('Ctrl Pts',(0.0528334307529256,-0.199256324410097,
-0.381774503794935));
#36609=CARTESIAN_POINT('Ctrl Pts',(-0.0206349313104262,-0.205106445126249,
-0.385481052375469));
#36610=CARTESIAN_POINT('Ctrl Pts',(-0.0797338016833294,-0.178743680286252,
-0.389187600956003));
#36611=CARTESIAN_POINT('Ctrl Pts',(-0.138832672056233,-0.152380915446255,
-0.392894149536536));
#36612=CARTESIAN_POINT('Ctrl Pts',(-0.183562050738688,-0.093805265050108,
-0.396600698117069));
#36613=CARTESIAN_POINT('Ctrl Pts',(-0.193431525155864,-0.0298500828981727,
-0.400307246697602));
#36614=CARTESIAN_POINT('Ctrl Pts',(-0.194945529543094,-0.0200391829179675,
-0.40087584139426));
#36615=CARTESIAN_POINT('Ctrl Pts',(-0.195639196730193,-0.0101016896463702,
-0.401444436090918));
#36616=CARTESIAN_POINT('Ctrl Pts',(-0.195553853432401,-0.000152262014626814,
-0.402013030787576));
#36617=CARTESIAN_POINT('Ctrl Pts',(-0.195582229504364,-0.000141746448570984,
-0.412186969212424));
#36618=CARTESIAN_POINT('Ctrl Pts',(-0.195655003460488,-0.00905196296956772,
-0.411677571373348));
#36619=CARTESIAN_POINT('Ctrl Pts',(-0.195098851215254,-0.0179530435413701,
-0.411168173534272));
#36620=CARTESIAN_POINT('Ctrl Pts',(-0.193882746133758,-0.0267630260896144,
-0.410658775695196));
#36621=CARTESIAN_POINT('Ctrl Pts',(-0.185033959943818,-0.0908673975725523,
-0.406952227114663));
#36622=CARTESIAN_POINT('Ctrl Pts',(-0.141243951202538,-0.150148581487782,
-0.403245678534129));
#36623=CARTESIAN_POINT('Ctrl Pts',(-0.0825728095466741,-0.177450020956349,
-0.399539129953596));
#36624=CARTESIAN_POINT('Ctrl Pts',(-0.0239016678908108,-0.204751460424916,
-0.395832581373063));
#36625=CARTESIAN_POINT('Ctrl Pts',(0.0496506066796362,-0.200073155446821,
-0.392126032792529));
#36626=CARTESIAN_POINT('Ctrl Pts',(0.104389907602852,-0.165558225420882,
-0.388419484211996));
#36627=CARTESIAN_POINT('Ctrl Pts',(0.159129208526068,-0.131043295394943,
-0.384712935631463));
#36628=CARTESIAN_POINT('Ctrl Pts',(0.195055535802052,-0.0666917403211604,
-0.381006387050929));
#36629=CARTESIAN_POINT('Ctrl Pts',(0.195711131915094,-0.00198284097962335,
-0.377299838470396));
#36630=CARTESIAN_POINT('Ctrl Pts',(0.196366728028137,0.0627260583619147,
-0.373593289889863));
#36631=CARTESIAN_POINT('Ctrl Pts',(0.161751592978236,0.127792301971207,
-0.36988674130933));
#36632=CARTESIAN_POINT('Ctrl Pts',(0.107722830516848,0.163409212100406,
-0.366180192728796));
#36633=CARTESIAN_POINT('Ctrl Pts',(0.0536940680554607,0.199026122229604,
-0.362473644148263));
#36634=CARTESIAN_POINT('Ctrl Pts',(-0.0197483218174141,0.20519369887871,
-0.358767095567729));
#36635=CARTESIAN_POINT('Ctrl Pts',(-0.0789605704353628,0.179086591151826,
-0.355060546987196));
#36636=CARTESIAN_POINT('Ctrl Pts',(-0.138172819053312,0.152979483424941,
-0.351353998406662));
#36637=CARTESIAN_POINT('Ctrl Pts',(-0.183154926416334,0.0945976913220663,
-0.347647449826129));
#36638=CARTESIAN_POINT('Ctrl Pts',(-0.193300705595433,0.0306857626616098,
-0.343940901245596));
#36639=CARTESIAN_POINT('Ctrl Pts',(-0.1949010270011,0.0206047599404502,
-0.343356257234539));
#36640=CARTESIAN_POINT('Ctrl Pts',(-0.19563463405017,0.0103861695630058,
-0.342771613223481));
#36641=CARTESIAN_POINT('Ctrl Pts',(-0.195545913560384,0.000154829267465116,
-0.342186969212424));
#36642=CARTESIAN_POINT('Origin',(0.,0.,-0.56));
#36643=CARTESIAN_POINT('',(-0.195099694633333,6.61648413741723E-5,-0.262013030787576));
#36644=CARTESIAN_POINT('',(-0.195090438596196,4.99224700532782E-5,-0.272186969212423));
#36645=CARTESIAN_POINT('',(-0.1954,-2.39295984553393E-17,-0.56));
#36646=CARTESIAN_POINT('Ctrl Pts',(-0.195099694633333,6.61648413741722E-5,
-0.262013030787576));
#36647=CARTESIAN_POINT('Ctrl Pts',(-0.195186244887412,0.0285724785253478,
-0.263632519791185));
#36648=CARTESIAN_POINT('Ctrl Pts',(-0.189346489992417,0.057045028877643,
-0.265252008794793));
#36649=CARTESIAN_POINT('Ctrl Pts',(-0.17740326045936,0.0826732456169493,
-0.266871497798402));
#36650=CARTESIAN_POINT('Ctrl Pts',(-0.150068613311955,0.141328926615721,
-0.270578046378935));
#36651=CARTESIAN_POINT('Ctrl Pts',(-0.0907626488691269,0.185085374337137,
-0.274284594959468));
#36652=CARTESIAN_POINT('Ctrl Pts',(-0.0266532758367687,0.19389787328715,
-0.277991143540002));
#36653=CARTESIAN_POINT('Ctrl Pts',(0.0374560971955886,0.202710372237162,
-0.281697692120535));
#36654=CARTESIAN_POINT('Ctrl Pts',(0.106368878817475,0.176578922415771,
-0.285404240701069));
#36655=CARTESIAN_POINT('Ctrl Pts',(0.148516302139648,0.127474273373296,
-0.289110789281602));
#36656=CARTESIAN_POINT('Ctrl Pts',(0.190663725461821,0.0783696243308199,
-0.292817337862135));
#36657=CARTESIAN_POINT('Ctrl Pts',(0.20604579048428,0.00629177606725653,
-0.296523886442669));
#36658=CARTESIAN_POINT('Ctrl Pts',(0.187616013061667,-0.0557405957499364,
-0.300230435023202));
#36659=CARTESIAN_POINT('Ctrl Pts',(0.169186235639053,-0.11777296756713,
-0.303936983603735));
#36660=CARTESIAN_POINT('Ctrl Pts',(0.116944615771367,-0.169759862937953,
-0.307643532184269));
#36661=CARTESIAN_POINT('Ctrl Pts',(0.0548229042621313,-0.187886219670852,
-0.311350080764802));
#36662=CARTESIAN_POINT('Ctrl Pts',(-0.00729880724710397,-0.20601257640375,
-0.315056629345336));
#36663=CARTESIAN_POINT('Ctrl Pts',(-0.0793006103978895,-0.190278394498723,
-0.318763177925869));
#36664=CARTESIAN_POINT('Ctrl Pts',(-0.128198665566548,-0.147891461957956,
-0.322469726506402));
#36665=CARTESIAN_POINT('Ctrl Pts',(-0.170164842374355,-0.111513379042165,
-0.32565082793346));
#36666=CARTESIAN_POINT('Ctrl Pts',(-0.195113428314472,-0.0555036066633279,
-0.328831929360518));
#36667=CARTESIAN_POINT('Ctrl Pts',(-0.195574688910705,0.000144757554679794,
-0.332013030787576));
#36668=CARTESIAN_POINT('Ctrl Pts',(-0.195545913560384,0.000154829267465116,
-0.342186969212424));
#36669=CARTESIAN_POINT('Ctrl Pts',(-0.195072160477773,-0.0544788750319072,
-0.339065064642948));
#36670=CARTESIAN_POINT('Ctrl Pts',(-0.171150663017774,-0.109476128897877,
-0.335943160073472));
#36671=CARTESIAN_POINT('Ctrl Pts',(-0.13053973515857,-0.14582920269464,
-0.332821255503996));
#36672=CARTESIAN_POINT('Ctrl Pts',(-0.0823235345474341,-0.188990174172393,
-0.329114706923462));
#36673=CARTESIAN_POINT('Ctrl Pts',(-0.0105816823299884,-0.205870051909861,
-0.325408158342929));
#36674=CARTESIAN_POINT('Ctrl Pts',(0.0518210647242702,-0.188736207614769,
-0.321701609762396));
#36675=CARTESIAN_POINT('Ctrl Pts',(0.11422381177853,-0.171602363319677,
-0.317995061181862));
#36676=CARTESIAN_POINT('Ctrl Pts',(0.167287453669601,-0.120454796992023,
-0.314288512601329));
#36677=CARTESIAN_POINT('Ctrl Pts',(0.186703673424414,-0.0587240763527305,
-0.310581964020795));
#36678=CARTESIAN_POINT('Ctrl Pts',(0.206119893179227,0.00300664428656105,
-0.306875415440262));
#36679=CARTESIAN_POINT('Ctrl Pts',(0.191888690797781,0.0753205192374923,
-0.303168866859729));
#36680=CARTESIAN_POINT('Ctrl Pts',(0.150529343245733,0.125090749601239,
-0.299462318279196));
#36681=CARTESIAN_POINT('Ctrl Pts',(0.109169995693685,0.174860979964985,
-0.295755769698662));
#36682=CARTESIAN_POINT('Ctrl Pts',(0.0406825029710331,0.202087565741548,
-0.292049221118129));
#36683=CARTESIAN_POINT('Ctrl Pts',(-0.0235591918084649,0.19429807846698,
-0.288342672537595));
#36684=CARTESIAN_POINT('Ctrl Pts',(-0.0878008865879639,0.186508591192413,
-0.284636123957062));
#36685=CARTESIAN_POINT('Ctrl Pts',(-0.147796783424309,0.143703030866715,
-0.280929575376528));
#36686=CARTESIAN_POINT('Ctrl Pts',(-0.176062917307789,0.0854905138682907,
-0.277223026795995));
#36687=CARTESIAN_POINT('Ctrl Pts',(-0.188864573152777,0.0591262218304634,
-0.275544340934805));
#36688=CARTESIAN_POINT('Ctrl Pts',(-0.195157947941312,0.029601716953994,
-0.273865655073614));
#36689=CARTESIAN_POINT('Ctrl Pts',(-0.195090438596196,4.99224700532782E-5,
-0.272186969212423));
#36690=CARTESIAN_POINT('Origin',(0.,0.,-0.56));
#36691=CARTESIAN_POINT('',(-0.195331947549774,-0.000176736735444216,-0.192013030787576));
#36692=CARTESIAN_POINT('',(-0.195362592747278,-0.00017879229733782,-0.202186969212423));
#36693=CARTESIAN_POINT('',(-0.1954,-2.39295984553393E-17,-0.56));
#36694=CARTESIAN_POINT('Ctrl Pts',(-0.195331947549774,-0.000176736735444216,
-0.192013030787576));
#36695=CARTESIAN_POINT('Ctrl Pts',(-0.194912364267956,0.0474440407802741,
-0.194726561641318));
#36696=CARTESIAN_POINT('Ctrl Pts',(-0.177373029739348,0.0953415099082568,
-0.19744009249506));
#36697=CARTESIAN_POINT('Ctrl Pts',(-0.14575529320444,0.130622265819019,
-0.200153623348801));
#36698=CARTESIAN_POINT('Ctrl Pts',(-0.102567033040916,0.178814028798557,
-0.203860171929335));
#36699=CARTESIAN_POINT('Ctrl Pts',(-0.0331110015127663,0.203465269351282,
-0.207566720509868));
#36700=CARTESIAN_POINT('Ctrl Pts',(0.0307951764230636,0.193283314489515,
-0.211273269090402));
#36701=CARTESIAN_POINT('Ctrl Pts',(0.0947013543588918,0.183101359627749,
-0.214979817670935));
#36702=CARTESIAN_POINT('Ctrl Pts',(0.153057678702401,0.138086209351492,
-0.218686366251468));
#36703=CARTESIAN_POINT('Ctrl Pts',(0.179131266631905,0.0788591893060497,
-0.222392914832002));
#36704=CARTESIAN_POINT('Ctrl Pts',(0.205204854561408,0.0196321692606077,
-0.226099463412535));
#36705=CARTESIAN_POINT('Ctrl Pts',(0.198995706076907,-0.0538067205540178,
-0.229806011993068));
#36706=CARTESIAN_POINT('Ctrl Pts',(0.163348216926586,-0.107815315807003,
-0.233512560573602));
#36707=CARTESIAN_POINT('Ctrl Pts',(0.127700727776265,-0.161823911059988,
-0.237219109154135));
#36708=CARTESIAN_POINT('Ctrl Pts',(0.0626148979601237,-0.196402211751331,
-0.240925657734668));
#36709=CARTESIAN_POINT('Ctrl Pts',(-0.00209362285706425,-0.19570998734557,
-0.244632206315201));
#36710=CARTESIAN_POINT('Ctrl Pts',(-0.0668021436742531,-0.195017762939809,
-0.248338754895735));
#36711=CARTESIAN_POINT('Ctrl Pts',(-0.13113335549249,-0.159055013436942,
-0.252045303476268));
#36712=CARTESIAN_POINT('Ctrl Pts',(-0.165617296475617,-0.104296181547444,
-0.255751852056802));
#36713=CARTESIAN_POINT('Ctrl Pts',(-0.185034292561122,-0.0734629300648085,
-0.257838911633726));
#36714=CARTESIAN_POINT('Ctrl Pts',(-0.194988156033035,-0.0366703457767274,
-0.259925971210651));
#36715=CARTESIAN_POINT('Ctrl Pts',(-0.195099694633333,6.61648413741722E-5,
-0.262013030787576));
#36716=CARTESIAN_POINT('Ctrl Pts',(-0.195090438596196,4.99224700532782E-5,
-0.272186969212423));
#36717=CARTESIAN_POINT('Ctrl Pts',(-0.195008886897137,-0.0356488248114389,
-0.270159106493081));
#36718=CARTESIAN_POINT('Ctrl Pts',(-0.185645032604243,-0.0713873952352632,
-0.268131243773738));
#36719=CARTESIAN_POINT('Ctrl Pts',(-0.167258709593931,-0.101643016872502,
-0.266103381054395));
#36720=CARTESIAN_POINT('Ctrl Pts',(-0.133651997065978,-0.156944556943723,
-0.262396832473862));
#36721=CARTESIAN_POINT('Ctrl Pts',(-0.069902201079457,-0.193928163415013,
-0.258690283893329));
#36722=CARTESIAN_POINT('Ctrl Pts',(-0.0052129381638058,-0.195651741864263,
-0.254983735312795));
#36723=CARTESIAN_POINT('Ctrl Pts',(0.0594763247518444,-0.197375320313514,
-0.251277186732262));
#36724=CARTESIAN_POINT('Ctrl Pts',(0.125105054596624,-0.163838870740725,
-0.247570638151728));
#36725=CARTESIAN_POINT('Ctrl Pts',(0.161608900190277,-0.110405353957066,
-0.243864089571195));
#36726=CARTESIAN_POINT('Ctrl Pts',(0.19811274578393,-0.0569718371734073,
-0.240157540990662));
#36727=CARTESIAN_POINT('Ctrl Pts',(0.205491707126456,0.016358746821123,
-0.236450992410128));
#36728=CARTESIAN_POINT('Ctrl Pts',(0.180365501023706,0.0759938475038011,
-0.232744443829595));
#36729=CARTESIAN_POINT('Ctrl Pts',(0.155239294920955,0.135628948186481,
-0.229037895249062));
#36730=CARTESIAN_POINT('Ctrl Pts',(0.0976079213729281,0.181568565557309,
-0.225331346668528));
#36731=CARTESIAN_POINT('Ctrl Pts',(0.0338721636032817,0.192767879526438,
-0.221624798087995));
#36732=CARTESIAN_POINT('Ctrl Pts',(-0.0298635941663648,0.203967193495566,
-0.217918249507461));
#36733=CARTESIAN_POINT('Ctrl Pts',(-0.0997037361576298,0.180426204062994,
-0.214211700926928));
#36734=CARTESIAN_POINT('Ctrl Pts',(-0.143654674518915,0.132928978123408,
-0.210505152346395));
#36735=CARTESIAN_POINT('Ctrl Pts',(-0.176532696237839,0.0973981138402943,
-0.207732424635071));
#36736=CARTESIAN_POINT('Ctrl Pts',(-0.194923208118132,0.0484614215119332,
-0.204959696923747));
#36737=CARTESIAN_POINT('Ctrl Pts',(-0.195362592747278,-0.00017879229733782,
-0.202186969212423));
#36738=CARTESIAN_POINT('Origin',(0.,0.,-0.56));
#36739=CARTESIAN_POINT('',(-0.195714505993407,3.28936632279161E-5,-0.122013030787576));
#36740=CARTESIAN_POINT('',(-0.195704662017859,5.15171773276178E-5,-0.132186969212423));
#36741=CARTESIAN_POINT('',(-0.1954,-2.39295984553393E-17,-0.56));
#36742=CARTESIAN_POINT('Ctrl Pts',(-0.195714505993407,3.28936632279162E-5,
-0.122013030787576));
#36743=CARTESIAN_POINT('Ctrl Pts',(-0.195718608760281,0.00179682927824294,
-0.122114054910918));
#36744=CARTESIAN_POINT('Ctrl Pts',(-0.195696828975953,0.00356066088435405,
-0.122215079034259));
#36745=CARTESIAN_POINT('Ctrl Pts',(-0.195648855912775,0.00532377956943465,
-0.122316103157601));
#36746=CARTESIAN_POINT('Ctrl Pts',(-0.193888736811089,0.0700121415501511,
-0.126022651738134));
#36747=CARTESIAN_POINT('Ctrl Pts',(-0.156868879881412,0.133740814262008,
-0.129729200318667));
#36748=CARTESIAN_POINT('Ctrl Pts',(-0.101548282882389,0.167316176473068,
-0.133435748899201));
#36749=CARTESIAN_POINT('Ctrl Pts',(-0.0462276858833664,0.200891538684129,
-0.137142297479734));
#36750=CARTESIAN_POINT('Ctrl Pts',(0.0273936511850024,0.204313590394393,
-0.140848846060268));
#36751=CARTESIAN_POINT('Ctrl Pts',(0.0855901404449638,0.176014531190619,
-0.144555394640801));
#36752=CARTESIAN_POINT('Ctrl Pts',(0.143786629704924,0.147715471986845,
-0.148261943221334));
#36753=CARTESIAN_POINT('Ctrl Pts',(0.186558271156478,0.0876953018690344,
-0.151968491801868));
#36754=CARTESIAN_POINT('Ctrl Pts',(0.194311404643603,0.0234491932800436,
-0.155675040382401));
#36755=CARTESIAN_POINT('Ctrl Pts',(0.202064538130729,-0.0407969153089472,
-0.159381588962934));
#36756=CARTESIAN_POINT('Ctrl Pts',(0.174799163653426,-0.109268962369118,
-0.163088137543468));
#36757=CARTESIAN_POINT('Ctrl Pts',(0.125005521700484,-0.150600126566253,
-0.166794686124001));
#36758=CARTESIAN_POINT('Ctrl Pts',(0.0752118797475406,-0.191931290763389,
-0.170501234704534));
#36759=CARTESIAN_POINT('Ctrl Pts',(0.00288997031895642,-0.206121572097488,
-0.174207783285068));
#36760=CARTESIAN_POINT('Ctrl Pts',(-0.0588297497046916,-0.186670415188142,
-0.177914331865601));
#36761=CARTESIAN_POINT('Ctrl Pts',(-0.120549469728339,-0.167219258278796,
-0.181620880446135));
#36762=CARTESIAN_POINT('Ctrl Pts',(-0.17166700034705,-0.114126663126006,
-0.185327429026668));
#36763=CARTESIAN_POINT('Ctrl Pts',(-0.188765521256956,-0.0517142228464369,
-0.189033977607201));
#36764=CARTESIAN_POINT('Ctrl Pts',(-0.193346368909845,-0.0349933683308803,
-0.190026995333993));
#36765=CARTESIAN_POINT('Ctrl Pts',(-0.195485494223524,-0.0176035797623098,
-0.191020013060785));
#36766=CARTESIAN_POINT('Ctrl Pts',(-0.195331947549774,-0.000176736735444216,
-0.192013030787576));
#36767=CARTESIAN_POINT('Ctrl Pts',(-0.195362592747278,-0.00017879229733782,
-0.202186969212423));
#36768=CARTESIAN_POINT('Ctrl Pts',(-0.195510572130406,-0.0165602229558212,
-0.201253148343214));
#36769=CARTESIAN_POINT('Ctrl Pts',(-0.193622426540463,-0.0329080252349692,
-0.200319327474004));
#36770=CARTESIAN_POINT('Ctrl Pts',(-0.189565844057378,-0.0486987641605954,
-0.199385506604795));
#36771=CARTESIAN_POINT('Ctrl Pts',(-0.17346434050325,-0.111375818058419,
-0.195678958024261));
#36772=CARTESIAN_POINT('Ctrl Pts',(-0.123199598663687,-0.165276463407468,
-0.191972409443728));
#36773=CARTESIAN_POINT('Ctrl Pts',(-0.0617977680446978,-0.185708952011097,
-0.188265860863195));
#36774=CARTESIAN_POINT('Ctrl Pts',(-0.000395937425709474,-0.206141440614726,
-0.184559312282662));
#36775=CARTESIAN_POINT('Ctrl Pts',(0.0721429819727052,-0.193105772472937,
-0.180852763702128));
#36776=CARTESIAN_POINT('Ctrl Pts',(0.122589101633872,-0.15257355742187,
-0.177146215121595));
#36777=CARTESIAN_POINT('Ctrl Pts',(0.17303522129504,-0.112041342370802,
-0.173439666541061));
#36778=CARTESIAN_POINT('Ctrl Pts',(0.20138854121896,-0.0440125804104571,
-0.169733117960528));
#36779=CARTESIAN_POINT('Ctrl Pts',(0.194660473879366,0.0203489363561378,
-0.166026569379995));
#36780=CARTESIAN_POINT('Ctrl Pts',(0.187932406539773,0.0847104531227328,
-0.162320020799461));
#36781=CARTESIAN_POINT('Ctrl Pts',(0.146122951936665,0.145404724695577,
-0.158613472218928));
#36782=CARTESIAN_POINT('Ctrl Pts',(0.0883849226421938,0.174627847866996,
-0.154906923638395));
#36783=CARTESIAN_POINT('Ctrl Pts',(0.0306468933477237,0.203850971038415,
-0.151200375057861));
#36784=CARTESIAN_POINT('Ctrl Pts',(-0.0430197106381098,0.201602945808412,
-0.147493826477328));
#36785=CARTESIAN_POINT('Ctrl Pts',(-0.0988684271343803,0.168913614382175,
-0.143787277896795));
#36786=CARTESIAN_POINT('Ctrl Pts',(-0.154717143630652,0.136224282955937,
-0.140080729316261));
#36787=CARTESIAN_POINT('Ctrl Pts',(-0.19274797263736,0.0730936453334647,
-0.136374180735728));
#36788=CARTESIAN_POINT('Ctrl Pts',(-0.195539054829503,0.0084416304927417,
-0.132667632155194));
#36789=CARTESIAN_POINT('Ctrl Pts',(-0.195659703437486,0.0056469526377488,
-0.132507411174271));
#36790=CARTESIAN_POINT('Ctrl Pts',(-0.195714505626837,0.00284943204833622,
-0.132347190193347));
#36791=CARTESIAN_POINT('Ctrl Pts',(-0.195704662017859,5.15171773276178E-5,
-0.132186969212423));
#36792=CARTESIAN_POINT('Origin',(0.,0.,-0.56));
#36793=CARTESIAN_POINT('',(-0.195233177397639,0.000155192514023357,-0.0520130307875762));
#36794=CARTESIAN_POINT('',(-0.195209575558751,0.00014773333329694,-0.0621869692124235));
#36795=CARTESIAN_POINT('',(-0.1954,-2.39295984553393E-17,-0.56));
#36796=CARTESIAN_POINT('Ctrl Pts',(-0.195233177397639,0.000155192514023357,
-0.0520130307875762));
#36797=CARTESIAN_POINT('Ctrl Pts',(-0.195394113464411,0.0211568636252984,
-0.053208096761051));
#36798=CARTESIAN_POINT('Ctrl Pts',(-0.192275975482653,0.0421126137721153,
-0.0544031627345257));
#36799=CARTESIAN_POINT('Ctrl Pts',(-0.185678101019284,0.0619073340238181,
-0.0555982287080004));
#36800=CARTESIAN_POINT('Ctrl Pts',(-0.165214509243147,0.1233015113157,-0.0593047772885337));
#36801=CARTESIAN_POINT('Ctrl Pts',(-0.111277350974912,0.17352708098491,
-0.0630113258690671));
#36802=CARTESIAN_POINT('Ctrl Pts',(-0.0485892744020614,0.189591048794179,
-0.0667178744496004));
#36803=CARTESIAN_POINT('Ctrl Pts',(0.0140988021707893,0.205655016603449,
-0.0704244230301338));
#36804=CARTESIAN_POINT('Ctrl Pts',(0.0855377970482562,0.187557382552778,
-0.0741309716106672));
#36805=CARTESIAN_POINT('Ctrl Pts',(0.133009133465254,0.143580642561344,
-0.0778375201912005));
#36806=CARTESIAN_POINT('Ctrl Pts',(0.180480469882252,0.0996039025699099,
-0.0815440687717339));
#36807=CARTESIAN_POINT('Ctrl Pts',(0.20398414783878,0.029748056637711,-0.0852506173522672));
#36808=CARTESIAN_POINT('Ctrl Pts',(0.192749285658678,-0.0339819211704,-0.0889571659328006));
#36809=CARTESIAN_POINT('Ctrl Pts',(0.181514423478577,-0.0977118989785101,
-0.0926637145133339));
#36810=CARTESIAN_POINT('Ctrl Pts',(0.135541021161846,-0.155316008662532,
-0.0963702630938673));
#36811=CARTESIAN_POINT('Ctrl Pts',(0.0758914272689859,-0.180408157931856,
-0.100076811674401));
#36812=CARTESIAN_POINT('Ctrl Pts',(0.0162418333761251,-0.205500307201181,
-0.103783360254934));
#36813=CARTESIAN_POINT('Ctrl Pts',(-0.0570839520928653,-0.198080496055805,
-0.107489908835468));
#36814=CARTESIAN_POINT('Ctrl Pts',(-0.110496654190512,-0.161546564858329,
-0.111196457416001));
#36815=CARTESIAN_POINT('Ctrl Pts',(-0.162453562228678,-0.12600838706628,
-0.114801981873193));
#36816=CARTESIAN_POINT('Ctrl Pts',(-0.195568079320075,-0.0629215056474345,
-0.118407506330385));
#36817=CARTESIAN_POINT('Ctrl Pts',(-0.195714505993407,3.28936632279162E-5,
-0.122013030787576));
#36818=CARTESIAN_POINT('Ctrl Pts',(-0.195704662017859,5.15171773276178E-5,
-0.132186969212423));
#36819=CARTESIAN_POINT('Ctrl Pts',(-0.195486783797436,-0.0618774678483191,
-0.128640641612814));
#36820=CARTESIAN_POINT('Ctrl Pts',(-0.163598090938826,-0.123999616539142,
-0.125094314013204));
#36821=CARTESIAN_POINT('Ctrl Pts',(-0.113057776887832,-0.159764585797867,
-0.121547986413594));
#36822=CARTESIAN_POINT('Ctrl Pts',(-0.0602340813764411,-0.197145395188781,
-0.117841437833061));
#36823=CARTESIAN_POINT('Ctrl Pts',(0.0129646450239196,-0.205733621911635,
-0.114134889252528));
#36824=CARTESIAN_POINT('Ctrl Pts',(0.0730063821891976,-0.181595212509884,
-0.110428340671994));
#36825=CARTESIAN_POINT('Ctrl Pts',(0.133048119354474,-0.157456803108133,
-0.106721792091461));
#36826=CARTESIAN_POINT('Ctrl Pts',(0.179932867284669,-0.10059175758178,
-0.103015243510927));
#36827=CARTESIAN_POINT('Ctrl Pts',(0.192182602645457,-0.0370494424593577,
-0.0993086949303943));
#36828=CARTESIAN_POINT('Ctrl Pts',(0.204432338006246,0.0264928726630671,
-0.0956021463498609));
#36829=CARTESIAN_POINT('Ctrl Pts',(0.182047060797625,0.0967124573815599,
-0.0918955977693276));
#36830=CARTESIAN_POINT('Ctrl Pts',(0.13528186872857,0.141441209413879,-0.0881890491887942));
#36831=CARTESIAN_POINT('Ctrl Pts',(0.0885166766595161,0.186169961446195,
-0.0844825006082609));
#36832=CARTESIAN_POINT('Ctrl Pts',(0.0173715697300292,0.205407880792338,
-0.0807759520277275));
#36833=CARTESIAN_POINT('Ctrl Pts',(-0.0455629389330441,0.190343444572713,
-0.0770694034471942));
#36834=CARTESIAN_POINT('Ctrl Pts',(-0.10849744759612,0.175279008353088,
-0.0733628548666607));
#36835=CARTESIAN_POINT('Ctrl Pts',(-0.163221357992783,0.125912216567692,
-0.0696563062861274));
#36836=CARTESIAN_POINT('Ctrl Pts',(-0.184664120209359,0.0648553589225613,
-0.065949757705594));
#36837=CARTESIAN_POINT('Ctrl Pts',(-0.191920158828329,0.0441942653306371,
-0.0646954948745371));
#36838=CARTESIAN_POINT('Ctrl Pts',(-0.195365223212996,0.0221945598750925,
-0.0634412320434803));
#36839=CARTESIAN_POINT('Ctrl Pts',(-0.195209575558751,0.00014773333329694,
-0.0621869692124235));
#36840=CARTESIAN_POINT('Origin',(0.,0.,-1.18400562256037));
#36841=CARTESIAN_POINT('',(-0.155417199305029,0.000123542454221778,-0.0290056225603694));
#36842=CARTESIAN_POINT('',(-0.155328879770405,-0.00016163609193072,-0.0151943774396288));
#36843=CARTESIAN_POINT('',(-0.15555,-1.32567133817862E-14,-1.18400562256037));
#36844=CARTESIAN_POINT('',(0.133820452603638,-0.0798000960230315,1.68903200041158E-16));
#36845=CARTESIAN_POINT('Ctrl Pts',(-0.155417199305029,0.000123542454221769,
-0.0290056225603694));
#36846=CARTESIAN_POINT('Ctrl Pts',(-0.15514796082327,-0.0350112670250425,
-0.0264941399533108));
#36847=CARTESIAN_POINT('Ctrl Pts',(-0.125938607687929,-0.122399182856573,
-0.020276108765719));
#36848=CARTESIAN_POINT('Ctrl Pts',(0.0152304203843597,-0.181290024202016,
-0.0106075679122624));
#36849=CARTESIAN_POINT('Ctrl Pts',(0.109031119236811,-0.120890131481052,
-0.00345050966586446));
#36850=CARTESIAN_POINT('Ctrl Pts',(0.133822070517494,-0.0798006560480846,
1.69216854070675E-16));
#36851=CARTESIAN_POINT('',(-0.0319621170202048,-0.15223082991164,0.));
#36852=CARTESIAN_POINT('Origin',(0.,0.,0.));
#36853=CARTESIAN_POINT('Ctrl Pts',(-0.155328879770405,-0.000161636091930716,
-0.0151943774396288));
#36854=CARTESIAN_POINT('Ctrl Pts',(-0.155437349196103,-0.0191858047064336,
-0.0138361335402858));
#36855=CARTESIAN_POINT('Ctrl Pts',(-0.143394445718357,-0.0899409694934188,
-0.00877134106040959));
#36856=CARTESIAN_POINT('Ctrl Pts',(-0.0826091653404253,-0.141597064818995,
-0.00370654858053334));
#36857=CARTESIAN_POINT('Ctrl Pts',(-0.0319621170202048,-0.15223082991164,
0.));
#36858=CARTESIAN_POINT('Origin',(0.,0.,-1.18400562256037));
#36859=CARTESIAN_POINT('',(-0.155800365441527,2.61853086679489E-5,-0.0990056225603694));
#36860=CARTESIAN_POINT('',(-0.155398410840142,0.000117604503539592,-0.0851943774396291));
#36861=CARTESIAN_POINT('',(-0.15555,-1.32567133817862E-14,-1.18400562256037));
#36862=CARTESIAN_POINT('Ctrl Pts',(-0.155800365441527,2.61853086679508E-5,
-0.0990056225603694));
#36863=CARTESIAN_POINT('Ctrl Pts',(-0.155683801116874,-0.0500892538559854,
-0.0954000981031777));
#36864=CARTESIAN_POINT('Ctrl Pts',(-0.102222939106085,-0.151938211910091,
-0.0880880250654528));
#36865=CARTESIAN_POINT('Ctrl Pts',(0.0713011418186189,-0.169497054292766,
-0.0770694034471942));
#36866=CARTESIAN_POINT('Ctrl Pts',(0.181093814239817,-0.0319281812935353,
-0.065949757705594));
#36867=CARTESIAN_POINT('Ctrl Pts',(0.124962845363592,0.134900019854162,
-0.0548301119639941));
#36868=CARTESIAN_POINT('Ctrl Pts',(-0.045646197418241,0.178120393087247,
-0.0437104662223939));
#36869=CARTESIAN_POINT('Ctrl Pts',(-0.145364369674128,0.0852641476206765,
-0.0351023030878524));
#36870=CARTESIAN_POINT('Ctrl Pts',(-0.155545313968215,0.0168421194314946,
-0.0302006885338442));
#36871=CARTESIAN_POINT('Ctrl Pts',(-0.155417199305029,0.000123542454221769,
-0.0290056225603694));
#36872=CARTESIAN_POINT('Ctrl Pts',(-0.155398410840142,0.00011760450353957,
-0.0851943774396291));
#36873=CARTESIAN_POINT('Ctrl Pts',(-0.155156157062649,-0.0341966101071686,
-0.0827420916901529));
#36874=CARTESIAN_POINT('Ctrl Pts',(-0.127029144573819,-0.120735747049266,
-0.0765832573601433));
#36875=CARTESIAN_POINT('Ctrl Pts',(0.0160916033347015,-0.183170692569655,
-0.0667178744496004));
#36876=CARTESIAN_POINT('Ctrl Pts',(0.16268430194739,-0.0857519355616629,
-0.0555982287080002));
#36877=CARTESIAN_POINT('Ctrl Pts',(0.160190409020898,0.0902865901057441,
-0.0444785829664002));
#36878=CARTESIAN_POINT('Ctrl Pts',(0.0109996935541243,0.183501383580361,
-0.0333589372248001));
#36879=CARTESIAN_POINT('Ctrl Pts',(-0.12893036588142,0.117918227652547,
-0.023597535382543));
#36880=CARTESIAN_POINT('Ctrl Pts',(-0.155141344041178,0.0327297645135169,
-0.0175426821208192));
#36881=CARTESIAN_POINT('Ctrl Pts',(-0.155328879770405,-0.000161636091930716,
-0.0151943774396288));
#36882=CARTESIAN_POINT('Origin',(0.,0.,-1.18400562256037));
#36883=CARTESIAN_POINT('',(-0.155495826209659,-0.00014069293346625,-0.16900562256037));
#36884=CARTESIAN_POINT('',(-0.1557925290526,4.10107314749147E-5,-0.155194377439629));
#36885=CARTESIAN_POINT('',(-0.15555,-1.32567133817862E-14,-1.18400562256037));
#36886=CARTESIAN_POINT('Ctrl Pts',(-0.155495826209659,-0.000140692933466274,
-0.16900562256037));
#36887=CARTESIAN_POINT('Ctrl Pts',(-0.155618058477324,-0.0140134945344324,
-0.168012604833578));
#36888=CARTESIAN_POINT('Ctrl Pts',(-0.147559034213969,-0.0795284632520187,
-0.163313038526253));
#36889=CARTESIAN_POINT('Ctrl Pts',(-0.0552719453863964,-0.175381314233795,
-0.154906923638395));
#36890=CARTESIAN_POINT('Ctrl Pts',(0.117445654587239,-0.141492395172598,
-0.143787277896795));
#36891=CARTESIAN_POINT('Ctrl Pts',(0.182560224698972,0.0220310478193626,
-0.132667632155195));
#36892=CARTESIAN_POINT('Ctrl Pts',(0.0804139274452977,0.165369903425689,
-0.121547986413595));
#36893=CARTESIAN_POINT('Ctrl Pts',(-0.0954069371552854,0.157197434487125,
-0.110428340671994));
#36894=CARTESIAN_POINT('Ctrl Pts',(-0.155150166767694,0.054351096265153,
-0.102914219387586));
#36895=CARTESIAN_POINT('Ctrl Pts',(-0.155803631487522,0.00143038277497305,
-0.0991066466837111));
#36896=CARTESIAN_POINT('Ctrl Pts',(-0.155800365441527,2.61853086679508E-5,
-0.0990056225603694));
#36897=CARTESIAN_POINT('Ctrl Pts',(-0.1557925290526,4.10107314749112E-5,
-0.155194377439629));
#36898=CARTESIAN_POINT('Ctrl Pts',(-0.155619085054709,-0.0492581377881695,
-0.15164804984002));
#36899=CARTESIAN_POINT('Ctrl Pts',(-0.103701607366211,-0.150398227879575,
-0.144395173659877));
#36900=CARTESIAN_POINT('Ctrl Pts',(0.0685911587771073,-0.170612914816246,
-0.133435748899201));
#36901=CARTESIAN_POINT('Ctrl Pts',(0.180560286830463,-0.0348090586500559,
-0.122316103157601));
#36902=CARTESIAN_POINT('Ctrl Pts',(0.127100258123179,0.132887815499814,
-0.111196457416001));
#36903=CARTESIAN_POINT('Ctrl Pts',(-0.0428069278985511,0.17883139309898,
-0.100076811674401));
#36904=CARTESIAN_POINT('Ctrl Pts',(-0.144675382459758,0.0869352045888443,
-0.0914094516822767));
#36905=CARTESIAN_POINT('Ctrl Pts',(-0.155522315613008,0.0176681872495837,
-0.0864486402706862));
#36906=CARTESIAN_POINT('Ctrl Pts',(-0.155398410840142,0.00011760450353957,
-0.0851943774396291));
#36907=CARTESIAN_POINT('Origin',(0.,0.,-1.18400562256037));
#36908=CARTESIAN_POINT('',(-0.155310939100384,5.26711416314951E-5,-0.23900562256037));
#36909=CARTESIAN_POINT('',(-0.155520221606136,-0.000142329282771692,-0.225194377439629));
#36910=CARTESIAN_POINT('',(-0.15555,-1.32567133817862E-14,-1.18400562256037));
#36911=CARTESIAN_POINT('Ctrl Pts',(-0.155310939100384,5.2671141631511E-5,
-0.23900562256037));
#36912=CARTESIAN_POINT('Ctrl Pts',(-0.155222147753012,-0.029191772188182,
-0.236918562983445));
#36913=CARTESIAN_POINT('Ctrl Pts',(-0.133225757910032,-0.110497290353548,
-0.231124954825986));
#36914=CARTESIAN_POINT('Ctrl Pts',(-0.00196700844525682,-0.183874200155875,
-0.221624798087995));
#36915=CARTESIAN_POINT('Ctrl Pts',(0.153469544695492,-0.101295059840545,
-0.210505152346395));
#36916=CARTESIAN_POINT('Ctrl Pts',(0.168298097102307,0.074090088224943,
-0.199385506604795));
#36917=CARTESIAN_POINT('Ctrl Pts',(0.0289328015296395,0.181594284112427,
-0.188265860863195));
#36918=CARTESIAN_POINT('Ctrl Pts',(-0.122127581727067,0.12798013767017,
-0.178139232848387));
#36919=CARTESIAN_POINT('Ctrl Pts',(-0.155161813008602,0.0377682729957565,
-0.171719153414111));
#36920=CARTESIAN_POINT('Ctrl Pts',(-0.155495826209659,-0.000140692933466274,
-0.16900562256037));
#36921=CARTESIAN_POINT('Ctrl Pts',(-0.155520221606136,-0.00014232928277169,
-0.225194377439629));
#36922=CARTESIAN_POINT('Ctrl Pts',(-0.155638021979962,-0.0131829205771748,
-0.22426055657042));
#36923=CARTESIAN_POINT('Ctrl Pts',(-0.148168893704103,-0.0778515737263976,
-0.219620187120677));
#36924=CARTESIAN_POINT('Ctrl Pts',(-0.0580604758392629,-0.174477990107862,
-0.211273269090402));
#36925=CARTESIAN_POINT('Ctrl Pts',(0.115175382590983,-0.143346492982138,
-0.200153623348801));
#36926=CARTESIAN_POINT('Ctrl Pts',(0.182888160188203,0.0191183062440436,
-0.189033977607201));
#36927=CARTESIAN_POINT('Ctrl Pts',(0.0830397364904521,0.164067036179902,
-0.177914331865601));
#36928=CARTESIAN_POINT('Ctrl Pts',(-0.0928892335709049,0.158698351565871,
-0.166794686124001));
#36929=CARTESIAN_POINT('Ctrl Pts',(-0.154747501165264,0.0560145032920222,
-0.15922136798201));
#36930=CARTESIAN_POINT('Ctrl Pts',(-0.155800365149716,0.00226831706815041,
-0.155354598420553));
#36931=CARTESIAN_POINT('Ctrl Pts',(-0.1557925290526,4.10107314749112E-5,
-0.155194377439629));
#36932=CARTESIAN_POINT('Origin',(0.,0.,-1.18400562256037));
#36933=CARTESIAN_POINT('',(-0.155689062743399,0.000115235607110945,-0.30900562256037));
#36934=CARTESIAN_POINT('',(-0.155303570745334,3.97412498162469E-5,-0.295194377439629));
#36935=CARTESIAN_POINT('',(-0.15555,-1.32567133817862E-14,-1.18400562256037));
#36936=CARTESIAN_POINT('Ctrl Pts',(-0.155689062743399,0.000115235607110934,
-0.30900562256037));
#36937=CARTESIAN_POINT('Ctrl Pts',(-0.155321871925874,-0.0441841658980628,
-0.305824521133312));
#36938=CARTESIAN_POINT('Ctrl Pts',(-0.112320239215782,-0.140723170785617,
-0.29893687112572));
#36939=CARTESIAN_POINT('Ctrl Pts',(0.0515074258588442,-0.176523583699745,
-0.288342672537596));
#36940=CARTESIAN_POINT('Ctrl Pts',(0.176269718137531,-0.0523696188850282,
-0.277223026795995));
#36941=CARTESIAN_POINT('Ctrl Pts',(0.139534607376368,0.119765119560166,
-0.266103381054396));
#36942=CARTESIAN_POINT('Ctrl Pts',(-0.0250413882421251,0.182171675645894,
-0.254983735312795));
#36943=CARTESIAN_POINT('Ctrl Pts',(-0.140091288211346,0.0972868755983294,
-0.24595114914812));
#36944=CARTESIAN_POINT('Ctrl Pts',(-0.155379838240722,0.0227453891229129,
-0.240625111563978));
#36945=CARTESIAN_POINT('Ctrl Pts',(-0.155310939100384,5.2671141631511E-5,
-0.23900562256037));
#36946=CARTESIAN_POINT('Ctrl Pts',(-0.155303570745334,3.97412498162556E-5,
-0.295194377439629));
#36947=CARTESIAN_POINT('Ctrl Pts',(-0.155238650751531,-0.028378580856813,
-0.293166514720287));
#36948=CARTESIAN_POINT('Ctrl Pts',(-0.134159631932849,-0.10882985390664,
-0.287432103420411));
#36949=CARTESIAN_POINT('Ctrl Pts',(-0.00489767969399011,-0.183819477000074,
-0.277991143540001));
#36950=CARTESIAN_POINT('Ctrl Pts',(0.151835415403586,-0.103728462705588,
-0.266871497798402));
#36951=CARTESIAN_POINT('Ctrl Pts',(0.169457689254605,0.0713980317726476,
-0.255751852056801));
#36952=CARTESIAN_POINT('Ctrl Pts',(0.0318237052925425,0.181110019726059,
-0.244632206315202));
#36953=CARTESIAN_POINT('Ctrl Pts',(-0.120960013984837,0.129611271034686,
-0.23444638144281));
#36954=CARTESIAN_POINT('Ctrl Pts',(-0.155170445357094,0.0385781684553703,
-0.227967105150953));
#36955=CARTESIAN_POINT('Ctrl Pts',(-0.155520221606136,-0.00014232928277169,
-0.225194377439629));
#36956=CARTESIAN_POINT('Origin',(0.,0.,-1.18400562256037));
#36957=CARTESIAN_POINT('',(-0.155672476465762,-0.000121209602746091,-0.37900562256037));
#36958=CARTESIAN_POINT('',(-0.155666155856283,0.000123253288390569,-0.365194377439629));
#36959=CARTESIAN_POINT('',(-0.15555,-1.32567133817862E-14,-1.18400562256037));
#36960=CARTESIAN_POINT('Ctrl Pts',(-0.155672476465762,-0.000121209602746106,
-0.37900562256037));
#36961=CARTESIAN_POINT('Ctrl Pts',(-0.155740414797244,-0.0080415446494063,
-0.378437027863712));
#36962=CARTESIAN_POINT('Ctrl Pts',(-0.151588537816422,-0.067521436921519,
-0.374161884586521));
#36963=CARTESIAN_POINT('Ctrl Pts',(-0.0749118080055823,-0.167933949932374,
-0.366180192728796));
#36964=CARTESIAN_POINT('Ctrl Pts',(0.100543725038754,-0.153962819777854,
-0.355060546987196));
#36965=CARTESIAN_POINT('Ctrl Pts',(0.183881617795998,0.00106824867117576,
-0.343940901245595));
#36966=CARTESIAN_POINT('Ctrl Pts',(0.0987481244286207,0.155120593218137,
-0.332821255503996));
#36967=CARTESIAN_POINT('Ctrl Pts',(-0.0768578892449788,0.167052253441001,
-0.321701609762395));
#36968=CARTESIAN_POINT('Ctrl Pts',(-0.151954637124841,0.0663032413753942,
-0.313763065447854));
#36969=CARTESIAN_POINT('Ctrl Pts',(-0.155749714493831,0.0074325107570195,
-0.309531069713845));
#36970=CARTESIAN_POINT('Ctrl Pts',(-0.155689062743399,0.000115235607110934,
-0.30900562256037));
#36971=CARTESIAN_POINT('Ctrl Pts',(-0.155666155856283,0.00012325328839057,
-0.365194377439629));
#36972=CARTESIAN_POINT('Ctrl Pts',(-0.155289020277978,-0.0433684186858502,
-0.362072472870154));
#36973=CARTESIAN_POINT('Ctrl Pts',(-0.113636956063751,-0.139129528685827,
-0.355244019720144));
#36974=CARTESIAN_POINT('Ctrl Pts',(0.0486871260286323,-0.177322167638905,
-0.344709017989602));
#36975=CARTESIAN_POINT('Ctrl Pts',(0.175412553298172,-0.0551726700606049,
-0.333589372248002));
#36976=CARTESIAN_POINT('Ctrl Pts',(0.141425907488028,0.117525742149486,
-0.322469726506402));
#36977=CARTESIAN_POINT('Ctrl Pts',(-0.0221344224967506,0.182547677935732,
-0.311350080764802));
#36978=CARTESIAN_POINT('Ctrl Pts',(-0.139285522744779,0.0989633204492847,
-0.302258297742544));
#36979=CARTESIAN_POINT('Ctrl Pts',(-0.155357312191768,0.023564724013264,
-0.29687306330082));
#36980=CARTESIAN_POINT('Ctrl Pts',(-0.155303570745334,3.97412498162556E-5,
-0.295194377439629));
#36981=CARTESIAN_POINT('Origin',(0.,0.,-1.18400562256037));
#36982=CARTESIAN_POINT('',(-0.155305368154442,-4.32865829287516E-5,-0.44900562256037));
#36983=CARTESIAN_POINT('',(-0.155695065503602,-0.00011283858791146,-0.435194377439629));
#36984=CARTESIAN_POINT('',(-0.15555,-1.32567133817862E-14,-1.18400562256037));
#36985=CARTESIAN_POINT('Ctrl Pts',(-0.155305368154442,-4.32865829287695E-5,
-0.44900562256037));
#36986=CARTESIAN_POINT('Ctrl Pts',(-0.15536338193547,-0.023342686153529,
-0.447342986013579));
#36987=CARTESIAN_POINT('Ctrl Pts',(-0.139505759847756,-0.098508885666548,
-0.441973800886254));
#36988=CARTESIAN_POINT('Ctrl Pts',(-0.0229231396891714,-0.182450322513706,
-0.432898067178396));
#36989=CARTESIAN_POINT('Ctrl Pts',(0.140916678082541,-0.118135855508594,
-0.421778421436797));
#36990=CARTESIAN_POINT('Ctrl Pts',(0.175649365031236,0.0544140706314786,
-0.410658775695196));
#36991=CARTESIAN_POINT('Ctrl Pts',(0.0494530132129136,0.177110107003317,
-0.399539129953596));
#36992=CARTESIAN_POINT('Ctrl Pts',(-0.113282157194832,0.139562230312325,
-0.388988078908654));
#36993=CARTESIAN_POINT('Ctrl Pts',(-0.155297539181982,0.0435894445193366,
-0.382143576444245));
#36994=CARTESIAN_POINT('Ctrl Pts',(-0.155672476465762,-0.000121209602746106,
-0.37900562256037));
#36995=CARTESIAN_POINT('Ctrl Pts',(-0.155695065503602,-0.000112838587911464,
-0.435194377439629));
#36996=CARTESIAN_POINT('Ctrl Pts',(-0.155752997892932,-0.00720589989722735,
-0.434684979600554));
#36997=CARTESIAN_POINT('Ctrl Pts',(-0.152088815062267,-0.0658502493267181,
-0.430469033180945));
#36998=CARTESIAN_POINT('Ctrl Pts',(-0.0775791235918538,-0.166718526143494,
-0.422546538180803));
#36999=CARTESIAN_POINT('Ctrl Pts',(0.098076807463925,-0.1555459006674,-0.411426892439203));
#37000=CARTESIAN_POINT('Ctrl Pts',(0.183875275341805,-0.00186292638295208,
-0.400307246697602));
#37001=CARTESIAN_POINT('Ctrl Pts',(0.101208168018179,0.153526851407609,
-0.389187600956003));
#37002=CARTESIAN_POINT('Ctrl Pts',(-0.0741853388097491,0.168256122867715,
-0.378067955214402));
#37003=CARTESIAN_POINT('Ctrl Pts',(-0.151450355425137,0.0679746909538998,
-0.370070214042278));
#37004=CARTESIAN_POINT('Ctrl Pts',(-0.155736782633081,0.00826800755129776,
-0.365779021450687));
#37005=CARTESIAN_POINT('Ctrl Pts',(-0.155666155856283,0.00012325328839057,
-0.365194377439629));
#37006=CARTESIAN_POINT('Origin',(0.,0.,-1.18400562256037));
#37007=CARTESIAN_POINT('',(-0.155513557532958,0.000142022966550295,-0.51900562256037));
#37008=CARTESIAN_POINT('',(-0.155313283030358,-5.6100541927756E-5,-0.505194377439629));
#37009=CARTESIAN_POINT('',(-0.15555,-1.32567133817862E-14,-1.18400562256037));
#37010=CARTESIAN_POINT('Ctrl Pts',(-0.155513557532958,0.000142022966550288,
-0.51900562256037));
#37011=CARTESIAN_POINT('Ctrl Pts',(-0.155167810588833,-0.0383585585219179,
-0.516248944163445));
#37012=CARTESIAN_POINT('Ctrl Pts',(-0.121278654951446,-0.129169493585072,
-0.509785717185988));
#37013=CARTESIAN_POINT('Ctrl Pts',(0.0310407000630972,-0.181245870182351,
-0.499615941627997));
#37014=CARTESIAN_POINT('Ctrl Pts',(0.169147551063838,-0.0721297198640855,
-0.488496295886397));
#37015=CARTESIAN_POINT('Ctrl Pts',(0.152282291589484,0.103071306321499,
-0.477376650144796));
#37016=CARTESIAN_POINT('Ctrl Pts',(-0.00410321495424111,0.183838935336354,
-0.466257004403197));
#37017=CARTESIAN_POINT('Ctrl Pts',(-0.133908341240762,0.109282116163178,
-0.456799995208387));
#37018=CARTESIAN_POINT('Ctrl Pts',(-0.155234050664522,0.028599126729369,
-0.451049534594112));
#37019=CARTESIAN_POINT('Ctrl Pts',(-0.155305368154442,-4.32865829287695E-5,
-0.44900562256037));
#37020=CARTESIAN_POINT('Ctrl Pts',(-0.155313283030358,-5.6100541927763E-5,
-0.505194377439629));
#37021=CARTESIAN_POINT('Ctrl Pts',(-0.15538600368638,-0.0225230806948092,
-0.50359093775042));
#37022=CARTESIAN_POINT('Ctrl Pts',(-0.140306651967032,-0.096832232461837,
-0.498280949480678));
#37023=CARTESIAN_POINT('Ctrl Pts',(-0.0258284510112228,-0.182061743634136,
-0.489264412630403));
#37024=CARTESIAN_POINT('Ctrl Pts',(0.139015704615632,-0.120367027241518,
-0.478144766888803));
#37025=CARTESIAN_POINT('Ctrl Pts',(0.176494391467026,0.0516073362752325,
-0.467025121147203));
#37026=CARTESIAN_POINT('Ctrl Pts',(0.0522698307062849,0.176299325508287,
-0.455905475405603));
#37027=CARTESIAN_POINT('Ctrl Pts',(-0.111959433833773,0.141154106954363,
-0.445295227503078));
#37028=CARTESIAN_POINT('Ctrl Pts',(-0.155331462505528,0.0444055799932159,
-0.438391528181087));
#37029=CARTESIAN_POINT('Ctrl Pts',(-0.155695065503602,-0.000112838587911464,
-0.435194377439629));
#37030=CARTESIAN_POINT('Origin',(0.,0.,-1.18400562256037));
#37031=CARTESIAN_POINT('',(-0.155794948693578,-3.70111496645316E-5,-0.589005622560369));
#37032=CARTESIAN_POINT('',(-0.15548930789199,0.000140015377334053,-0.575194377439629));
#37033=CARTESIAN_POINT('',(-0.15555,-1.32567133817862E-14,-1.18400562256037));
#37034=CARTESIAN_POINT('Ctrl Pts',(-0.155794948693578,-3.70111496645414E-5,
-0.58900562256037));
#37035=CARTESIAN_POINT('Ctrl Pts',(-0.155801375060938,-0.00204112484285652,
-0.588861450893845));
#37036=CARTESIAN_POINT('Ctrl Pts',(-0.15485797915675,-0.0555633522856045,
-0.585010730646788));
#37037=CARTESIAN_POINT('Ctrl Pts',(-0.0935742393001708,-0.15829545874079,
-0.577453461819198));
#37038=CARTESIAN_POINT('Ctrl Pts',(0.0823299191069159,-0.164424374526445,
-0.566333816077597));
#37039=CARTESIAN_POINT('Ctrl Pts',(0.182803831914859,-0.0199085297249743,
-0.555214170335998));
#37040=CARTESIAN_POINT('Ctrl Pts',(0.115793820441273,0.142847406928437,
-0.544094524594397));
#37041=CARTESIAN_POINT('Ctrl Pts',(-0.057305889765134,0.174727288987128,
-0.532974878852797));
#37042=CARTESIAN_POINT('Ctrl Pts',(-0.148005123032518,0.0783061562763419,
-0.524611911508121));
#37043=CARTESIAN_POINT('Ctrl Pts',(-0.155632691746678,0.0134081893965227,
-0.519955492743979));
#37044=CARTESIAN_POINT('Ctrl Pts',(-0.155513557532958,0.000142022966550288,
-0.51900562256037));
#37045=CARTESIAN_POINT('Ctrl Pts',(-0.15548930789199,0.000140015377334046,
-0.575194377439629));
#37046=CARTESIAN_POINT('Ctrl Pts',(-0.155159975094503,-0.037548743133565,
-0.572496895900287));
#37047=CARTESIAN_POINT('Ctrl Pts',(-0.122440493891221,-0.127537141042073,
-0.566092865780412));
#37048=CARTESIAN_POINT('Ctrl Pts',(0.028147729041889,-0.181717618096114,
-0.555982287080003));
#37049=CARTESIAN_POINT('Ctrl Pts',(0.167976319009287,-0.0748167336150888,
-0.544862641338404));
#37050=CARTESIAN_POINT('Ctrl Pts',(0.153905875245583,0.100630854819146,
-0.533742995596803));
#37051=CARTESIAN_POINT('Ctrl Pts',(-0.00117233452664475,0.183880975112975,
-0.522623349855203));
#37052=CARTESIAN_POINT('Ctrl Pts',(-0.132969246133086,0.11094901835971,
-0.513107143802813));
#37053=CARTESIAN_POINT('Ctrl Pts',(-0.15521790092195,0.0294121145950307,
-0.507297486330954));
#37054=CARTESIAN_POINT('Ctrl Pts',(-0.155313283030358,-5.6100541927763E-5,
-0.505194377439629));
#37055=CARTESIAN_POINT('Origin',(0.,0.,-1.18400562256037));
#37056=CARTESIAN_POINT('',(-0.15540393784838,-0.000119995988950991,-0.65900562256037));
#37057=CARTESIAN_POINT('',(-0.155801839037753,-2.20116907670709E-5,-0.645194377439629));
#37058=CARTESIAN_POINT('',(-0.15555,-1.32567133817862E-14,-1.18400562256037));
#37059=CARTESIAN_POINT('Ctrl Pts',(-0.15540393784838,-0.000119995988950999,
-0.65900562256037));
#37060=CARTESIAN_POINT('Ctrl Pts',(-0.155528444664855,-0.0174441538003097,
-0.657767409043713));
#37061=CARTESIAN_POINT('Ctrl Pts',(-0.144860866850051,-0.0864786497960442,
-0.652822646946522));
#37062=CARTESIAN_POINT('Ctrl Pts',(-0.0435801783122908,-0.178645902770777,
-0.644171336268797));
#37063=CARTESIAN_POINT('Ctrl Pts',(0.126525183886544,-0.133435259062113,
-0.633051690527199));
#37064=CARTESIAN_POINT('Ctrl Pts',(0.180708827729641,0.0340280781002357,
-0.621932044785597));
#37065=CARTESIAN_POINT('Ctrl Pts',(0.0693279792777336,0.170315066297202,
-0.610812399043998));
#37066=CARTESIAN_POINT('Ctrl Pts',(-0.103303156215773,0.150816403206739,
-0.599836924968922));
#37067=CARTESIAN_POINT('Ctrl Pts',(-0.155636157834885,0.0494831790916029,
-0.592567999474379));
#37068=CARTESIAN_POINT('Ctrl Pts',(-0.155794948693578,-3.70111496645414E-5,
-0.58900562256037));
#37069=CARTESIAN_POINT('Ctrl Pts',(-0.155801839037753,-2.20116907670611E-5,
-0.645194377439629));
#37070=CARTESIAN_POINT('Ctrl Pts',(-0.155804177189137,-0.00120309644097989,
-0.645109402630688));
#37071=CARTESIAN_POINT('Ctrl Pts',(-0.155256813551466,-0.0539001433168381,
-0.641317879241212));
#37072=CARTESIAN_POINT('Ctrl Pts',(-0.0960855472312445,-0.156783784206156,
-0.633819807271204));
#37073=CARTESIAN_POINT('Ctrl Pts',(0.0796985611215568,-0.165715801092974,
-0.622700161529604));
#37074=CARTESIAN_POINT('Ctrl Pts',(0.182463260436913,-0.0228198590591629,
-0.611580515788004));
#37075=CARTESIAN_POINT('Ctrl Pts',(0.118056065295367,0.140983519688348,
-0.600460870046404));
#37076=CARTESIAN_POINT('Ctrl Pts',(-0.054513485600872,0.175618527679694,
-0.589341224304804));
#37077=CARTESIAN_POINT('Ctrl Pts',(-0.14739093441373,0.0799831865833066,
-0.580919060102545));
#37078=CARTESIAN_POINT('Ctrl Pts',(-0.155612503868192,0.0142385304114906,
-0.576203444480821));
#37079=CARTESIAN_POINT('Ctrl Pts',(-0.15548930789199,0.000140015377334046,
-0.575194377439629));
#37080=CARTESIAN_POINT('Origin',(0.,0.,-1.18400562256037));
#37081=CARTESIAN_POINT('',(-0.155362436352018,9.99900651833539E-5,-0.72900562256037));
#37082=CARTESIAN_POINT('',(-0.155424369060156,-0.000126926758710719,-0.715194377439629));
#37083=CARTESIAN_POINT('',(-0.15555,-1.32567133817862E-14,-1.18400562256037));
#37084=CARTESIAN_POINT('Ctrl Pts',(-0.155362436352018,9.99900651833512E-5,
-0.72900562256037));
#37085=CARTESIAN_POINT('Ctrl Pts',(-0.155170334697732,-0.032553096980618,
-0.72667336719358));
#37086=CARTESIAN_POINT('Ctrl Pts',(-0.129150367964797,-0.117380331222216,
-0.720634563246256));
#37087=CARTESIAN_POINT('Ctrl Pts',(0.0101689670613149,-0.183603329566334,
-0.710889210718397));
#37088=CARTESIAN_POINT('Ctrl Pts',(0.159818411126364,-0.0909486997130359,
-0.6997695649768));
#37089=CARTESIAN_POINT('Ctrl Pts',(0.163043054468382,0.0850326579052167,
-0.688649919235197));
#37090=CARTESIAN_POINT('Ctrl Pts',(0.0168884954843339,0.183107534631158,
-0.677530273493599));
#37091=CARTESIAN_POINT('Ctrl Pts',(-0.126741374559613,0.121180173616676,
-0.667648841268655));
#37092=CARTESIAN_POINT('Ctrl Pts',(-0.155155737892023,0.0344151028471008,
-0.661473957624246));
#37093=CARTESIAN_POINT('Ctrl Pts',(-0.15540393784838,-0.000119995988950999,
-0.65900562256037));
#37094=CARTESIAN_POINT('Ctrl Pts',(-0.155424369060156,-0.000126926758710741,
-0.715194377439629));
#37095=CARTESIAN_POINT('Ctrl Pts',(-0.155550893466124,-0.0166173779854387,
-0.714015360780554));
#37096=CARTESIAN_POINT('Ctrl Pts',(-0.145538034253706,-0.0848002269033668,
-0.709129795540946));
#37097=CARTESIAN_POINT('Ctrl Pts',(-0.0464222225043185,-0.177928537998713,
-0.700537681720804));
#37098=CARTESIAN_POINT('Ctrl Pts',(0.124382169793526,-0.135435088561476,
-0.689418035979205));
#37099=CARTESIAN_POINT('Ctrl Pts',(0.181228262157198,0.0311432877610799,
-0.678298390237604));
#37100=CARTESIAN_POINT('Ctrl Pts',(0.0720339590899123,0.169188345090688,
-0.667178744496004));
#37101=CARTESIAN_POINT('Ctrl Pts',(-0.101818695314802,0.152353556505981,
-0.656144073563346));
#37102=CARTESIAN_POINT('Ctrl Pts',(-0.155702188472728,0.0503150894650411,
-0.648815951211221));
#37103=CARTESIAN_POINT('Ctrl Pts',(-0.155801839037753,-2.20116907670611E-5,
-0.645194377439629));
#37104=CARTESIAN_POINT('Origin',(0.,0.,-1.18400562256037));
#37105=CARTESIAN_POINT('',(-0.155767789804036,6.93381960118415E-5,-0.79900562256037));
#37106=CARTESIAN_POINT('',(-0.155347070724463,8.97218886615411E-5,-0.78519437743963));
#37107=CARTESIAN_POINT('',(-0.15555,-1.32567133817862E-14,-1.18400562256037));
#37108=CARTESIAN_POINT('Ctrl Pts',(-0.155767789804036,6.93381960118404E-5,
-0.79900562256037));
#37109=CARTESIAN_POINT('Ctrl Pts',(-0.155502544361867,-0.0475813235126791,
-0.795579325343446));
#37110=CARTESIAN_POINT('Ctrl Pts',(-0.106628930778583,-0.147250628696526,
-0.78844647954599));
#37111=CARTESIAN_POINT('Ctrl Pts',(0.0630419049178878,-0.172740582625397,
-0.777607085167998));
#37112=CARTESIAN_POINT('Ctrl Pts',(0.179340890619455,-0.0406255492142766,
-0.766487439426399));
#37113=CARTESIAN_POINT('Ctrl Pts',(0.131328683099859,0.128710402067756,
-0.755367793684797));
#37114=CARTESIAN_POINT('Ctrl Pts',(-0.037006185026792,0.180122549393705,
-0.7442481479432));
#37115=CARTESIAN_POINT('Ctrl Pts',(-0.14324057853946,0.0903372148411208,
-0.735460757568388));
#37116=CARTESIAN_POINT('Ctrl Pts',(-0.155475633218705,0.0193409859585915,
-0.730379915774113));
#37117=CARTESIAN_POINT('Ctrl Pts',(-0.155362436352018,9.99900651833512E-5,
-0.72900562256037));
#37118=CARTESIAN_POINT('Ctrl Pts',(-0.155347070724463,8.9721888661529E-5,
-0.78519437743963));
#37119=CARTESIAN_POINT('Ctrl Pts',(-0.155180081869041,-0.0317424574751034,
-0.782921318930421));
#37120=CARTESIAN_POINT('Ctrl Pts',(-0.13016521763349,-0.115722480957532,
-0.776941711840679));
#37121=CARTESIAN_POINT('Ctrl Pts',(0.00724107137421544,-0.183742086289102,
-0.767255556170406));
#37122=CARTESIAN_POINT('Ctrl Pts',(0.158348393578249,-0.0934846169015645,
-0.756135910428804));
#37123=CARTESIAN_POINT('Ctrl Pts',(0.164377737792651,0.0824229744011697,
-0.745016264687206));
#37124=CARTESIAN_POINT('Ctrl Pts',(0.0198050495896289,0.182815063350545,
-0.733896618945604));
#37125=CARTESIAN_POINT('Ctrl Pts',(-0.125659926754502,0.122827779940055,
-0.72395598986308));
#37126=CARTESIAN_POINT('Ctrl Pts',(-0.155153130759608,0.0352246872782868,
-0.717721909361088));
#37127=CARTESIAN_POINT('Ctrl Pts',(-0.155424369060156,-0.000126926758710741,
-0.715194377439629));
#37128=CARTESIAN_POINT('Origin',(0.,0.,-1.18400562256037));
#37129=CARTESIAN_POINT('',(-0.155570908001796,-0.000141339127694456,-0.86900562256037));
#37130=CARTESIAN_POINT('',(-0.155751765103858,8.20881598970168E-5,-0.855194377439629));
#37131=CARTESIAN_POINT('',(-0.15555,-1.32567133817862E-14,-1.18400562256037));
#37132=CARTESIAN_POINT('Ctrl Pts',(-0.155570908001796,-0.000141339127694456,
-0.86900562256037));
#37133=CARTESIAN_POINT('Ctrl Pts',(-0.15567590648691,-0.0114962743919849,
-0.868191832073847));
#37134=CARTESIAN_POINT('Ctrl Pts',(-0.149357049078014,-0.0744533324005729,
-0.863671493006789));
#37135=CARTESIAN_POINT('Ctrl Pts',(-0.0636687064710734,-0.17251058084216,
-0.8554446053592));
#37136=CARTESIAN_POINT('Ctrl Pts',(0.110482893512257,-0.146993649357098,
-0.844324959617598));
#37137=CARTESIAN_POINT('Ctrl Pts',(0.18341044091426,0.0131980997397562,
-0.833205313875999));
#37138=CARTESIAN_POINT('Ctrl Pts',(0.0882983957762384,0.161297819676871,
-0.822085668134399));
#37139=CARTESIAN_POINT('Ctrl Pts',(-0.0877122368719845,0.161617311611651,
-0.810966022392799));
#37140=CARTESIAN_POINT('Ctrl Pts',(-0.153888977708246,0.0593911412520667,
-0.803272673868122));
#37141=CARTESIAN_POINT('Ctrl Pts',(-0.155789485352365,0.00396688767152082,
-0.79928587392398));
#37142=CARTESIAN_POINT('Ctrl Pts',(-0.155767789804036,6.93381960118404E-5,
-0.79900562256037));
#37143=CARTESIAN_POINT('Ctrl Pts',(-0.155751765103858,8.20881598970159E-5,
-0.85519437743963));
#37144=CARTESIAN_POINT('Ctrl Pts',(-0.155452044257622,-0.0467580259285011,
-0.851827277080288));
#37145=CARTESIAN_POINT('Ctrl Pts',(-0.108038257994642,-0.14568622625586,
-0.844753628140413));
#37146=CARTESIAN_POINT('Ctrl Pts',(0.060280446378822,-0.173723506052108,
-0.833973430620006));
#37147=CARTESIAN_POINT('Ctrl Pts',(0.178670530140934,-0.0434790462684611,
-0.822853784878404));
#37148=CARTESIAN_POINT('Ctrl Pts',(0.133363614212077,0.126600688351419,
-0.811734139136806));
#37149=CARTESIAN_POINT('Ctrl Pts',(-0.0341303623589111,0.180689528985939,
-0.800614493395204));
#37150=CARTESIAN_POINT('Ctrl Pts',(-0.142507620182121,0.0920156013334908,
-0.791767906162814));
#37151=CARTESIAN_POINT('Ctrl Pts',(-0.155452381197247,0.0201644858605286,
-0.786627867510955));
#37152=CARTESIAN_POINT('Ctrl Pts',(-0.155347070724463,8.9721888661529E-5,
-0.78519437743963));
#37153=CARTESIAN_POINT('Origin',(0.,0.,-1.18400562256037));
#37154=CARTESIAN_POINT('',(-0.15529890300355,1.25102102450688E-5,-0.93900562256037));
#37155=CARTESIAN_POINT('',(-0.155595980901295,-0.000138704452836119,-0.925194377439629));
#37156=CARTESIAN_POINT('',(-0.15555,-1.32567133817862E-14,-1.18400562256037));
#37157=CARTESIAN_POINT('Ctrl Pts',(-0.15529890300355,1.25102102450734E-5,
-0.93900562256037));
#37158=CARTESIAN_POINT('Ctrl Pts',(-0.155277540336578,-0.0267273135833239,
-0.937097790223713));
#37159=CARTESIAN_POINT('Ctrl Pts',(-0.135987452190703,-0.105443411679473,
-0.931483409306522));
#37160=CARTESIAN_POINT('Ctrl Pts',(-0.0108405547554956,-0.183565275721231,
-0.922162479808802));
#37161=CARTESIAN_POINT('Ctrl Pts',(0.148406703733419,-0.108580977171968,
-0.911042834067198));
#37162=CARTESIAN_POINT('Ctrl Pts',(0.171675085100322,0.0658845155887245,
-0.899923188325601));
#37163=CARTESIAN_POINT('Ctrl Pts',(0.037660590930604,0.179987027118587,
-0.888803542583998));
#37164=CARTESIAN_POINT('Ctrl Pts',(-0.118527703919238,0.132904165366808,
-0.878497687328924));
#37165=CARTESIAN_POINT('Ctrl Pts',(-0.155197672847659,0.0402217290534668,
-0.87189838065438));
#37166=CARTESIAN_POINT('Ctrl Pts',(-0.155570908001796,-0.000141339127694456,
-0.86900562256037));
#37167=CARTESIAN_POINT('Ctrl Pts',(-0.155595980901295,-0.000138704452836098,
-0.925194377439629));
#37168=CARTESIAN_POINT('Ctrl Pts',(-0.155692996261753,-0.010663309100421,
-0.924439783810688));
#37169=CARTESIAN_POINT('Ctrl Pts',(-0.149918881858646,-0.0727785826548655,
-0.919978641601213));
#37170=CARTESIAN_POINT('Ctrl Pts',(-0.0664110274107763,-0.171473678917601,
-0.911810950811206));
#37171=CARTESIAN_POINT('Ctrl Pts',(0.108126128703887,-0.148736101992464,
-0.900691305069605));
#37172=CARTESIAN_POINT('Ctrl Pts',(0.183597333320993,0.010272923727082,
-0.889571659328006));
#37173=CARTESIAN_POINT('Ctrl Pts',(0.0908583219823267,0.15986984368347,
-0.878452013586405));
#37174=CARTESIAN_POINT('Ctrl Pts',(-0.0851249865183533,0.162994896424521,
-0.867332367844806));
#37175=CARTESIAN_POINT('Ctrl Pts',(-0.153444406068025,0.0610581867156833,
-0.859579822462547));
#37176=CARTESIAN_POINT('Ctrl Pts',(-0.155781980926748,0.00480419077368596,
-0.855533825660821));
#37177=CARTESIAN_POINT('Ctrl Pts',(-0.155751765103858,8.20881598970159E-5,
-0.85519437743963));
#37178=CARTESIAN_POINT('Origin',(0.,0.,-1.18400562256037));
#37179=CARTESIAN_POINT('',(-0.15555,-1.32567133817862E-14,-1.));
#37180=CARTESIAN_POINT('',(-0.155319281545194,2.55672115835603E-6,-0.995194377439629));
#37181=CARTESIAN_POINT('',(-0.15555,-1.32567133817862E-14,-1.18400562256037));
#37182=CARTESIAN_POINT('',(-0.107438039834496,-0.112484977203719,-1.));
#37183=CARTESIAN_POINT('Origin',(0.,0.,-1.));
#37184=CARTESIAN_POINT('Ctrl Pts',(-0.107438039834496,-0.112484977203719,
-1.));
#37185=CARTESIAN_POINT('Ctrl Pts',(-0.070014397862351,-0.148229508046032,
-0.996293451419467));
#37186=CARTESIAN_POINT('Ctrl Pts',(0.0426645675892999,-0.178810969987729,
-0.988880354258401));
#37187=CARTESIAN_POINT('Ctrl Pts',(0.173668580798161,-0.0608101377048221,
-0.977760708516799));
#37188=CARTESIAN_POINT('Ctrl Pts',(0.145082536077593,0.112893009936692,
-0.9666410627752));
#37189=CARTESIAN_POINT('Ctrl Pts',(-0.016188327655916,0.183168151262569,
-0.9555214170336));
#37190=CARTESIAN_POINT('Ctrl Pts',(-0.137605454051508,0.102359736842961,
-0.946309603628658));
#37191=CARTESIAN_POINT('Ctrl Pts',(-0.155319043859408,0.0252229831075507,
-0.940804338804247));
#37192=CARTESIAN_POINT('Ctrl Pts',(-0.15529890300355,1.25102102450734E-5,
-0.93900562256037));
#37193=CARTESIAN_POINT('Ctrl Pts',(-0.155319281545194,2.55672115836644E-6,
-0.995194377439629));
#37194=CARTESIAN_POINT('Ctrl Pts',(-0.155306686282912,-0.0259101337848701,
-0.993345741960555));
#37195=CARTESIAN_POINT('Ctrl Pts',(-0.136821575085788,-0.103778540630361,
-0.987790557900947));
#37196=CARTESIAN_POINT('Ctrl Pts',(-0.0137950195410933,-0.183363935742736,
-0.978528825260807));
#37197=CARTESIAN_POINT('Ctrl Pts',(0.14667274202516,-0.110935491613379,
-0.967409179519206));
#37198=CARTESIAN_POINT('Ctrl Pts',(0.172695229799944,0.0631411111612149,
-0.956289533777606));
#37199=CARTESIAN_POINT('Ctrl Pts',(0.0405290837896907,0.179363093540042,
-0.945169888036005));
#37200=CARTESIAN_POINT('Ctrl Pts',(-0.117297335950851,0.134520793240012,
-0.934804835923348));
#37201=CARTESIAN_POINT('Ctrl Pts',(-0.155216458781444,0.0410333351873348,
-0.928146332391221));
#37202=CARTESIAN_POINT('Ctrl Pts',(-0.155595980901295,-0.000138704452836098,
-0.925194377439629));
#37203=CARTESIAN_POINT('Ctrl Pts',(0.124290537174079,0.0935289520361411,
-1.02300740822721));
#37204=CARTESIAN_POINT('Ctrl Pts',(0.0931735462474481,0.134880292271595,
-1.01930085964667));
#37205=CARTESIAN_POINT('Ctrl Pts',(-0.013037262777072,0.183367614985409,
-1.01188776248561));
#37206=CARTESIAN_POINT('Ctrl Pts',(-0.161477093702181,0.0882259055140853,
-1.00076811674401));
#37207=CARTESIAN_POINT('Ctrl Pts',(-0.161500828769186,-0.0878136284471678,
-0.989648471002406));
#37208=CARTESIAN_POINT('Ctrl Pts',(-0.0137950195410933,-0.183363935742736,
-0.978528825260807));
#37209=CARTESIAN_POINT('Ctrl Pts',(0.14667274202516,-0.110935491613379,
-0.967409179519206));
#37210=CARTESIAN_POINT('Ctrl Pts',(0.172695229799944,0.0631411111612149,
-0.956289533777606));
#37211=CARTESIAN_POINT('Ctrl Pts',(0.0405290837896907,0.179363093540042,
-0.945169888036005));
#37212=CARTESIAN_POINT('Ctrl Pts',(-0.128787370879799,0.131256196618047,
-0.934050242294407));
#37213=CARTESIAN_POINT('Ctrl Pts',(-0.180100169418625,-0.0371083441993324,
-0.922930596552805));
#37214=CARTESIAN_POINT('Ctrl Pts',(-0.0664110274107763,-0.171473678917601,
-0.911810950811206));
#37215=CARTESIAN_POINT('Ctrl Pts',(0.108126128703887,-0.148736101992464,
-0.900691305069605));
#37216=CARTESIAN_POINT('Ctrl Pts',(0.183597333320993,0.010272923727082,
-0.889571659328006));
#37217=CARTESIAN_POINT('Ctrl Pts',(0.0908583219823267,0.15986984368347,
-0.878452013586405));
#37218=CARTESIAN_POINT('Ctrl Pts',(-0.0851249865183533,0.162994896424521,
-0.867332367844806));
#37219=CARTESIAN_POINT('Ctrl Pts',(-0.183117027223152,0.016784839709399,
-0.856212722103206));
#37220=CARTESIAN_POINT('Ctrl Pts',(-0.113338298618642,-0.144803384848188,
-0.845093076361605));
#37221=CARTESIAN_POINT('Ctrl Pts',(0.060280446378822,-0.173723506052108,
-0.833973430620006));
#37222=CARTESIAN_POINT('Ctrl Pts',(0.178670530140934,-0.0434790462684611,
-0.822853784878404));
#37223=CARTESIAN_POINT('Ctrl Pts',(0.133363614212077,0.126600688351419,
-0.811734139136806));
#37224=CARTESIAN_POINT('Ctrl Pts',(-0.0341303623589111,0.180689528985939,
-0.800614493395204));
#37225=CARTESIAN_POINT('Ctrl Pts',(-0.170354273544413,0.0692315581199349,
-0.789494847653606));
#37226=CARTESIAN_POINT('Ctrl Pts',(-0.150500483525886,-0.105656007506409,
-0.778375201912004));
#37227=CARTESIAN_POINT('Ctrl Pts',(0.00724107137421544,-0.183742086289102,
-0.767255556170406));
#37228=CARTESIAN_POINT('Ctrl Pts',(0.158348393578249,-0.0934846169015645,
-0.756135910428804));
#37229=CARTESIAN_POINT('Ctrl Pts',(0.164377737792651,0.0824229744011697,
-0.745016264687206));
#37230=CARTESIAN_POINT('Ctrl Pts',(0.0198050495896289,0.182815063350545,
-0.733896618945604));
#37231=CARTESIAN_POINT('Ctrl Pts',(-0.142912922414824,0.115712937822271,
-0.722776973204005));
#37232=CARTESIAN_POINT('Ctrl Pts',(-0.174694814920481,-0.0574047821953129,
-0.711657327462404));
#37233=CARTESIAN_POINT('Ctrl Pts',(-0.0464222225043185,-0.177928537998713,
-0.700537681720804));
#37234=CARTESIAN_POINT('Ctrl Pts',(0.124382169793526,-0.135435088561476,
-0.689418035979205));
#37235=CARTESIAN_POINT('Ctrl Pts',(0.181228262157198,0.0311432877610799,
-0.678298390237604));
#37236=CARTESIAN_POINT('Ctrl Pts',(0.0720339590899123,0.169188345090688,
-0.667178744496004));
#37237=CARTESIAN_POINT('Ctrl Pts',(-0.103157484317412,0.152223916668754,
-0.656059098754404));
#37238=CARTESIAN_POINT('Ctrl Pts',(-0.183836574721314,-0.00420727602229024,
-0.644939453012804));
#37239=CARTESIAN_POINT('Ctrl Pts',(-0.0960855472312445,-0.156783784206156,
-0.633819807271204));
#37240=CARTESIAN_POINT('Ctrl Pts',(0.0796985611215568,-0.165715801092974,
-0.622700161529604));
#37241=CARTESIAN_POINT('Ctrl Pts',(0.182463260436913,-0.0228198590591629,
-0.611580515788004));
#37242=CARTESIAN_POINT('Ctrl Pts',(0.118056065295367,0.140983519688348,
-0.600460870046404));
#37243=CARTESIAN_POINT('Ctrl Pts',(-0.054513485600872,0.175618527679694,
-0.589341224304804));
#37244=CARTESIAN_POINT('Ctrl Pts',(-0.177138063248702,0.0493527499258254,
-0.578221578563203));
#37245=CARTESIAN_POINT('Ctrl Pts',(-0.137469664530806,-0.122129761772175,
-0.567101932821604));
#37246=CARTESIAN_POINT('Ctrl Pts',(0.028147729041889,-0.181717618096114,
-0.555982287080003));
#37247=CARTESIAN_POINT('Ctrl Pts',(0.167976319009287,-0.0748167336150888,
-0.544862641338404));
#37248=CARTESIAN_POINT('Ctrl Pts',(0.153905875245583,0.100630854819146,
-0.533742995596803));
#37249=CARTESIAN_POINT('Ctrl Pts',(-0.00117233452664475,0.183880975112975,
-0.522623349855203));
#37250=CARTESIAN_POINT('Ctrl Pts',(-0.155176457475656,0.0986602981043884,
-0.511503704113604));
#37251=CARTESIAN_POINT('Ctrl Pts',(-0.167008713555752,-0.0769524331856614,
-0.500384058372002));
#37252=CARTESIAN_POINT('Ctrl Pts',(-0.0258284510112228,-0.182061743634136,
-0.489264412630403));
#37253=CARTESIAN_POINT('Ctrl Pts',(0.139015704615632,-0.120367027241518,
-0.478144766888803));
#37254=CARTESIAN_POINT('Ctrl Pts',(0.176494391467026,0.0516073362752325,
-0.467025121147203));
#37255=CARTESIAN_POINT('Ctrl Pts',(0.0522698307062849,0.176299325508287,
-0.455905475405603));
#37256=CARTESIAN_POINT('Ctrl Pts',(-0.11984407830563,0.139466785550596,
-0.444785829664003));
#37257=CARTESIAN_POINT('Ctrl Pts',(-0.182157463300752,-0.0251445011995766,
-0.433666183922403));
#37258=CARTESIAN_POINT('Ctrl Pts',(-0.0775791235918538,-0.166718526143494,
-0.422546538180803));
#37259=CARTESIAN_POINT('Ctrl Pts',(0.098076807463925,-0.1555459006674,-0.411426892439203));
#37260=CARTESIAN_POINT('Ctrl Pts',(0.183875275341805,-0.00186292638295208,
-0.400307246697602));
#37261=CARTESIAN_POINT('Ctrl Pts',(0.101208168018179,0.153526851407609,
-0.389187600956003));
#37262=CARTESIAN_POINT('Ctrl Pts',(-0.0741853388097491,0.168256122867715,
-0.378067955214402));
#37263=CARTESIAN_POINT('Ctrl Pts',(-0.181610622335615,0.0288300057499716,
-0.366948309472803));
#37264=CARTESIAN_POINT('Ctrl Pts',(-0.122645194018816,-0.137010013359534,
-0.355828663731202));
#37265=CARTESIAN_POINT('Ctrl Pts',(0.0486871260286323,-0.177322167638905,
-0.344709017989602));
#37266=CARTESIAN_POINT('Ctrl Pts',(0.175412553298172,-0.0551726700606049,
-0.333589372248002));
#37267=CARTESIAN_POINT('Ctrl Pts',(0.141425907488028,0.117525742149486,
-0.322469726506402));
#37268=CARTESIAN_POINT('Ctrl Pts',(-0.0221344224967506,0.182547677935732,
-0.311350080764802));
#37269=CARTESIAN_POINT('Ctrl Pts',(-0.165415309183955,0.0803203763697784,
-0.300230435023202));
#37270=CARTESIAN_POINT('Ctrl Pts',(-0.157143546107041,-0.0954960381063839,
-0.289110789281602));
#37271=CARTESIAN_POINT('Ctrl Pts',(-0.00489767969399011,-0.183819477000074,
-0.277991143540001));
#37272=CARTESIAN_POINT('Ctrl Pts',(0.151835415403586,-0.103728462705588,
-0.266871497798402));
#37273=CARTESIAN_POINT('Ctrl Pts',(0.169457689254605,0.0713980317726476,
-0.255751852056801));
#37274=CARTESIAN_POINT('Ctrl Pts',(0.0318237052925425,0.181110019726059,
-0.244632206315202));
#37275=CARTESIAN_POINT('Ctrl Pts',(-0.134966992047393,0.12488994440001,
-0.233512560573601));
#37276=CARTESIAN_POINT('Ctrl Pts',(-0.178101631312305,-0.0457536495135279,
-0.222392914832001));
#37277=CARTESIAN_POINT('Ctrl Pts',(-0.0580604758392629,-0.174477990107862,
-0.211273269090402));
#37278=CARTESIAN_POINT('Ctrl Pts',(0.115175382590983,-0.143346492982138,
-0.200153623348801));
#37279=CARTESIAN_POINT('Ctrl Pts',(0.182888160188203,0.0191183062440436,
-0.189033977607201));
#37280=CARTESIAN_POINT('Ctrl Pts',(0.0830397364904521,0.164067036179902,
-0.177914331865601));
#37281=CARTESIAN_POINT('Ctrl Pts',(-0.0928892335709049,0.158698351565871,
-0.166794686124001));
#37282=CARTESIAN_POINT('Ctrl Pts',(-0.183713626385541,0.00793114559592943,
-0.155675040382401));
#37283=CARTESIAN_POINT('Ctrl Pts',(-0.106220436282912,-0.150102699871419,
-0.144555394640801));
#37284=CARTESIAN_POINT('Ctrl Pts',(0.0685911587771073,-0.170612914816246,
-0.133435748899201));
#37285=CARTESIAN_POINT('Ctrl Pts',(0.180560286830463,-0.0348090586500559,
-0.122316103157601));
#37286=CARTESIAN_POINT('Ctrl Pts',(0.127100258123179,0.132887815499814,
-0.111196457416001));
#37287=CARTESIAN_POINT('Ctrl Pts',(-0.0428069278985511,0.17883139309898,
-0.100076811674401));
#37288=CARTESIAN_POINT('Ctrl Pts',(-0.173497372046971,0.0609347022767939,
-0.0889571659328004));
#37289=CARTESIAN_POINT('Ctrl Pts',(-0.145225197994402,-0.112797907004394,
-0.0778375201912004));
#37290=CARTESIAN_POINT('Ctrl Pts',(0.0160916033347015,-0.183170692569655,
-0.0667178744496004));
#37291=CARTESIAN_POINT('Ctrl Pts',(0.16268430194739,-0.0857519355616629,
-0.0555982287080002));
#37292=CARTESIAN_POINT('Ctrl Pts',(0.160190409020898,0.0902865901057441,
-0.0444785829664002));
#37293=CARTESIAN_POINT('Ctrl Pts',(0.0109996935541243,0.183501383580361,
-0.0333589372248001));
#37294=CARTESIAN_POINT('Ctrl Pts',(-0.148400842830771,0.108792702151384,
-0.0222392914832001));
#37295=CARTESIAN_POINT('Ctrl Pts',(-0.171577704761274,-0.0659904817000804,
-0.0111196457416));
#37296=CARTESIAN_POINT('Ctrl Pts',(-0.0826091653404253,-0.141597064818995,
-0.00370654858053334));
#37297=CARTESIAN_POINT('Ctrl Pts',(-0.0319621170202048,-0.15223082991164,
0.));
#37298=CARTESIAN_POINT('Ctrl Pts',(0.134904440327165,0.101515941725715,
-1.01533827215147));
#37299=CARTESIAN_POINT('Ctrl Pts',(0.101130185737347,0.146398517166105,
-1.01163172357094));
#37300=CARTESIAN_POINT('Ctrl Pts',(-0.0141505916566728,0.199026458780906,
-1.00421862640987));
#37301=CARTESIAN_POINT('Ctrl Pts',(-0.175266576578065,0.0957600367360653,
-0.99309898066827));
#37302=CARTESIAN_POINT('Ctrl Pts',(-0.175292338522647,-0.0953125528950821,
-0.981979334926671));
#37303=CARTESIAN_POINT('Ctrl Pts',(-0.0149730577468432,-0.199022465345967,
-0.970859689185071));
#37304=CARTESIAN_POINT('Ctrl Pts',(0.159197993862087,-0.120408928537827,
-0.95974004344347));
#37305=CARTESIAN_POINT('Ctrl Pts',(0.18744269558271,0.0685331036176038,
-0.94862039770187));
#37306=CARTESIAN_POINT('Ctrl Pts',(0.043990101659657,0.194679967594623,
-0.937500751960271));
#37307=CARTESIAN_POINT('Ctrl Pts',(-0.139785285225796,0.142464938577181,
-0.92638110621867));
#37308=CARTESIAN_POINT('Ctrl Pts',(-0.195479986736384,-0.0402772449093781,
-0.915261460477071));
#37309=CARTESIAN_POINT('Ctrl Pts',(-0.0720822573311022,-0.186116829254826,
-0.90414181473547));
#37310=CARTESIAN_POINT('Ctrl Pts',(0.117359657534594,-0.161437556325261,
-0.89302216899387));
#37311=CARTESIAN_POINT('Ctrl Pts',(0.19927579412211,0.0111501893662626,
-0.88190252325227));
#37312=CARTESIAN_POINT('Ctrl Pts',(0.098617250796205,0.173522073986237,
-0.87078287751067));
#37313=CARTESIAN_POINT('Ctrl Pts',(-0.092394311950167,0.176913993440523,
-0.859663231769071));
#37314=CARTESIAN_POINT('Ctrl Pts',(-0.198754471849409,0.0182181963201783,
-0.848543586027468));
#37315=CARTESIAN_POINT('Ctrl Pts',(-0.123016925426643,-0.157169001233487,
-0.837423940285871));
#37316=CARTESIAN_POINT('Ctrl Pts',(0.0654281497715049,-0.188558782418071,
-0.826304294544269));
#37317=CARTESIAN_POINT('Ctrl Pts',(0.193928262115897,-0.0471919788599082,
-0.815184648802669));
#37318=CARTESIAN_POINT('Ctrl Pts',(0.144752321008073,0.137411868959591,
-0.80406500306107));
#37319=CARTESIAN_POINT('Ctrl Pts',(-0.0370449556086742,0.196119675198496,
-0.792945357319469));
#37320=CARTESIAN_POINT('Ctrl Pts',(-0.184901831244498,0.0751436498183813,
-0.781825711577869));
#37321=CARTESIAN_POINT('Ctrl Pts',(-0.163352608820018,-0.114678598097066,
-0.770706065836269));
#37322=CARTESIAN_POINT('Ctrl Pts',(0.00785942923184284,-0.199432908401222,
-0.75958642009467));
#37323=CARTESIAN_POINT('Ctrl Pts',(0.17187069826933,-0.101467820552112,
-0.748466774353069));
#37324=CARTESIAN_POINT('Ctrl Pts',(0.178414923801518,0.0894615590575204,
-0.737347128611469));
#37325=CARTESIAN_POINT('Ctrl Pts',(0.0214963197624508,0.19842672149802,
-0.726227482869868));
#37326=CARTESIAN_POINT('Ctrl Pts',(-0.155117101045983,0.125594349098855,
-0.71510783712827));
#37327=CARTESIAN_POINT('Ctrl Pts',(-0.189613037088232,-0.0623069156368273,
-0.703988191386669));
#37328=CARTESIAN_POINT('Ctrl Pts',(-0.0503864902998775,-0.193122906881706,
-0.692868545645069));
#37329=CARTESIAN_POINT('Ctrl Pts',(0.135003897997258,-0.147000690788359,
-0.681748899903469));
#37330=CARTESIAN_POINT('Ctrl Pts',(0.196704413977544,0.0338027970662945,
-0.670629254161869));
#37331=CARTESIAN_POINT('Ctrl Pts',(0.0781853643609582,0.183636337272974,
-0.659509608420269));
#37332=CARTESIAN_POINT('Ctrl Pts',(-0.111966711254192,0.16522321609927,
-0.648389962678668));
#37333=CARTESIAN_POINT('Ctrl Pts',(-0.199535465758804,-0.0045665601741977,
-0.637270316937069));
#37334=CARTESIAN_POINT('Ctrl Pts',(-0.10429085968633,-0.170172477660811,
-0.626150671195469));
#37335=CARTESIAN_POINT('Ctrl Pts',(0.086504492034861,-0.179867252230991,
-0.615031025453868));
#37336=CARTESIAN_POINT('Ctrl Pts',(0.198044876055494,-0.0247685816210578,
-0.603911379712269));
#37337=CARTESIAN_POINT('Ctrl Pts',(0.128137570067725,0.153022935223718,
-0.592791733970668));
#37338=CARTESIAN_POINT('Ctrl Pts',(-0.0591687141473076,0.190615631136323,
-0.581672088229069));
#37339=CARTESIAN_POINT('Ctrl Pts',(-0.192264928823459,0.0535672727685228,
-0.570552442487468));
#37340=CARTESIAN_POINT('Ctrl Pts',(-0.149209011217944,-0.132559143549997,
-0.559432796745868));
#37341=CARTESIAN_POINT('Ctrl Pts',(0.0305514298933165,-0.197235558910708,
-0.548313151004268));
#37342=CARTESIAN_POINT('Ctrl Pts',(0.182320809125048,-0.0812057764406795,
-0.537193505262669));
#37343=CARTESIAN_POINT('Ctrl Pts',(0.167048807054298,0.109224317938277,
-0.526073859521067));
#37344=CARTESIAN_POINT('Ctrl Pts',(-0.00127244709684963,0.199583657762181,
-0.514954213779468));
#37345=CARTESIAN_POINT('Ctrl Pts',(-0.168427891806321,0.107085483745576,
-0.503834568037868));
#37346=CARTESIAN_POINT('Ctrl Pts',(-0.181270574126195,-0.083523856013151,
-0.492714922296267));
#37347=CARTESIAN_POINT('Ctrl Pts',(-0.0280340950116467,-0.197609071361169,
-0.481595276554668));
#37348=CARTESIAN_POINT('Ctrl Pts',(0.150887076798065,-0.130645878705303,
-0.470475630813067));
#37349=CARTESIAN_POINT('Ctrl Pts',(0.19156629010618,0.0560143915641372,
-0.459355985071468));
#37350=CARTESIAN_POINT('Ctrl Pts',(0.056733460308012,0.191354566312969,
-0.448236339329867));
#37351=CARTESIAN_POINT('Ctrl Pts',(-0.130078272070719,0.151376678198602,
-0.437116693588267));
#37352=CARTESIAN_POINT('Ctrl Pts',(-0.197712965095534,-0.0272917386854921,
-0.425997047846668));
#37353=CARTESIAN_POINT('Ctrl Pts',(-0.0842040632149887,-0.180955605896666,
-0.414877402105067));
#37354=CARTESIAN_POINT('Ctrl Pts',(0.106452165392644,-0.168828883934509,
-0.403757756363467));
#37355=CARTESIAN_POINT('Ctrl Pts',(0.199577471253882,-0.00202201267109366,
-0.392638110621867));
#37356=CARTESIAN_POINT('Ctrl Pts',(0.109850931321565,0.166637416131906,
-0.381518464880267));
#37357=CARTESIAN_POINT('Ctrl Pts',(-0.0805204631032623,0.182624507087749,
-0.370398819138667));
#37358=CARTESIAN_POINT('Ctrl Pts',(-0.197119426150196,0.0312919702397112,
-0.359279173397067));
#37359=CARTESIAN_POINT('Ctrl Pts',(-0.133118591600838,-0.148710107717997,
-0.348159527655467));
#37360=CARTESIAN_POINT('Ctrl Pts',(0.0528448073149077,-0.192464754975046,
-0.337039881913867));
#37361=CARTESIAN_POINT('Ctrl Pts',(0.190392067385672,-0.05988419026186,
-0.325920236172266));
#37362=CARTESIAN_POINT('Ctrl Pts',(0.153503101130798,0.127561959495798,
-0.314800590430667));
#37363=CARTESIAN_POINT('Ctrl Pts',(-0.024024611581707,0.198136502463191,
-0.303680944689066));
#37364=CARTESIAN_POINT('Ctrl Pts',(-0.179541099542854,0.0871794077601917,
-0.292561298947467));
#37365=CARTESIAN_POINT('Ctrl Pts',(-0.170562961755526,-0.103651008895067,
-0.281441653205866));
#37366=CARTESIAN_POINT('Ctrl Pts',(-0.00531592149363913,-0.19951690796215,
-0.270322007464267));
#37367=CARTESIAN_POINT('Ctrl Pts',(0.164801538416192,-0.112586448859704,
-0.259202361722666));
#37368=CARTESIAN_POINT('Ctrl Pts',(0.183928682326064,0.0774951314536493,
-0.248082715981066));
#37369=CARTESIAN_POINT('Ctrl Pts',(0.0345413194699957,0.196576074126752,
-0.236963070239466));
#37370=CARTESIAN_POINT('Ctrl Pts',(-0.146492620747893,0.135555034476814,
-0.225843424497866));
#37371=CARTESIAN_POINT('Ctrl Pts',(-0.193310781655808,-0.0496608239121424,
-0.214723778756266));
#37372=CARTESIAN_POINT('Ctrl Pts',(-0.0630186028342171,-0.18937769632408,
-0.203604133014666));
#37373=CARTESIAN_POINT('Ctrl Pts',(0.125010888851029,-0.155587696765142,
-0.192484487273065));
#37374=CARTESIAN_POINT('Ctrl Pts',(0.198506060506429,0.0207509313459927,
-0.181364841531466));
#37375=CARTESIAN_POINT('Ctrl Pts',(0.0901309901048207,0.178077689542741,
-0.170245195789865));
#37376=CARTESIAN_POINT('Ctrl Pts',(-0.100821593921917,0.172250541236717,
-0.159125550048266));
#37377=CARTESIAN_POINT('Ctrl Pts',(-0.199402018138383,0.00860843296761797,
-0.148005904306665));
#37378=CARTESIAN_POINT('Ctrl Pts',(-0.115291226780875,-0.162920856069588,
-0.136886258565066));
#37379=CARTESIAN_POINT('Ctrl Pts',(0.0744485629928304,-0.185182559422327,
-0.125766612823465));
#37380=CARTESIAN_POINT('Ctrl Pts',(0.195979396291931,-0.0377816097851794,
-0.114646967081865));
#37381=CARTESIAN_POINT('Ctrl Pts',(0.137954099945121,0.144235891033227,
-0.103527321340265));
#37382=CARTESIAN_POINT('Ctrl Pts',(-0.046462464332188,0.194102862112147,
-0.092407675598665));
#37383=CARTESIAN_POINT('Ctrl Pts',(-0.188313337494461,0.0661382764452947,
-0.0812880298570651));
#37384=CARTESIAN_POINT('Ctrl Pts',(-0.157626835495907,-0.12243038658036,
-0.0701683841154649));
#37385=CARTESIAN_POINT('Ctrl Pts',(0.0174657603964976,-0.19881271999685,
-0.0590487383738649));
#37386=CARTESIAN_POINT('Ctrl Pts',(0.176576875466308,-0.093074799875673,
-0.0479290926322647));
#37387=CARTESIAN_POINT('Ctrl Pts',(0.173870014291407,0.0979966953574602,
-0.0368094468906647));
#37388=CARTESIAN_POINT('Ctrl Pts',(0.0119390223618658,0.199171650666351,
-0.0256898011490646));
#37389=CARTESIAN_POINT('Ctrl Pts',(-0.161073667403376,0.118083153626222,
-0.0145701554074646));
#37390=CARTESIAN_POINT('Ctrl Pts',(-0.186229738479772,-0.0716257987380052,
-0.00345050966586453));
#37391=CARTESIAN_POINT('Ctrl Pts',(-0.0896636499409105,-0.15368887459728,
0.00396258749520215));
#37392=CARTESIAN_POINT('Ctrl Pts',(-0.0346915509926802,-0.165230719704802,
0.00766913607573549));
#37393=CARTESIAN_POINT('Ctrl Pts',(0.145518343480251,0.10950293141529,-1.00766913607574));
#37394=CARTESIAN_POINT('Ctrl Pts',(0.109086825227246,0.157916742060614,
-1.0039625874952));
#37395=CARTESIAN_POINT('Ctrl Pts',(-0.0152639205362734,0.214685302576403,
-0.996549490334137));
#37396=CARTESIAN_POINT('Ctrl Pts',(-0.18905605945395,0.103294167958045,
-0.985429844592534));
#37397=CARTESIAN_POINT('Ctrl Pts',(-0.189083848276107,-0.102811477342996,
-0.974310198850937));
#37398=CARTESIAN_POINT('Ctrl Pts',(-0.0161510959525931,-0.214680994949199,
-0.963190553109335));
#37399=CARTESIAN_POINT('Ctrl Pts',(0.171723245699015,-0.129882365462275,
-0.952070907367735));
#37400=CARTESIAN_POINT('Ctrl Pts',(0.202190161365477,0.0739250960739926,
-0.940951261626135));
#37401=CARTESIAN_POINT('Ctrl Pts',(0.0474511195296233,0.209996841649205,
-0.929831615884535));
#37402=CARTESIAN_POINT('Ctrl Pts',(-0.150783199571793,0.153673680536314,
-0.918711970142935));
#37403=CARTESIAN_POINT('Ctrl Pts',(-0.210859804054144,-0.0434461456194237,
-0.907592324401335));
#37404=CARTESIAN_POINT('Ctrl Pts',(-0.0777534872514279,-0.200759979592051,
-0.896472678659735));
#37405=CARTESIAN_POINT('Ctrl Pts',(0.126593186365301,-0.174139010658059,
-0.885353032918134));
#37406=CARTESIAN_POINT('Ctrl Pts',(0.214954254923228,0.0120274550054429,
-0.874233387176536));
#37407=CARTESIAN_POINT('Ctrl Pts',(0.106376179610083,0.187174304289003,
-0.863113741434934));
#37408=CARTESIAN_POINT('Ctrl Pts',(-0.0996636373819806,0.190833090456525,
-0.851994095693334));
#37409=CARTESIAN_POINT('Ctrl Pts',(-0.214391916475665,0.0196515529309577,
-0.840874449951735));
#37410=CARTESIAN_POINT('Ctrl Pts',(-0.132695552234643,-0.169534617618786,
-0.829754804210134));
#37411=CARTESIAN_POINT('Ctrl Pts',(0.0705758531641878,-0.203394058784034,
-0.818635158468534));
#37412=CARTESIAN_POINT('Ctrl Pts',(0.209185994090859,-0.0509049114513555,
-0.807515512726934));
#37413=CARTESIAN_POINT('Ctrl Pts',(0.15614102780407,0.148223049567763,-0.796395866985335));
#37414=CARTESIAN_POINT('Ctrl Pts',(-0.0399595488584374,0.211549821411053,
-0.785276221243734));
#37415=CARTESIAN_POINT('Ctrl Pts',(-0.199449388944583,0.0810557415168278,
-0.774156575502134));
#37416=CARTESIAN_POINT('Ctrl Pts',(-0.176204734114151,-0.123701188687723,
-0.763036929760533));
#37417=CARTESIAN_POINT('Ctrl Pts',(0.00847778708947041,-0.215123730513342,
-0.751917284018934));
#37418=CARTESIAN_POINT('Ctrl Pts',(0.185393002960411,-0.109451024202659,
-0.740797638277333));
#37419=CARTESIAN_POINT('Ctrl Pts',(0.192452109810384,0.0965001437138712,
-0.729677992535734));
#37420=CARTESIAN_POINT('Ctrl Pts',(0.0231875899352727,0.214038379645495,
-0.718558346794133));
#37421=CARTESIAN_POINT('Ctrl Pts',(-0.167321279677142,0.135475760375439,
-0.707438701052534));
#37422=CARTESIAN_POINT('Ctrl Pts',(-0.204531259255984,-0.0672090490783415,
-0.696319055310933));
#37423=CARTESIAN_POINT('Ctrl Pts',(-0.0543507580954369,-0.208317275764699,
-0.685199409569334));
#37424=CARTESIAN_POINT('Ctrl Pts',(0.14562562620099,-0.158566293015243,
-0.674079763827733));
#37425=CARTESIAN_POINT('Ctrl Pts',(0.21218056579789,0.0364623063715093,
-0.662960118086133));
#37426=CARTESIAN_POINT('Ctrl Pts',(0.0843367696320044,0.198084329455259,
-0.651840472344534));
#37427=CARTESIAN_POINT('Ctrl Pts',(-0.120775938190972,0.178222515529785,
-0.640720826602933));
#37428=CARTESIAN_POINT('Ctrl Pts',(-0.215234356796293,-0.00492584432610516,
-0.629601180861333));
#37429=CARTESIAN_POINT('Ctrl Pts',(-0.112496172141415,-0.183561171115467,
-0.618481535119733));
#37430=CARTESIAN_POINT('Ctrl Pts',(0.0933104229481655,-0.194018703369007,
-0.607361889378134));
#37431=CARTESIAN_POINT('Ctrl Pts',(0.213626491674075,-0.0267173041829527,
-0.596242243636532));
#37432=CARTESIAN_POINT('Ctrl Pts',(0.138219074840083,0.165062350759088,
-0.585122597894933));
#37433=CARTESIAN_POINT('Ctrl Pts',(-0.0638239426937432,0.205612734592953,
-0.574002952153332));
#37434=CARTESIAN_POINT('Ctrl Pts',(-0.207391794398217,0.0577817956112202,
-0.562883306411733));
#37435=CARTESIAN_POINT('Ctrl Pts',(-0.160948357905082,-0.14298852532782,
-0.551763660670132));
#37436=CARTESIAN_POINT('Ctrl Pts',(0.032955130744744,-0.212753499725302,
-0.540644014928533));
#37437=CARTESIAN_POINT('Ctrl Pts',(0.196665299240809,-0.0875948192662701,
-0.529524369186932));
#37438=CARTESIAN_POINT('Ctrl Pts',(0.180191738863013,0.117817781057408,
-0.518404723445332));
#37439=CARTESIAN_POINT('Ctrl Pts',(-0.00137255966705475,0.215286340411388,
-0.507285077703732));
#37440=CARTESIAN_POINT('Ctrl Pts',(-0.181679326136985,0.115510669386764,
-0.496165431962132));
#37441=CARTESIAN_POINT('Ctrl Pts',(-0.195532434696637,-0.0900952788406405,
-0.485045786220532));
#37442=CARTESIAN_POINT('Ctrl Pts',(-0.0302397390120705,-0.213156399088203,
-0.473926140478932));
#37443=CARTESIAN_POINT('Ctrl Pts',(0.162758448980498,-0.140924730169087,
-0.462806494737332));
#37444=CARTESIAN_POINT('Ctrl Pts',(0.206638188745334,0.060421446853042,
-0.451686848995732));
#37445=CARTESIAN_POINT('Ctrl Pts',(0.0611970899097395,0.206409807117652,
-0.440567203254132));
#37446=CARTESIAN_POINT('Ctrl Pts',(-0.140312465835808,0.163286570846607,
-0.429447557512532));
#37447=CARTESIAN_POINT('Ctrl Pts',(-0.213268466890316,-0.0294389761714076,
-0.418327911770931));
#37448=CARTESIAN_POINT('Ctrl Pts',(-0.0908290028381239,-0.195192685649839,
-0.407208266029332));
#37449=CARTESIAN_POINT('Ctrl Pts',(0.114827523321364,-0.182111867201617,
-0.396088620287731));
#37450=CARTESIAN_POINT('Ctrl Pts',(0.215279667165959,-0.0021810989592354,
-0.384968974546132));
#37451=CARTESIAN_POINT('Ctrl Pts',(0.118493694624951,0.179747980856202,
-0.373849328804531));
#37452=CARTESIAN_POINT('Ctrl Pts',(-0.0868555873967757,0.196992891307782,
-0.362729683062932));
#37453=CARTESIAN_POINT('Ctrl Pts',(-0.212628229964777,0.0337539347294509,
-0.351610037321331));
#37454=CARTESIAN_POINT('Ctrl Pts',(-0.14359198918286,-0.160410202076461,
-0.340490391579732));
#37455=CARTESIAN_POINT('Ctrl Pts',(0.0570024886011833,-0.207607342311188,
-0.329370745838131));
#37456=CARTESIAN_POINT('Ctrl Pts',(0.205371581473172,-0.0645957104631151,
-0.318251100096531));
#37457=CARTESIAN_POINT('Ctrl Pts',(0.165580294773567,0.13759817684211,-0.307131454354931));
#37458=CARTESIAN_POINT('Ctrl Pts',(-0.0259148006666635,0.213725326990651,
-0.296011808613331));
#37459=CARTESIAN_POINT('Ctrl Pts',(-0.193666889901754,0.0940384391506045,
-0.284892162871731));
#37460=CARTESIAN_POINT('Ctrl Pts',(-0.183982377404012,-0.11180597968375,
-0.27377251713013));
#37461=CARTESIAN_POINT('Ctrl Pts',(-0.00573416329328779,-0.215214338924227,
-0.262652871388531));
#37462=CARTESIAN_POINT('Ctrl Pts',(0.177767661428798,-0.12144443501382,
-0.25153322564693));
#37463=CARTESIAN_POINT('Ctrl Pts',(0.198399675397523,0.0835922311346511,
-0.240413579905331));
#37464=CARTESIAN_POINT('Ctrl Pts',(0.0372589336474485,0.212042128527444,
-0.22929393416373));
#37465=CARTESIAN_POINT('Ctrl Pts',(-0.158018249448392,0.146220124553619,
-0.218174288422131));
#37466=CARTESIAN_POINT('Ctrl Pts',(-0.20851993199931,-0.0535679983107572,
-0.20705464268053));
#37467=CARTESIAN_POINT('Ctrl Pts',(-0.0679767298291708,-0.204277402540297,
-0.195934996938931));
#37468=CARTESIAN_POINT('Ctrl Pts',(0.134846395111074,-0.167828900548145,
-0.18481535119733));
#37469=CARTESIAN_POINT('Ctrl Pts',(0.214123960824655,0.0223835564479417,
-0.17369570545573));
#37470=CARTESIAN_POINT('Ctrl Pts',(0.097222243719189,0.19208834290558,-0.16257605971413));
#37471=CARTESIAN_POINT('Ctrl Pts',(-0.10875395427293,0.185802730907562,
-0.15145641397253));
#37472=CARTESIAN_POINT('Ctrl Pts',(-0.215090409891226,0.0092857203393065,
-0.14033676823093));
#37473=CARTESIAN_POINT('Ctrl Pts',(-0.124362017278838,-0.175739012267757,
-0.12921712248933));
#37474=CARTESIAN_POINT('Ctrl Pts',(0.0803059672085533,-0.199752204028408,
-0.11809747674773));
#37475=CARTESIAN_POINT('Ctrl Pts',(0.211398505753398,-0.0407541609203029,
-0.10697783100613));
#37476=CARTESIAN_POINT('Ctrl Pts',(0.148807941767063,0.15558396656664,-0.0958581852645297));
#37477=CARTESIAN_POINT('Ctrl Pts',(-0.0501180007658248,0.209374331125314,
-0.0847385395229296));
#37478=CARTESIAN_POINT('Ctrl Pts',(-0.203129302941952,0.0713418506137954,
-0.0736188937813295));
#37479=CARTESIAN_POINT('Ctrl Pts',(-0.170028472997412,-0.132062866156327,
-0.0624992480397294));
#37480=CARTESIAN_POINT('Ctrl Pts',(0.018839917458294,-0.214454747424046,
-0.0513796022981294));
#37481=CARTESIAN_POINT('Ctrl Pts',(0.190469448985226,-0.100397664189683,
-0.0402599565565293));
#37482=CARTESIAN_POINT('Ctrl Pts',(0.187549619561917,0.105706800609176,
-0.0291403108149292));
#37483=CARTESIAN_POINT('Ctrl Pts',(0.0128783511696067,0.214841917752341,
-0.0180206650733292));
#37484=CARTESIAN_POINT('Ctrl Pts',(-0.17374649197598,0.12737360510106,-0.00690101933172906));
#37485=CARTESIAN_POINT('Ctrl Pts',(-0.20088177219827,-0.07726111577593,
0.00421862640987097));
#37486=CARTESIAN_POINT('Ctrl Pts',(-0.0967181345413958,-0.165780684375565,
0.0116317235709377));
#37487=CARTESIAN_POINT('Ctrl Pts',(-0.0374209849651557,-0.178230609497963,
0.015338272151471));
#37488=CARTESIAN_POINT('Ctrl Pts',(0.156132246633336,0.117489921104864,
-1.));
#37489=CARTESIAN_POINT('Ctrl Pts',(0.117043464717144,0.169434966955123,
-0.996293451419467));
#37490=CARTESIAN_POINT('Ctrl Pts',(-0.0163772494158741,0.2303441463719,
-0.9888803542584));
#37491=CARTESIAN_POINT('Ctrl Pts',(-0.202845542329835,0.110828299180025,
-0.9777607085168));
#37492=CARTESIAN_POINT('Ctrl Pts',(-0.202875358029568,-0.11031040179091,
-0.9666410627752));
#37493=CARTESIAN_POINT('Ctrl Pts',(-0.0173291341583431,-0.23033952455243,
-0.9555214170336));
#37494=CARTESIAN_POINT('Ctrl Pts',(0.184248497535942,-0.139355802386723,
-0.944401771292));
#37495=CARTESIAN_POINT('Ctrl Pts',(0.216937627148243,0.0793170885303813,
-0.933282125550399));
#37496=CARTESIAN_POINT('Ctrl Pts',(0.0509121373995896,0.225313715703786,
-0.922162479808799));
#37497=CARTESIAN_POINT('Ctrl Pts',(-0.161781113917791,0.164882422495448,
-0.9110428340672));
#37498=CARTESIAN_POINT('Ctrl Pts',(-0.226239621371903,-0.0466150463294693,
-0.899923188325598));
#37499=CARTESIAN_POINT('Ctrl Pts',(-0.0834247171717535,-0.215403129929277,
-0.888803542584));
#37500=CARTESIAN_POINT('Ctrl Pts',(0.135826715196008,-0.186840464990857,
-0.877683896842398));
#37501=CARTESIAN_POINT('Ctrl Pts',(0.230632715724346,0.0129047206446236,
-0.866564251100799));
#37502=CARTESIAN_POINT('Ctrl Pts',(0.114135108423961,0.200826534591769,
-0.855444605359199));
#37503=CARTESIAN_POINT('Ctrl Pts',(-0.106932962813794,0.204752187472527,
-0.8443249596176));
#37504=CARTESIAN_POINT('Ctrl Pts',(-0.230029361101922,0.0210849095417369,
-0.833205313875998));
#37505=CARTESIAN_POINT('Ctrl Pts',(-0.142374179042644,-0.181900234004086,
-0.8220856681344));
#37506=CARTESIAN_POINT('Ctrl Pts',(0.0757235565568705,-0.218229335149998,
-0.810966022392799));
#37507=CARTESIAN_POINT('Ctrl Pts',(0.224443726065821,-0.0546178440428023,
-0.799846376651198));
#37508=CARTESIAN_POINT('Ctrl Pts',(0.167529734600066,0.159034230175935,
-0.788726730909599));
#37509=CARTESIAN_POINT('Ctrl Pts',(-0.0428741421082007,0.22697996762361,
-0.777607085167998));
#37510=CARTESIAN_POINT('Ctrl Pts',(-0.213996946644668,0.0869678332152738,
-0.766487439426399));
#37511=CARTESIAN_POINT('Ctrl Pts',(-0.189056859408284,-0.132723779278379,
-0.755367793684799));
#37512=CARTESIAN_POINT('Ctrl Pts',(0.00909614494709787,-0.230814552625462,
-0.744248147943198));
#37513=CARTESIAN_POINT('Ctrl Pts',(0.198915307651492,-0.117434227853206,
-0.733128502201599));
#37514=CARTESIAN_POINT('Ctrl Pts',(0.20648929581925,0.103538728370222,-0.722008856459998));
#37515=CARTESIAN_POINT('Ctrl Pts',(0.0248788601080945,0.22965003779297,
-0.710889210718398));
#37516=CARTESIAN_POINT('Ctrl Pts',(-0.179525458308301,0.145357171652024,
-0.699769564976799));
#37517=CARTESIAN_POINT('Ctrl Pts',(-0.219449481423736,-0.0721111825198558,
-0.688649919235197));
#37518=CARTESIAN_POINT('Ctrl Pts',(-0.0583150258909959,-0.223511644647691,
-0.677530273493599));
#37519=CARTESIAN_POINT('Ctrl Pts',(0.156247354404722,-0.170131895242127,
-0.666410627751997));
#37520=CARTESIAN_POINT('Ctrl Pts',(0.227656717618236,0.0391218156767241,
-0.655290982010398));
#37521=CARTESIAN_POINT('Ctrl Pts',(0.0904881749030501,0.212532321637545,
-0.644171336268797));
#37522=CARTESIAN_POINT('Ctrl Pts',(-0.129585165127752,0.191221814960301,
-0.633051690527198));
#37523=CARTESIAN_POINT('Ctrl Pts',(-0.230933247833782,-0.00528512847801286,
-0.621932044785597));
#37524=CARTESIAN_POINT('Ctrl Pts',(-0.120701484596501,-0.196949864570122,
-0.610812399043998));
#37525=CARTESIAN_POINT('Ctrl Pts',(0.10011635386147,-0.208170154507023,
-0.599692753302397));
#37526=CARTESIAN_POINT('Ctrl Pts',(0.229208107292656,-0.0286660267448476,
-0.588573107560798));
#37527=CARTESIAN_POINT('Ctrl Pts',(0.148300579612441,0.177101766294457,
-0.577453461819196));
#37528=CARTESIAN_POINT('Ctrl Pts',(-0.0684791712401787,0.220609838049582,
-0.566333816077598));
#37529=CARTESIAN_POINT('Ctrl Pts',(-0.222518659972974,0.0619963184539177,
-0.555214170335996));
#37530=CARTESIAN_POINT('Ctrl Pts',(-0.17268770459222,-0.153417907105642,
-0.544094524594398));
#37531=CARTESIAN_POINT('Ctrl Pts',(0.0353588315961715,-0.228271440539896,
-0.532974878852797));
#37532=CARTESIAN_POINT('Ctrl Pts',(0.21100978935657,-0.0939838620918607,
-0.521855233111197));
#37533=CARTESIAN_POINT('Ctrl Pts',(0.193334670671728,0.126411244176538,
-0.510735587369597));
#37534=CARTESIAN_POINT('Ctrl Pts',(-0.00147267223725966,0.230989023060594,
-0.499615941627997));
#37535=CARTESIAN_POINT('Ctrl Pts',(-0.19493076046765,0.123935855027952,
-0.488496295886396));
#37536=CARTESIAN_POINT('Ctrl Pts',(-0.20979429526708,-0.0966667016681302,
-0.477376650144797));
#37537=CARTESIAN_POINT('Ctrl Pts',(-0.0324453830124945,-0.228703726815237,
-0.466257004403196));
#37538=CARTESIAN_POINT('Ctrl Pts',(0.174629821162932,-0.151203581632872,
-0.455137358661597));
#37539=CARTESIAN_POINT('Ctrl Pts',(0.221710087384488,0.0648285021419467,
-0.444017712919996));
#37540=CARTESIAN_POINT('Ctrl Pts',(0.0656607195114666,0.221465047922334,
-0.432898067178396));
#37541=CARTESIAN_POINT('Ctrl Pts',(-0.150546659600897,0.175196463494612,
-0.421778421436796));
#37542=CARTESIAN_POINT('Ctrl Pts',(-0.228823968685098,-0.0315862136573233,
-0.410658775695196));
#37543=CARTESIAN_POINT('Ctrl Pts',(-0.0974539424612588,-0.209429765403011,
-0.399539129953596));
#37544=CARTESIAN_POINT('Ctrl Pts',(0.123202881250083,-0.195394850468726,
-0.388419484211996));
#37545=CARTESIAN_POINT('Ctrl Pts',(0.230981863078037,-0.00234018524737671,
-0.377299838470396));
#37546=CARTESIAN_POINT('Ctrl Pts',(0.127136457928336,0.192858545580498,
-0.366180192728797));
#37547=CARTESIAN_POINT('Ctrl Pts',(-0.0931907116902888,0.211361275527816,
-0.355060546987195));
#37548=CARTESIAN_POINT('Ctrl Pts',(-0.228137033779358,0.0362158992191905,
-0.343940901245597));
#37549=CARTESIAN_POINT('Ctrl Pts',(-0.154065386764881,-0.172110296434925,
-0.332821255503995));
#37550=CARTESIAN_POINT('Ctrl Pts',(0.0611601698874586,-0.22274992964733,
-0.321701609762396));
#37551=CARTESIAN_POINT('Ctrl Pts',(0.220351095560672,-0.0693072306643703,
-0.310581964020795));
#37552=CARTESIAN_POINT('Ctrl Pts',(0.177657488416336,0.147634394188423,
-0.299462318279196));
#37553=CARTESIAN_POINT('Ctrl Pts',(-0.0278049897516198,0.22931415151811,
-0.288342672537595));
#37554=CARTESIAN_POINT('Ctrl Pts',(-0.207792680260653,0.100897470541018,
-0.277223026795995));
#37555=CARTESIAN_POINT('Ctrl Pts',(-0.197401793052498,-0.119960950472433,
-0.266103381054396));
#37556=CARTESIAN_POINT('Ctrl Pts',(-0.00615240509293671,-0.230911769886303,
-0.254983735312795));
#37557=CARTESIAN_POINT('Ctrl Pts',(0.190733784441404,-0.130302421167936,
-0.243864089571195));
#37558=CARTESIAN_POINT('Ctrl Pts',(0.212870668468982,0.0896893308156527,
-0.232744443829595));
#37559=CARTESIAN_POINT('Ctrl Pts',(0.0399765478249015,0.227508182928137,
-0.221624798087995));
#37560=CARTESIAN_POINT('Ctrl Pts',(-0.169543878148892,0.156885214630423,
-0.210505152346395));
#37561=CARTESIAN_POINT('Ctrl Pts',(-0.223729082342813,-0.0574751727093715,
-0.199385506604795));
#37562=CARTESIAN_POINT('Ctrl Pts',(-0.0729348568241247,-0.219177108756516,
-0.188265860863195));
#37563=CARTESIAN_POINT('Ctrl Pts',(0.144681901371119,-0.180070104331149,
-0.177146215121594));
#37564=CARTESIAN_POINT('Ctrl Pts',(0.22974186114288,0.0240161815498906,
-0.166026569379995));
#37565=CARTESIAN_POINT('Ctrl Pts',(0.104313497333558,0.206098996268419,
-0.154906923638395));
#37566=CARTESIAN_POINT('Ctrl Pts',(-0.116686314623943,0.199354920578408,
-0.143787277896795));
#37567=CARTESIAN_POINT('Ctrl Pts',(-0.230778801644068,0.00996300771099484,
-0.132667632155194));
#37568=CARTESIAN_POINT('Ctrl Pts',(-0.133432807776802,-0.188557168465927,
-0.121547986413595));
#37569=CARTESIAN_POINT('Ctrl Pts',(0.0861633714242763,-0.214321848634489,
-0.110428340671994));
#37570=CARTESIAN_POINT('Ctrl Pts',(0.226817615214866,-0.0437267120554264,
-0.0993086949303942));
#37571=CARTESIAN_POINT('Ctrl Pts',(0.159661783589004,0.166932042100053,
-0.0881890491887944));
#37572=CARTESIAN_POINT('Ctrl Pts',(-0.0537735371994615,0.224645800138481,
-0.0770694034471939));
#37573=CARTESIAN_POINT('Ctrl Pts',(-0.217945268389443,0.0765454247822962,
-0.0659497577055941));
#37574=CARTESIAN_POINT('Ctrl Pts',(-0.182430110498917,-0.141695345732293,
-0.0548301119639939));
#37575=CARTESIAN_POINT('Ctrl Pts',(0.0202140745200903,-0.230096774851241,
-0.0437104662223939));
#37576=CARTESIAN_POINT('Ctrl Pts',(0.204362022504145,-0.107720528503693,
-0.0325908204807937));
#37577=CARTESIAN_POINT('Ctrl Pts',(0.201229224832426,0.113416905860893,
-0.0214711747391938));
#37578=CARTESIAN_POINT('Ctrl Pts',(0.0138176799773481,0.230512184838331,
-0.0103515289975936));
#37579=CARTESIAN_POINT('Ctrl Pts',(-0.186419316548585,0.136664056575899,
0.000768116744006414));
#37580=CARTESIAN_POINT('Ctrl Pts',(-0.215533805916768,-0.082896432813855,
0.0118877624856065));
#37581=CARTESIAN_POINT('Ctrl Pts',(-0.103772619141881,-0.17787249415385,
0.0193008596466731));
#37582=CARTESIAN_POINT('Ctrl Pts',(-0.0401504189376312,-0.191230499291124,
0.0230074082272065));
#37583=CARTESIAN_POINT('',(-0.149577339797456,0.126231096176531,2.3740120150659E-16));
#37584=CARTESIAN_POINT('Ctrl Pts',(-0.149579224365402,0.126232117338717,
3.12250225675825E-17));
#37585=CARTESIAN_POINT('Ctrl Pts',(-0.15213626770352,0.122550735753821,
1.75395509689456E-17));
#37586=CARTESIAN_POINT('Ctrl Pts',(-0.154553778983314,0.118780419069818,
-2.56435089757285E-17));
#37587=CARTESIAN_POINT('Ctrl Pts',(-0.156823814682293,0.114924149748616,
-7.28583859910259E-17));
#37588=CARTESIAN_POINT('Ctrl Pts',(-0.161285099186592,0.107345451944513,
-1.65588310206067E-16));
#37589=CARTESIAN_POINT('Ctrl Pts',(-0.165177482683705,0.0994348489301857,
-4.45014344919782E-16));
#37590=CARTESIAN_POINT('Ctrl Pts',(-0.168497913306379,0.0912613466614302,
-6.1409211049579E-16));
#37591=CARTESIAN_POINT('Ctrl Pts',(-0.170168203952632,0.0871497942942736,
-6.9914403370195E-16));
#37592=CARTESIAN_POINT('Ctrl Pts',(-0.171694353287266,0.0829692560081717,
-3.2424756013121E-16));
#37593=CARTESIAN_POINT('Ctrl Pts',(-0.173072321343778,0.0787365486429996,
-3.08780778723872E-16));
#37594=CARTESIAN_POINT('Ctrl Pts',(-0.17688112264392,0.0670370457122868,
-2.66029499508873E-16));
#37595=CARTESIAN_POINT('Ctrl Pts',(-0.179552067097139,0.0549719351495626,
-1.72155562539013E-16));
#37596=CARTESIAN_POINT('Ctrl Pts',(-0.181069928572971,0.0427320571800164,
1.45716771982052E-16));
#37597=CARTESIAN_POINT('Ctrl Pts',(-0.181571983366965,0.0386835392418783,
2.50857677107766E-16));
#37598=CARTESIAN_POINT('Ctrl Pts',(-0.181947631644738,0.0346138283481453,
-4.72643688963084E-17));
#37599=CARTESIAN_POINT('Ctrl Pts',(-0.18219485039693,0.0305368171567139,
-6.93889390390723E-17));
#37600=CARTESIAN_POINT('Ctrl Pts',(-0.182940753710731,0.0182357431842819,
-1.36142735179339E-16));
#37601=CARTESIAN_POINT('Ctrl Pts',(-0.182518848032763,0.00592920171664246,
-2.46842689824824E-16));
#37602=CARTESIAN_POINT('Ctrl Pts',(-0.180911458839137,-0.00619024109343332,
-3.34801630863524E-16));
#37603=CARTESIAN_POINT('Ctrl Pts',(-0.179850463364892,-0.0141899676206825,
-3.92861022286291E-16));
#37604=CARTESIAN_POINT('Ctrl Pts',(-0.178271908795443,-0.0221081540245901,
-2.21255589905061E-16));
#37605=CARTESIAN_POINT('Ctrl Pts',(-0.176159106007433,-0.0298838204643374,
-3.40005801291454E-16));
#37606=CARTESIAN_POINT('Ctrl Pts',(-0.174809572472798,-0.0348504565716565,
-4.15856417080292E-16));
#37607=CARTESIAN_POINT('Ctrl Pts',(-0.173239451433683,-0.0397640700380695,
-3.63363244663589E-16));
#37608=CARTESIAN_POINT('Ctrl Pts',(-0.171455092377085,-0.0445771192033741,
-3.71230823859037E-16));
#37609=CARTESIAN_POINT('Ctrl Pts',(-0.169157099318569,-0.0507756214225697,
-3.81363113272206E-16));
#37610=CARTESIAN_POINT('Ctrl Pts',(-0.1665024797364,-0.0568161660521192,
-2.09853073085683E-16));
#37611=CARTESIAN_POINT('Ctrl Pts',(-0.16348481359929,-0.0626658509200692,
-2.98372437868011E-16));
#37612=CARTESIAN_POINT('Ctrl Pts',(-0.158069190177679,-0.0731639275596034,
-4.56902188558693E-16));
#37613=CARTESIAN_POINT('Ctrl Pts',(-0.15148551162908,-0.0830500140735381,
-1.69238594609806E-16));
#37614=CARTESIAN_POINT('Ctrl Pts',(-0.143886948956133,-0.0921970824958435,
-6.24500451351651E-17));
#37615=CARTESIAN_POINT('Ctrl Pts',(-0.141498396059732,-0.0950723969091165,
-2.88818414986653E-17));
#37616=CARTESIAN_POINT('Ctrl Pts',(-0.139008411786517,-0.0978749248249702,
-3.46133223658663E-16));
#37617=CARTESIAN_POINT('Ctrl Pts',(-0.136433692072541,-0.100588045776136,
-3.48679418671338E-16));
#37618=CARTESIAN_POINT('Ctrl Pts',(-0.129595227249087,-0.107794104783498,
-3.55442121785516E-16));
#37619=CARTESIAN_POINT('Ctrl Pts',(-0.122142516767232,-0.114393608368861,
-2.3081146500224E-16));
#37620=CARTESIAN_POINT('Ctrl Pts',(-0.114172290333582,-0.1203153298124,
-2.60208521396521E-16));
#37621=CARTESIAN_POINT('Ctrl Pts',(-0.109745931829009,-0.123604027102437,
-2.76534520621699E-16));
#37622=CARTESIAN_POINT('Ctrl Pts',(-0.105159682538236,-0.126683244398258,
1.53094208316784E-16));
#37623=CARTESIAN_POINT('Ctrl Pts',(-0.100428978517873,-0.129537077171602,
2.34187669256869E-16));
#37624=CARTESIAN_POINT('Ctrl Pts',(-0.0974655015542694,-0.131324816934094,
2.84987423872767E-16));
#37625=CARTESIAN_POINT('Ctrl Pts',(-0.0944453272369587,-0.133024055864704,
-1.57159659481818E-16));
#37626=CARTESIAN_POINT('Ctrl Pts',(-0.091372239374377,-0.134630282149142,
-1.76941794549634E-16));
#37627=CARTESIAN_POINT('Ctrl Pts',(-0.0882085618680696,-0.136283857378145,
-1.97307074860303E-16));
#37628=CARTESIAN_POINT('Ctrl Pts',(-0.084995963230153,-0.137835002018624,
-1.14607397771812E-16));
#37629=CARTESIAN_POINT('Ctrl Pts',(-0.0817435159838432,-0.139278121880328,
-1.25333771139324E-16));
#37630=CARTESIAN_POINT('Ctrl Pts',(-0.0719268932182113,-0.143633784621363,
-1.57708396465424E-16));
#37631=CARTESIAN_POINT('Ctrl Pts',(-0.0617342162816699,-0.147015917264351,
-2.37152691385054E-16));
#37632=CARTESIAN_POINT('Ctrl Pts',(-0.0512859179194202,-0.149305219054896,
-1.346579098227E-16));
#37633=CARTESIAN_POINT('Ctrl Pts',(-0.0449298836761154,-0.150697874592619,
-7.23070543260647E-17));
#37634=CARTESIAN_POINT('Ctrl Pts',(-0.0384791302638158,-0.151685198677283,
-1.58142429239726E-16));
#37635=CARTESIAN_POINT('Ctrl Pts',(-0.0319621170202069,-0.15223082991164,
-1.59594559789866E-16));
#37636=CARTESIAN_POINT('Ctrl Pts',(-0.195209575558751,0.00014773333329694,
-0.0621869692124235));
#37637=CARTESIAN_POINT('Ctrl Pts',(-0.194905259338105,-0.0429573617160955,
-0.059734683462947));
#37638=CARTESIAN_POINT('Ctrl Pts',(-0.180836665151344,-0.0862425843964161,
-0.0572823977134706));
#37639=CARTESIAN_POINT('Ctrl Pts',(-0.154575272644172,-0.120055455499684,
-0.0548301119639941));
#37640=CARTESIAN_POINT('Ctrl Pts',(-0.114882048825917,-0.171162488771942,
-0.0511235633834607));
#37641=CARTESIAN_POINT('Ctrl Pts',(-0.0473339871529112,-0.200629631811592,
-0.0474170148029272));
#37642=CARTESIAN_POINT('Ctrl Pts',(0.0171313683475999,-0.194967162273492,
-0.0437104662223938));
#37643=CARTESIAN_POINT('Ctrl Pts',(0.0815967238481101,-0.189304692735391,
-0.0400039176418604));
#37644=CARTESIAN_POINT('Ctrl Pts',(0.142979373176127,-0.148512610619542,
-0.0362973690613271));
#37645=CARTESIAN_POINT('Ctrl Pts',(0.173148564894849,-0.0912603305008528,
-0.0325908204807937));
#37646=CARTESIAN_POINT('Ctrl Pts',(0.203317756613572,-0.0340080503821637,
-0.0288842719002604));
#37647=CARTESIAN_POINT('Ctrl Pts',(0.202273490722998,0.0397044277393669,
-0.025177723319727));
#37648=CARTESIAN_POINT('Ctrl Pts',(0.170516100301865,0.096076546629704,
-0.0214711747391936));
#37649=CARTESIAN_POINT('Ctrl Pts',(0.138758709880731,0.15244866552004,-0.0177646261586603));
#37650=CARTESIAN_POINT('Ctrl Pts',(0.0762881949290407,0.191480425179185,
-0.014058077578127));
#37651=CARTESIAN_POINT('Ctrl Pts',(0.0116801046988732,0.195354950298353,
-0.0103515289975937));
#37652=CARTESIAN_POINT('Ctrl Pts',(-0.0484650235757366,0.198961833112337,
-0.00690101933172905));
#37653=CARTESIAN_POINT('Ctrl Pts',(-0.110462610495604,0.172100865870811,
-0.00345050966586447));
#37654=CARTESIAN_POINT('Ctrl Pts',(-0.149579224365404,0.126232117338714,
1.70002900645727E-16));
#37655=CARTESIAN_POINT('',(-0.141301845044904,0.0650353064643039,-1.));
#37656=CARTESIAN_POINT('Ctrl Pts',(-0.141514759450945,0.0651925368729976,
-1.));
#37657=CARTESIAN_POINT('Ctrl Pts',(-0.140439543113019,0.0686377703387253,
-1.));
#37658=CARTESIAN_POINT('Ctrl Pts',(-0.139238142539461,0.0720367067892421,
-1.));
#37659=CARTESIAN_POINT('Ctrl Pts',(-0.137910622472938,0.0753822101626856,
-1.));
#37660=CARTESIAN_POINT('Ctrl Pts',(-0.134668353041792,0.0835531023345245,
-1.));
#37661=CARTESIAN_POINT('Ctrl Pts',(-0.130675558679426,0.0914056054140095,
-1.));
#37662=CARTESIAN_POINT('Ctrl Pts',(-0.126026137664389,0.0988943536247196,
-1.));
#37663=CARTESIAN_POINT('Ctrl Pts',(-0.123780053918212,0.102512084860693,
-1.));
#37664=CARTESIAN_POINT('Ctrl Pts',(-0.121379830696976,0.106044927785419,
-1.));
#37665=CARTESIAN_POINT('Ctrl Pts',(-0.118844566172191,0.109475158254566,
-1.));
#37666=CARTESIAN_POINT('Ctrl Pts',(-0.1142132117073,0.115741412936701,-1.));
#37667=CARTESIAN_POINT('Ctrl Pts',(-0.109125681139024,0.121676187684083,
-1.));
#37668=CARTESIAN_POINT('Ctrl Pts',(-0.103641429786816,0.127248528569788,
-1.));
#37669=CARTESIAN_POINT('Ctrl Pts',(-0.100783730165235,0.130152129338194,
-1.));
#37670=CARTESIAN_POINT('Ctrl Pts',(-0.0978169100852653,0.132958315023231,
-1.));
#37671=CARTESIAN_POINT('Ctrl Pts',(-0.0947519441241897,0.135658875758607,
-1.));
#37672=CARTESIAN_POINT('Ctrl Pts',(-0.0860010566744776,0.14336933758641,
-1.));
#37673=CARTESIAN_POINT('Ctrl Pts',(-0.0765074634433449,0.150174174108871,
-1.));
#37674=CARTESIAN_POINT('Ctrl Pts',(-0.0664560352410665,0.155977668638949,
-1.));
#37675=CARTESIAN_POINT('Ctrl Pts',(-0.0587959349774297,0.16040045802621,
-1.));
#37676=CARTESIAN_POINT('Ctrl Pts',(-0.0508104927247559,0.164241610466299,
-1.));
#37677=CARTESIAN_POINT('Ctrl Pts',(-0.0425661446334144,0.167446298872687,
-1.));
#37678=CARTESIAN_POINT('Ctrl Pts',(-0.0392699210733563,0.168727585071517,
-1.));
#37679=CARTESIAN_POINT('Ctrl Pts',(-0.0359322471339816,0.169906628237342,
-1.));
#37680=CARTESIAN_POINT('Ctrl Pts',(-0.0325709935602962,0.170975746975499,
-1.));
#37681=CARTESIAN_POINT('Ctrl Pts',(-0.0260409344851832,0.173052772217845,
-1.));
#37682=CARTESIAN_POINT('Ctrl Pts',(-0.0194097376667411,0.174720258844212,
-1.));
#37683=CARTESIAN_POINT('Ctrl Pts',(-0.0127103276648721,0.175957707572939,
-1.));
#37684=CARTESIAN_POINT('Ctrl Pts',(-0.00513764342403194,0.17735645887854,
-1.));
#37685=CARTESIAN_POINT('Ctrl Pts',(0.00252225608355841,0.178206122099873,
-1.));
#37686=CARTESIAN_POINT('Ctrl Pts',(0.0102240731002703,0.178534251350247,
-1.));
#37687=CARTESIAN_POINT('Ctrl Pts',(0.0149026548551076,0.178733578277996,
-1.));
#37688=CARTESIAN_POINT('Ctrl Pts',(0.0195967888085301,0.178740260799471,
-1.));
#37689=CARTESIAN_POINT('Ctrl Pts',(0.0242967627079693,0.178558747054534,
-1.));
#37690=CARTESIAN_POINT('Ctrl Pts',(0.0278750965504952,0.178420551228283,
-1.));
#37691=CARTESIAN_POINT('Ctrl Pts',(0.0314562829551843,0.178172985748135,
-1.));
#37692=CARTESIAN_POINT('Ctrl Pts',(0.0350223326126129,0.177819803126781,
-1.));
#37693=CARTESIAN_POINT('Ctrl Pts',(0.0464531859559181,0.176687688003343,
-1.));
#37694=CARTESIAN_POINT('Ctrl Pts',(0.057763458181646,0.174472683704982,
-1.));
#37695=CARTESIAN_POINT('Ctrl Pts',(0.0688115888091587,0.171259810959209,
-1.));
#37696=CARTESIAN_POINT('Ctrl Pts',(0.0755835048896587,0.169290490958818,
-1.));
#37697=CARTESIAN_POINT('Ctrl Pts',(0.0822572209906249,0.16694544858736,
-1.));
#37698=CARTESIAN_POINT('Ctrl Pts',(0.0888005398454858,0.164236932162052,
-1.));
#37699=CARTESIAN_POINT('Ctrl Pts',(0.0937380717004385,0.162193109076817,
-1.));
#37700=CARTESIAN_POINT('Ctrl Pts',(0.0986065782001952,0.159939028720903,
-1.));
#37701=CARTESIAN_POINT('Ctrl Pts',(0.103361681203228,0.157494885851826,
-1.));
#37702=CARTESIAN_POINT('Ctrl Pts',(0.114767902239668,0.151632040443103,
-1.));
#37703=CARTESIAN_POINT('Ctrl Pts',(0.125550646082581,0.144670357618447,
-1.));
#37704=CARTESIAN_POINT('Ctrl Pts',(0.135527553857112,0.13669485551301,-1.));
#37705=CARTESIAN_POINT('Ctrl Pts',(0.142856934691975,0.130835776367343,
-1.));
#37706=CARTESIAN_POINT('Ctrl Pts',(0.149751664752612,0.124428399142311,
-1.));
#37707=CARTESIAN_POINT('Ctrl Pts',(0.156132246633335,0.117489921104865,
-1.));
#37708=CARTESIAN_POINT('Ctrl Pts',(-0.141514759450946,0.0651925368729961,
-1.));
#37709=CARTESIAN_POINT('Ctrl Pts',(-0.150731766956786,0.0449100614655458,
-0.99839812581321));
#37710=CARTESIAN_POINT('Ctrl Pts',(-0.15533019555488,0.0224563452055557,
-0.996796251626419));
#37711=CARTESIAN_POINT('Ctrl Pts',(-0.155319281545194,2.55672115836644E-6,
-0.995194377439629));
#37712=CARTESIAN_POINT('Origin',(-2.59090492670967E-17,0.,-1.));
#37713=CARTESIAN_POINT('Ctrl Pts',(0.188715001522267,-0.051914696198531,
-1.));
#37714=CARTESIAN_POINT('Ctrl Pts',(0.187126268659119,-0.0561059924632036,
-1.));
#37715=CARTESIAN_POINT('Ctrl Pts',(0.185385258844343,-0.0602325559568805,
-1.));
#37716=CARTESIAN_POINT('Ctrl Pts',(0.183489936934311,-0.0642861493789803,
-1.));
#37717=CARTESIAN_POINT('Ctrl Pts',(0.179765074014344,-0.0722526482363455,
-1.));
#37718=CARTESIAN_POINT('Ctrl Pts',(0.17544466132878,-0.0799378474501277,
-1.));
#37719=CARTESIAN_POINT('Ctrl Pts',(0.170583870709489,-0.0873001880106591,
-1.));
#37720=CARTESIAN_POINT('Ctrl Pts',(0.16813872456559,-0.0910037004722348,
-1.));
#37721=CARTESIAN_POINT('Ctrl Pts',(0.165555142410874,-0.094627392494239,
-1.));
#37722=CARTESIAN_POINT('Ctrl Pts',(0.162844704799912,-0.098158418110447,
-1.));
#37723=CARTESIAN_POINT('Ctrl Pts',(0.155352865708622,-0.107918419830045,
-1.));
#37724=CARTESIAN_POINT('Ctrl Pts',(0.146915777629002,-0.116947057395722,
-1.));
#37725=CARTESIAN_POINT('Ctrl Pts',(0.137682182322815,-0.125123801279632,
-1.));
#37726=CARTESIAN_POINT('Ctrl Pts',(0.134628037165296,-0.127828377548053,
-1.));
#37727=CARTESIAN_POINT('Ctrl Pts',(0.131484897843174,-0.130440716087263,
-1.));
#37728=CARTESIAN_POINT('Ctrl Pts',(0.12826307503258,-0.132951288440458,
-1.));
#37729=CARTESIAN_POINT('Ctrl Pts',(0.118542257931425,-0.140526135382502,
-1.));
#37730=CARTESIAN_POINT('Ctrl Pts',(0.10815619820295,-0.147141159084441,
-1.));
#37731=CARTESIAN_POINT('Ctrl Pts',(0.0972536752672356,-0.15267283480508,
-1.));
#37732=CARTESIAN_POINT('Ctrl Pts',(0.090057189388818,-0.156324157204702,
-1.));
#37733=CARTESIAN_POINT('Ctrl Pts',(0.0826351063399878,-0.159502589968769,
-1.));
#37734=CARTESIAN_POINT('Ctrl Pts',(0.0750282645074606,-0.162159870196947,
-1.));
#37735=CARTESIAN_POINT('Ctrl Pts',(0.0701695094492505,-0.163857167713314,
-1.));
#37736=CARTESIAN_POINT('Ctrl Pts',(0.0652296690239961,-0.165342583374345,
-1.));
#37737=CARTESIAN_POINT('Ctrl Pts',(0.0602515354147416,-0.166594454550118,
-1.));
#37738=CARTESIAN_POINT('Ctrl Pts',(0.0538403798350176,-0.168206693494195,
-1.));
#37739=CARTESIAN_POINT('Ctrl Pts',(0.0473576918062638,-0.169435505552497,
-1.));
#37740=CARTESIAN_POINT('Ctrl Pts',(0.0408269682982621,-0.170256981483823,
-1.));
#37741=CARTESIAN_POINT('Ctrl Pts',(0.0291066787191395,-0.171731234035722,
-1.));
#37742=CARTESIAN_POINT('Ctrl Pts',(0.017230129317074,-0.171896111652057,
-1.));
#37743=CARTESIAN_POINT('Ctrl Pts',(0.00538872457353722,-0.170806039426225,
-1.));
#37744=CARTESIAN_POINT('Ctrl Pts',(0.00166646623728207,-0.170463383253449,
-1.));
#37745=CARTESIAN_POINT('Ctrl Pts',(-0.0020531649922566,-0.169995910229923,
-1.));
#37746=CARTESIAN_POINT('Ctrl Pts',(-0.00574701830086723,-0.169407983257621,
-1.));
#37747=CARTESIAN_POINT('Ctrl Pts',(-0.0155579084828646,-0.167846446705308,
-1.));
#37748=CARTESIAN_POINT('Ctrl Pts',(-0.0252161982402266,-0.165435252063536,
-1.));
#37749=CARTESIAN_POINT('Ctrl Pts',(-0.0346084283051884,-0.162213857880575,
-1.));
#37750=CARTESIAN_POINT('Ctrl Pts',(-0.0398245124126221,-0.160424819187389,
-1.));
#37751=CARTESIAN_POINT('Ctrl Pts',(-0.0449583344912096,-0.158385421116544,
-1.));
#37752=CARTESIAN_POINT('Ctrl Pts',(-0.0499880468050878,-0.156099392746595,
-1.));
#37753=CARTESIAN_POINT('Ctrl Pts',(-0.0531388312209868,-0.154667346117912,
-1.));
#37754=CARTESIAN_POINT('Ctrl Pts',(-0.0562487211166722,-0.153138476967067,
-1.));
#37755=CARTESIAN_POINT('Ctrl Pts',(-0.0593118554215172,-0.151513352468256,
-1.));
#37756=CARTESIAN_POINT('Ctrl Pts',(-0.0624652902574377,-0.149840319653745,
-1.));
#37757=CARTESIAN_POINT('Ctrl Pts',(-0.0655619449577883,-0.14806899457065,
-1.));
#37758=CARTESIAN_POINT('Ctrl Pts',(-0.0685920735998228,-0.146203692832195,
-1.));
#37759=CARTESIAN_POINT('Ctrl Pts',(-0.0777376759071703,-0.140573797240811,
-1.));
#37760=CARTESIAN_POINT('Ctrl Pts',(-0.086293321868111,-0.13408301355852,
-1.));
#37761=CARTESIAN_POINT('Ctrl Pts',(-0.0940925019796224,-0.126763144612894,
-1.));
#37762=CARTESIAN_POINT('Ctrl Pts',(-0.0988370020441118,-0.122310225435747,
-1.));
#37763=CARTESIAN_POINT('Ctrl Pts',(-0.103300876049684,-0.117549871947081,
-1.));
#37764=CARTESIAN_POINT('Ctrl Pts',(-0.107438039834494,-0.112484977203721,
-1.));
#37765=CARTESIAN_POINT('Origin',(0.,0.,-1.));
#37766=CARTESIAN_POINT('Origin',(0.,0.,-1.18400562256037));
#37767=CARTESIAN_POINT('Ctrl Pts',(-0.134962346407334,-0.141302247159154,
-1.02300740822721));
#37768=CARTESIAN_POINT('Ctrl Pts',(-0.0879512268871996,-0.186204087895818,
-1.01930085964667));
#37769=CARTESIAN_POINT('Ctrl Pts',(0.0535947059270241,-0.224620144876903,
-1.01188776248561));
#37770=CARTESIAN_POINT('Ctrl Pts',(0.218160338720414,-0.0763889482965145,
-1.00076811674401));
#37771=CARTESIAN_POINT('Ctrl Pts',(0.182250900350768,0.141814812868076,
-0.989648471002405));
#37772=CARTESIAN_POINT('Ctrl Pts',(-0.020335578424721,0.230093582492485,
-0.978528825260807));
#37773=CARTESIAN_POINT('Ctrl Pts',(-0.204446822720336,0.107559487262165,
-0.967409179519207));
#37774=CARTESIAN_POINT('Ctrl Pts',(-0.201163147192314,-0.113518873259326,
-0.956289533777606));
#37775=CARTESIAN_POINT('Ctrl Pts',(-0.0136177717725777,-0.23059244536116,
-0.945169888036007));
#37776=CARTESIAN_POINT('Ctrl Pts',(0.186426678942524,-0.136398090256529,
-0.934050242294405));
#37777=CARTESIAN_POINT('Ctrl Pts',(0.215656133902945,0.0827633194859286,
-0.922930596552807));
#37778=CARTESIAN_POINT('Ctrl Pts',(0.0473087718922573,0.226097493403868,
-0.911810950811205));
#37779=CARTESIAN_POINT('Ctrl Pts',(-0.164385906299704,0.16228226783603,
-0.900691305069606));
#37780=CARTESIAN_POINT('Ctrl Pts',(-0.225469354113307,-0.0502151067302932,
-0.889571659328005));
#37781=CARTESIAN_POINT('Ctrl Pts',(-0.0799798472802848,-0.216705673394779,
-0.878452013586406));
#37782=CARTESIAN_POINT('Ctrl Pts',(0.138787254209544,-0.184651617385904,
-0.867332367844805));
#37783=CARTESIAN_POINT('Ctrl Pts',(0.230397943777862,0.0165792908334795,
-0.856212722103206));
#37784=CARTESIAN_POINT('Ctrl Pts',(0.110919360557233,0.202620340500548,
-0.845093076361604));
#37785=CARTESIAN_POINT('Ctrl Pts',(-0.110183034939153,0.203021682345978,
-0.833973430620007));
#37786=CARTESIAN_POINT('Ctrl Pts',(-0.230336268383591,0.0174156105429483,
-0.822853784878404));
#37787=CARTESIAN_POINT('Ctrl Pts',(-0.139456624242068,-0.18414655373536,
-0.811734139136807));
#37788=CARTESIAN_POINT('Ctrl Pts',(0.079192466865668,-0.21699459881069,
-0.800614493395203));
#37789=CARTESIAN_POINT('Ctrl Pts',(0.225285824667576,-0.0510333160814544,
-0.789494847653607));
#37790=CARTESIAN_POINT('Ctrl Pts',(0.164973479123837,0.161684426641202,
-0.778375201912004));
#37791=CARTESIAN_POINT('Ctrl Pts',(-0.0464867152313373,0.226267734821794,
-0.767255556170406));
#37792=CARTESIAN_POINT('Ctrl Pts',(-0.215356021036036,0.083545715935049,
-0.756135910428805));
#37793=CARTESIAN_POINT('Ctrl Pts',(-0.18691725583042,-0.135720455315325,
-0.745016264687205));
#37794=CARTESIAN_POINT('Ctrl Pts',(0.0127741315575716,-0.230640248134116,
-0.733896618945605));
#37795=CARTESIAN_POINT('Ctrl Pts',(0.200761925645074,-0.114248639819529,
-0.722776973204004));
#37796=CARTESIAN_POINT('Ctrl Pts',(0.204812683015893,0.106816980743676,
-0.711657327462405));
#37797=CARTESIAN_POINT('Ctrl Pts',(0.0212151206534201,0.230017436624418,
-0.700537681720805));
#37798=CARTESIAN_POINT('Ctrl Pts',(-0.181819625388585,0.142477108050848,
-0.689418035979204));
#37799=CARTESIAN_POINT('Ctrl Pts',(-0.218272172080734,-0.0756000092032434,
-0.678298390237605));
#37800=CARTESIAN_POINT('Ctrl Pts',(-0.0547448848744599,-0.224412789465829,
-0.667178744496004));
#37801=CARTESIAN_POINT('Ctrl Pts',(0.15893938239428,-0.167619733980953,
-0.656059098754404));
#37802=CARTESIAN_POINT('Ctrl Pts',(0.227004210468479,0.0427456538784019,
-0.644939453012805));
#37803=CARTESIAN_POINT('Ctrl Pts',(0.0870889562897442,0.213947694982147,
-0.633819807271204));
#37804=CARTESIAN_POINT('Ctrl Pts',(-0.132616748713462,0.189131965718346,
-0.622700161529604));
#37805=CARTESIAN_POINT('Ctrl Pts',(-0.230819675206534,-0.00896549125201681,
-0.611580515788004));
#37806=CARTESIAN_POINT('Ctrl Pts',(-0.117546810409861,-0.198848811558663,
-0.600460870046404));
#37807=CARTESIAN_POINT('Ctrl Pts',(0.103421833452207,-0.206547880311589,
-0.589341224304804));
#37808=CARTESIAN_POINT('Ctrl Pts',(0.229635929001371,-0.0250088505834818,
-0.578221578563204));
#37809=CARTESIAN_POINT('Ctrl Pts',(0.145458775404855,0.179443158558768,
-0.567101932821604));
#37810=CARTESIAN_POINT('Ctrl Pts',(-0.0719869550633662,0.219490274947508,
-0.555982287080004));
#37811=CARTESIAN_POINT('Ctrl Pts',(-0.223478610035487,0.0584415379027191,
-0.544862641338404));
#37812=CARTESIAN_POINT('Ctrl Pts',(-0.17022031961721,-0.156151033570842,
-0.533742995596803));
#37813=CARTESIAN_POINT('Ctrl Pts',(0.0389929462701933,-0.227678836603225,
-0.522623349855203));
#37814=CARTESIAN_POINT('Ctrl Pts',(0.212481076681926,-0.0906084684117187,
-0.511503704113604));
#37815=CARTESIAN_POINT('Ctrl Pts',(0.191295144818936,0.129476909387466,
-0.500384058372003));
#37816=CARTESIAN_POINT('Ctrl Pts',(-0.00515440824209666,0.230936213209409,
-0.489264412630403));
#37817=CARTESIAN_POINT('Ctrl Pts',(-0.196881519160137,0.120812954226874,
-0.478144766888803));
#37818=CARTESIAN_POINT('Ctrl Pts',(-0.208226801633768,-0.0999985078748647,
-0.467025121147203));
#37819=CARTESIAN_POINT('Ctrl Pts',(-0.0287957666040805,-0.229191854832389,
-0.455905475405603));
#37820=CARTESIAN_POINT('Ctrl Pts',(0.177017800689991,-0.148400811098552,
-0.444785829664003));
#37821=CARTESIAN_POINT('Ctrl Pts',(0.220648575551937,0.0683542873763441,
-0.433666183922403));
#37822=CARTESIAN_POINT('Ctrl Pts',(0.0621222679640238,0.222483541680797,
-0.422546538180802));
#37823=CARTESIAN_POINT('Ctrl Pts',(-0.153320139876834,0.172774527069206,
-0.411426892439203));
#37824=CARTESIAN_POINT('Ctrl Pts',(-0.228291429421142,-0.0352296146539616,
-0.400307246697602));
#37825=CARTESIAN_POINT('Ctrl Pts',(-0.0941032933737792,-0.210956565842401,
-0.389187600956003));
#37826=CARTESIAN_POINT('Ctrl Pts',(0.126301792816278,-0.193406203693944,
-0.378067955214402));
#37827=CARTESIAN_POINT('Ctrl Pts',(0.230989830391116,0.00134192086369089,
-0.366948309472803));
#37828=CARTESIAN_POINT('Ctrl Pts',(0.124046181378033,0.194860584473312,
-0.355828663731202));
#37829=CARTESIAN_POINT('Ctrl Pts',(-0.0965479367307507,0.209848989536302,
-0.344709017989603));
#37830=CARTESIAN_POINT('Ctrl Pts',(-0.228685335108273,0.0325748369358222,
-0.333589372248002));
#37831=CARTESIAN_POINT('Ctrl Pts',(-0.151302413548674,-0.174544212593695,
-0.322469726506402));
#37832=CARTESIAN_POINT('Ctrl Pts',(0.0647029959036807,-0.221746758308778,
-0.311350080764802));
#37833=CARTESIAN_POINT('Ctrl Pts',(0.22142785550674,-0.065786072196304,
-0.300230435023202));
#37834=CARTESIAN_POINT('Ctrl Pts',(0.175281660439362,0.15044747259438,-0.289110789281602));
#37835=CARTESIAN_POINT('Ctrl Pts',(-0.031456684426298,0.228841822058552,
-0.277991143540001));
#37836=CARTESIAN_POINT('Ctrl Pts',(-0.209374577754782,0.0975724788943068,
-0.266871497798402));
#37837=CARTESIAN_POINT('Ctrl Pts',(-0.195464567310726,-0.123092263934074,
-0.255751852056802));
#37838=CARTESIAN_POINT('Ctrl Pts',(-0.0024709318560192,-0.230980512442675,
-0.244632206315202));
#37839=CARTESIAN_POINT('Ctrl Pts',(0.192786557592405,-0.127245610368647,
-0.233512560573602));
#37840=CARTESIAN_POINT('Ctrl Pts',(0.211414003045909,0.0930710590752383,
-0.222392914832001));
#37841=CARTESIAN_POINT('Ctrl Pts',(0.0363450300153787,0.228116509904006,
-0.211273269090402));
#37842=CARTESIAN_POINT('Ctrl Pts',(-0.172023064569064,0.154162788245832,
-0.200153623348801));
#37843=CARTESIAN_POINT('Ctrl Pts',(-0.222784530965761,-0.0610340679732166,
-0.189033977607201));
#37844=CARTESIAN_POINT('Ctrl Pts',(-0.0694319391096267,-0.220311853431586,
-0.177914331865601));
#37845=CARTESIAN_POINT('Ctrl Pts',(0.147533789176124,-0.17774100942929,
-0.166794686124001));
#37846=CARTESIAN_POINT('Ctrl Pts',(0.229329912608031,0.0276751317512237,
-0.155675040382401));
#37847=CARTESIAN_POINT('Ctrl Pts',(0.10101498825337,0.207735642104657,-0.144555394640801));
#37848=CARTESIAN_POINT('Ctrl Pts',(-0.119849022951734,0.197469486973865,
-0.133435748899201));
#37849=CARTESIAN_POINT('Ctrl Pts',(-0.230908593740765,0.00628346883829749,
-0.122316103157601));
#37850=CARTESIAN_POINT('Ctrl Pts',(-0.130409737561855,-0.19066068491043,
-0.111196457416001));
#37851=CARTESIAN_POINT('Ctrl Pts',(0.0895676188451145,-0.212920118346556,
-0.100076811674401));
#37852=CARTESIAN_POINT('Ctrl Pts',(0.227487825795308,-0.0401077892944868,
-0.0889571659328005));
#37853=CARTESIAN_POINT('Ctrl Pts',(0.156976791925724,0.169459748502108,
-0.0778375201912006));
#37854=CARTESIAN_POINT('Ctrl Pts',(-0.0573401927066776,0.223752650654119,
-0.0667178744496004));
#37855=CARTESIAN_POINT('Ctrl Pts',(-0.219151667511382,0.0730759416464898,
-0.0555982287080003));
#37856=CARTESIAN_POINT('Ctrl Pts',(-0.180121743363499,-0.144612413097174,
-0.0444785829664003));
#37857=CARTESIAN_POINT('Ctrl Pts',(0.0238283851653625,-0.229693360565524,
-0.0333589372248002));
#37858=CARTESIAN_POINT('Ctrl Pts',(0.206151341171209,-0.104550606625525,
-0.0222392914832002));
#37859=CARTESIAN_POINT('Ctrl Pts',(0.199196267801896,0.116822296166958,
-0.0111196457416001));
#37860=CARTESIAN_POINT('Ctrl Pts',(0.0734855601112398,0.192372693268079,
-0.00370654858053334));
#37861=CARTESIAN_POINT('Ctrl Pts',(0.00853826423430722,0.195213365433479,
0.));
#37862=CARTESIAN_POINT('Ctrl Pts',(-0.125787577549722,-0.131696490507342,
-1.01533827215147));
#37863=CARTESIAN_POINT('Ctrl Pts',(-0.0819722838789168,-0.173545894612556,
-1.01163172357094));
#37864=CARTESIAN_POINT('Ctrl Pts',(0.049951326481116,-0.209350419913845,
-1.00421862640987));
#37865=CARTESIAN_POINT('Ctrl Pts',(0.20332975274633,-0.0711960114326169,
-0.99309898066827));
#37866=CARTESIAN_POINT('Ctrl Pts',(0.169861445593043,0.132174211890948,
-0.981979334926672));
#37867=CARTESIAN_POINT('Ctrl Pts',(-0.0189531615017859,0.214451772082513,
-0.97085968918507));
#37868=CARTESIAN_POINT('Ctrl Pts',(-0.190548484464784,0.100247570565819,
-0.959740043443472));
#37869=CARTESIAN_POINT('Ctrl Pts',(-0.187488033893757,-0.105801836242295,
-0.948620397701869));
#37870=CARTESIAN_POINT('Ctrl Pts',(-0.0126920327668837,-0.21491672214785,
-0.937500751960273));
#37871=CARTESIAN_POINT('Ctrl Pts',(0.173753353872823,-0.127125719228342,
-0.926381106218669));
#37872=CARTESIAN_POINT('Ctrl Pts',(0.200995784302071,0.0771370515201939,
-0.915261460477071));
#37873=CARTESIAN_POINT('Ctrl Pts',(0.0440927115717062,0.210727337975441,
-0.904141814735469));
#37874=CARTESIAN_POINT('Ctrl Pts',(-0.153210917616587,0.151250284940659,
-0.893022168993871));
#37875=CARTESIAN_POINT('Ctrl Pts',(-0.210141899726723,-0.0468014731526719,
-0.881902523252271));
#37876=CARTESIAN_POINT('Ctrl Pts',(-0.074542800343881,-0.201973975877239,
-0.87078287751067));
#37877=CARTESIAN_POINT('Ctrl Pts',(0.129352467310449,-0.172098961376302,
-0.85966323176907));
#37878=CARTESIAN_POINT('Ctrl Pts',(0.214735442823328,0.0154522271355718,
-0.84854358602747));
#37879=CARTESIAN_POINT('Ctrl Pts',(0.103379038963568,0.188846166892656,
-0.83742394028587));
#37880=CARTESIAN_POINT('Ctrl Pts',(-0.102692768916763,0.189220225434536,
-0.826304294544271));
#37881=CARTESIAN_POINT('Ctrl Pts',(-0.214677960135406,0.0162316936542803,
-0.815184648802669));
#37882=CARTESIAN_POINT('Ctrl Pts',(-0.129976333426566,-0.171628232059561,
-0.804065003061071));
#37883=CARTESIAN_POINT('Ctrl Pts',(0.0738089462164079,-0.20224326008226,
-0.792945357319469));
#37884=CARTESIAN_POINT('Ctrl Pts',(0.209970846651535,-0.0475640604590616,
-0.78182571157787));
#37885=CARTESIAN_POINT('Ctrl Pts',(0.153758547115844,0.15069308511672,-0.77070606583627));
#37886=CARTESIAN_POINT('Ctrl Pts',(-0.0433265384964888,0.210886006345764,
-0.759586420094669));
#37887=CARTESIAN_POINT('Ctrl Pts',(-0.200716073171338,0.0778662604931993,
-0.74846677435307));
#37888=CARTESIAN_POINT('Ctrl Pts',(-0.174210581240105,-0.126494150053784,
-0.737347128611469));
#37889=CARTESIAN_POINT('Ctrl Pts',(0.0119057433921528,-0.214961275278188,
-0.726227482869869));
#37890=CARTESIAN_POINT('Ctrl Pts',(0.187114087472171,-0.106481993117365,
-0.715107837128269));
#37891=CARTESIAN_POINT('Ctrl Pts',(0.190889473500056,0.0995555397975229,
-0.703988191386669));
#37892=CARTESIAN_POINT('Ctrl Pts',(0.0197729122637246,0.214380802626665,
-0.69286854564507));
#37893=CARTESIAN_POINT('Ctrl Pts',(-0.169459488794018,0.132791484107098,
-0.681748899903469));
#37894=CARTESIAN_POINT('Ctrl Pts',(-0.203433983651159,-0.0704607045857945,
-0.670629254161869));
#37895=CARTESIAN_POINT('Ctrl Pts',(-0.0510233160204035,-0.209157160567478,
-0.659509608420268));
#37896=CARTESIAN_POINT('Ctrl Pts',(0.148134649558368,-0.156224909008006,
-0.648389962678669));
#37897=CARTESIAN_POINT('Ctrl Pts',(0.2115724162222,0.0398397952856799,-0.637270316937069));
#37898=CARTESIAN_POINT('Ctrl Pts',(0.081168630619074,0.199403485420499,
-0.626150671195468));
#37899=CARTESIAN_POINT('Ctrl Pts',(-0.123601434083249,0.176274734681368,
-0.615031025453869));
#37900=CARTESIAN_POINT('Ctrl Pts',(-0.21512850486027,-0.00835601526021841,
-0.603911379712268));
#37901=CARTESIAN_POINT('Ctrl Pts',(-0.109555953373298,-0.185331027286038,
-0.592791733970669));
#37902=CARTESIAN_POINT('Ctrl Pts',(0.0963911953371101,-0.192506711716541,
-0.581672088229068));
#37903=CARTESIAN_POINT('Ctrl Pts',(0.214025229972533,-0.023308743630646,
-0.570552442487468));
#37904=CARTESIAN_POINT('Ctrl Pts',(0.135570457083661,0.167244574681991,
-0.559432796745868));
#37905=CARTESIAN_POINT('Ctrl Pts',(-0.0670932666306222,0.204569279627381,
-0.548313151004268));
#37906=CARTESIAN_POINT('Ctrl Pts',(-0.20828648685242,0.0544686697938416,
-0.537193505262669));
#37907=CARTESIAN_POINT('Ctrl Pts',(-0.158648706282604,-0.145535853277772,
-0.526073859521068));
#37908=CARTESIAN_POINT('Ctrl Pts',(0.0363421975344947,-0.2122011811296,
-0.514954213779468));
#37909=CARTESIAN_POINT('Ctrl Pts',(0.198036568142563,-0.0844488855625077,
-0.503834568037868));
#37910=CARTESIAN_POINT('Ctrl Pts',(0.178290860409118,0.12067504169881,-0.492714922296268));
#37911=CARTESIAN_POINT('Ctrl Pts',(-0.00480401047947801,0.215237120585057,
-0.481595276554667));
#37912=CARTESIAN_POINT('Ctrl Pts',(-0.18349747184091,0.112600064042736,
-0.470475630813068));
#37913=CARTESIAN_POINT('Ctrl Pts',(-0.194071499612093,-0.0932005881566582,
-0.459355985071467));
#37914=CARTESIAN_POINT('Ctrl Pts',(-0.0268382242991108,-0.213611344059494,
-0.448236339329868));
#37915=CARTESIAN_POINT('Ctrl Pts',(0.164984093154174,-0.138312492568566,
-0.437116693588267));
#37916=CARTESIAN_POINT('Ctrl Pts',(0.205648838711703,0.0637075484613892,
-0.425997047846667));
#37917=CARTESIAN_POINT('Ctrl Pts',(0.0578991830469871,0.20735906345497,
-0.414877402105067));
#37918=CARTESIAN_POINT('Ctrl Pts',(-0.142897404335907,0.161029278171717,
-0.403757756363467));
#37919=CARTESIAN_POINT('Ctrl Pts',(-0.212772129758173,-0.0328346979975991,
-0.392638110621867));
#37920=CARTESIAN_POINT('Ctrl Pts',(-0.0877061315843801,-0.196615693872392,
-0.381518464880267));
#37921=CARTESIAN_POINT('Ctrl Pts',(0.11771577022377,-0.180258409055248,
-0.370398819138667));
#37922=CARTESIAN_POINT('Ctrl Pts',(0.21528709285941,0.00125069679951916,
-0.359279173397067));
#37923=CARTESIAN_POINT('Ctrl Pts',(0.115613495728229,0.181613920721587,
-0.348159527655467));
#37924=CARTESIAN_POINT('Ctrl Pts',(-0.0899845875688268,0.195583410837868,
-0.337039881913867));
#37925=CARTESIAN_POINT('Ctrl Pts',(-0.213139257653369,0.0303603926303067,
-0.325920236172267));
#37926=CARTESIAN_POINT('Ctrl Pts',(-0.141016843470348,-0.162678660099908,
-0.314800590430666));
#37927=CARTESIAN_POINT('Ctrl Pts',(0.0603044725554018,-0.206672366772434,
-0.303680944689067));
#37928=CARTESIAN_POINT('Ctrl Pts',(0.206375143050337,-0.0613139210925453,
-0.292561298947466));
#37929=CARTESIAN_POINT('Ctrl Pts',(0.163365976085031,0.140220021582975,
-0.281441653205867));
#37930=CARTESIAN_POINT('Ctrl Pts',(-0.029318252364907,0.213285106587666,
-0.270322007464266));
#37931=CARTESIAN_POINT('Ctrl Pts',(-0.19514124966961,0.0909394811393789,
-0.259202361722666));
#37932=CARTESIAN_POINT('Ctrl Pts',(-0.182176844677951,-0.114724425793896,
-0.248082715981066));
#37933=CARTESIAN_POINT('Ctrl Pts',(-0.00230295738576517,-0.215278408347075,
-0.236963070239466));
#37934=CARTESIAN_POINT('Ctrl Pts',(0.179680886626768,-0.118595426859279,
-0.225843424497866));
#37935=CARTESIAN_POINT('Ctrl Pts',(0.197042034398042,0.0867440687918065,
-0.214723778756266));
#37936=CARTESIAN_POINT('Ctrl Pts',(0.0338742871867991,0.212609101306813,
-0.203604133014666));
#37937=CARTESIAN_POINT('Ctrl Pts',(-0.160328900251294,0.143682769290532,
-0.192484487273066));
#37938=CARTESIAN_POINT('Ctrl Pts',(-0.207639591424673,-0.0568849591217459,
-0.181364841531466));
#37939=CARTESIAN_POINT('Ctrl Pts',(-0.0647119412018833,-0.205335007032323,
-0.170245195789866));
#37940=CARTESIAN_POINT('Ctrl Pts',(0.137504410979829,-0.165658138010392,
-0.159125550048266));
#37941=CARTESIAN_POINT('Ctrl Pts',(0.213740016638345,0.0257937704406031,
-0.148005904306665));
#37942=CARTESIAN_POINT('Ctrl Pts',(0.0941479679840126,0.193613729211668,
-0.136886258565066));
#37943=CARTESIAN_POINT('Ctrl Pts',(-0.111701661019585,0.184045469478285,
-0.125766612823465));
#37944=CARTESIAN_POINT('Ctrl Pts',(-0.215211378693734,0.00585631729751509,
-0.114646967081866));
#37945=CARTESIAN_POINT('Ctrl Pts',(-0.121544456016579,-0.177699531219403,
-0.103527321340265));
#37946=CARTESIAN_POINT('Ctrl Pts',(0.0834787931696162,-0.198445763661959,
-0.0924076755986652));
#37947=CARTESIAN_POINT('Ctrl Pts',(0.212023155276811,-0.0373812532941696,
-0.081288029857065));
#37948=CARTESIAN_POINT('Ctrl Pts',(0.146305476405014,0.157939838952792,
-0.0701683841154652));
#37949=CARTESIAN_POINT('Ctrl Pts',(-0.0534421942771988,0.208541898131829,
-0.0590487383738648));
#37950=CARTESIAN_POINT('Ctrl Pts',(-0.20425369079639,0.0681082236754674,
-0.0479290926322649));
#37951=CARTESIAN_POINT('Ctrl Pts',(-0.167877029148153,-0.134781630664691,
-0.0368094468906647));
#37952=CARTESIAN_POINT('Ctrl Pts',(0.0222085265013588,-0.214078757326807,
-0.0256898011490648));
#37953=CARTESIAN_POINT('Ctrl Pts',(0.192137129390805,-0.0974432342713328,
-0.0145701554074646));
#37954=CARTESIAN_POINT('Ctrl Pts',(0.185654863380358,0.108880691761887,
-0.00345050966586461));
#37955=CARTESIAN_POINT('Ctrl Pts',(0.0684899961903367,0.179295156886754,
0.00396258749520215));
#37956=CARTESIAN_POINT('Ctrl Pts',(0.00795783122554286,0.181942719557457,
0.00766913607573549));
#37957=CARTESIAN_POINT('Ctrl Pts',(-0.116612808692109,-0.122090733855531,
-1.00766913607574));
#37958=CARTESIAN_POINT('Ctrl Pts',(-0.0759933408706338,-0.160887701329294,
-1.0039625874952));
#37959=CARTESIAN_POINT('Ctrl Pts',(0.0463079470352078,-0.194080694950787,
-0.996549490334135));
#37960=CARTESIAN_POINT('Ctrl Pts',(0.188499166772245,-0.0660030745687196,
-0.985429844592535));
#37961=CARTESIAN_POINT('Ctrl Pts',(0.157471990835318,0.12253361091382,-0.974310198850936));
#37962=CARTESIAN_POINT('Ctrl Pts',(-0.0175707445788509,0.198809961672541,
-0.963190553109335));
#37963=CARTESIAN_POINT('Ctrl Pts',(-0.17665014620923,0.0929356538694735,
-0.952070907367737));
#37964=CARTESIAN_POINT('Ctrl Pts',(-0.1738129205952,-0.0980847992252637,
-0.940951261626134));
#37965=CARTESIAN_POINT('Ctrl Pts',(-0.0117662937611897,-0.19924099893454,
-0.929831615884536));
#37966=CARTESIAN_POINT('Ctrl Pts',(0.161080028803121,-0.117853348200155,
-0.918711970142934));
#37967=CARTESIAN_POINT('Ctrl Pts',(0.186335434701197,0.0715107835544593,
-0.907592324401336));
#37968=CARTESIAN_POINT('Ctrl Pts',(0.0408766512511551,0.195357182547014,
-0.896472678659735));
#37969=CARTESIAN_POINT('Ctrl Pts',(-0.142035928933471,0.140218302045289,
-0.885353032918135));
#37970=CARTESIAN_POINT('Ctrl Pts',(-0.194814445340139,-0.0433878395750506,
-0.874233387176535));
#37971=CARTESIAN_POINT('Ctrl Pts',(-0.0691057534074772,-0.1872422783597,
-0.863113741434934));
#37972=CARTESIAN_POINT('Ctrl Pts',(0.119917680411353,-0.1595463053667,-0.851994095693335));
#37973=CARTESIAN_POINT('Ctrl Pts',(0.199072941868794,0.014325163437664,
-0.840874449951735));
#37974=CARTESIAN_POINT('Ctrl Pts',(0.0958387173699031,0.175071993284764,
-0.829754804210135));
#37975=CARTESIAN_POINT('Ctrl Pts',(-0.0952025028943739,0.175418768523093,
-0.818635158468535));
#37976=CARTESIAN_POINT('Ctrl Pts',(-0.199019651887221,0.0150477767656126,
-0.807515512726934));
#37977=CARTESIAN_POINT('Ctrl Pts',(-0.120496042611065,-0.159109910383761,
-0.796395866985335));
#37978=CARTESIAN_POINT('Ctrl Pts',(0.068425425567148,-0.187491921353828,
-0.785276221243733));
#37979=CARTESIAN_POINT('Ctrl Pts',(0.194655868635495,-0.0440948048366693,
-0.774156575502135));
#37980=CARTESIAN_POINT('Ctrl Pts',(0.142543615107852,0.139701743592238,
-0.763036929760534));
#37981=CARTESIAN_POINT('Ctrl Pts',(-0.0401663617616404,0.195504277869735,
-0.751917284018934));
#37982=CARTESIAN_POINT('Ctrl Pts',(-0.18607612530664,0.0721868050513496,
-0.740797638277334));
#37983=CARTESIAN_POINT('Ctrl Pts',(-0.16150390664979,-0.117267844792243,
-0.729677992535734));
#37984=CARTESIAN_POINT('Ctrl Pts',(0.0110373552267338,-0.199282302422261,
-0.718558346794134));
#37985=CARTESIAN_POINT('Ctrl Pts',(0.173466249299268,-0.0987153464152002,
-0.707438701052533));
#37986=CARTESIAN_POINT('Ctrl Pts',(0.176966263984219,0.0922940988513697,
-0.696319055310934));
#37987=CARTESIAN_POINT('Ctrl Pts',(0.0183307038740293,0.198744168628912,
-0.685199409569334));
#37988=CARTESIAN_POINT('Ctrl Pts',(-0.157099352199452,0.123105860163347,
-0.674079763827732));
#37989=CARTESIAN_POINT('Ctrl Pts',(-0.188595795221582,-0.0653213999683454,
-0.662960118086134));
#37990=CARTESIAN_POINT('Ctrl Pts',(-0.0473017471663473,-0.193901531669128,
-0.651840472344532));
#37991=CARTESIAN_POINT('Ctrl Pts',(0.137329916722456,-0.144830084035059,
-0.640720826602934));
#37992=CARTESIAN_POINT('Ctrl Pts',(0.19614062197592,0.0369339366929576,
-0.629601180861333));
#37993=CARTESIAN_POINT('Ctrl Pts',(0.0752483049484038,0.184859275858851,
-0.618481535119733));
#37994=CARTESIAN_POINT('Ctrl Pts',(-0.114586119453036,0.16341750364439,
-0.607361889378132));
#37995=CARTESIAN_POINT('Ctrl Pts',(-0.199437334514005,-0.00774653926841995,
-0.596242243636534));
#37996=CARTESIAN_POINT('Ctrl Pts',(-0.101565096336734,-0.171813243013414,
-0.585122597894932));
#37997=CARTESIAN_POINT('Ctrl Pts',(0.089360557222013,-0.178465543121493,
-0.574002952153333));
#37998=CARTESIAN_POINT('Ctrl Pts',(0.198414530943696,-0.0216086366778103,
-0.562883306411733));
#37999=CARTESIAN_POINT('Ctrl Pts',(0.125682138762467,0.155045990805214,
-0.551763660670133));
#38000=CARTESIAN_POINT('Ctrl Pts',(-0.062199578197878,0.189648284307254,
-0.540644014928533));
#38001=CARTESIAN_POINT('Ctrl Pts',(-0.193094363669353,0.0504958016849643,
-0.529524369186932));
#38002=CARTESIAN_POINT('Ctrl Pts',(-0.147077092947998,-0.134920672984703,
-0.518404723445333));
#38003=CARTESIAN_POINT('Ctrl Pts',(0.033691448798796,-0.196723525655976,
-0.507285077703731));
#38004=CARTESIAN_POINT('Ctrl Pts',(0.1835920596032,-0.0782893027132967,
-0.496165431962133));
#38005=CARTESIAN_POINT('Ctrl Pts',(0.165286575999301,0.111873174010154,
-0.485045786220532));
#38006=CARTESIAN_POINT('Ctrl Pts',(-0.0044536127168597,0.199538027960706,
-0.473926140478932));
#38007=CARTESIAN_POINT('Ctrl Pts',(-0.170113424521682,0.104387173858599,
-0.462806494737332));
#38008=CARTESIAN_POINT('Ctrl Pts',(-0.179916197590418,-0.0864026684384514,
-0.451686848995732));
#38009=CARTESIAN_POINT('Ctrl Pts',(-0.0248806819941409,-0.1980308332866,
-0.440567203254132));
#38010=CARTESIAN_POINT('Ctrl Pts',(0.152950385618357,-0.12822417403858,
-0.429447557512532));
#38011=CARTESIAN_POINT('Ctrl Pts',(0.19064910187147,0.0590608095464339,
-0.418327911770931));
#38012=CARTESIAN_POINT('Ctrl Pts',(0.0536760981299502,0.192234585229143,
-0.407208266029333));
#38013=CARTESIAN_POINT('Ctrl Pts',(-0.13247466879498,0.149284029274227,
-0.396088620287731));
#38014=CARTESIAN_POINT('Ctrl Pts',(-0.197252830095204,-0.0304397813412365,
-0.384968974546132));
#38015=CARTESIAN_POINT('Ctrl Pts',(-0.0813089697949813,-0.182274821902383,
-0.373849328804531));
#38016=CARTESIAN_POINT('Ctrl Pts',(0.109129747631262,-0.167110614416551,
-0.362729683062932));
#38017=CARTESIAN_POINT('Ctrl Pts',(0.199584355327704,0.00115947273534765,
-0.351610037321331));
#38018=CARTESIAN_POINT('Ctrl Pts',(0.107180810078425,0.168367256969862,
-0.340490391579731));
#38019=CARTESIAN_POINT('Ctrl Pts',(-0.0834212384069029,0.181317832139435,
-0.329370745838131));
#38020=CARTESIAN_POINT('Ctrl Pts',(-0.197593180198466,0.0281459483247914,
-0.318251100096531));
#38021=CARTESIAN_POINT('Ctrl Pts',(-0.130731273392021,-0.15081310760612,
-0.307131454354931));
#38022=CARTESIAN_POINT('Ctrl Pts',(0.0559059492071229,-0.191597975236089,
-0.296011808613331));
#38023=CARTESIAN_POINT('Ctrl Pts',(0.191322430593934,-0.0568417699887867,
-0.284892162871731));
#38024=CARTESIAN_POINT('Ctrl Pts',(0.151450291730699,0.129992570571571,
-0.273772517130131));
#38025=CARTESIAN_POINT('Ctrl Pts',(-0.0271798203035159,0.19772839111678,
-0.262652871388531));
#38026=CARTESIAN_POINT('Ctrl Pts',(-0.180907921584439,0.0843064833844511,
-0.251533225646931));
#38027=CARTESIAN_POINT('Ctrl Pts',(-0.168889122045176,-0.106356587653718,
-0.240413579905331));
#38028=CARTESIAN_POINT('Ctrl Pts',(-0.00213498291551102,-0.199576304251475,
-0.229293934163731));
#38029=CARTESIAN_POINT('Ctrl Pts',(0.16657521566113,-0.109945243349912,
-0.218174288422131));
#38030=CARTESIAN_POINT('Ctrl Pts',(0.182670065750174,0.0804170785083747,
-0.20705464268053));
#38031=CARTESIAN_POINT('Ctrl Pts',(0.0314035443582194,0.19710169270962,
-0.19593499693893));
#38032=CARTESIAN_POINT('Ctrl Pts',(-0.148634735933524,0.133202750335231,
-0.18481535119733));
#38033=CARTESIAN_POINT('Ctrl Pts',(-0.192494651883585,-0.0527358502702753,
-0.17369570545573));
#38034=CARTESIAN_POINT('Ctrl Pts',(-0.0599919432941398,-0.190358160633059,
-0.16257605971413));
#38035=CARTESIAN_POINT('Ctrl Pts',(0.127475032783534,-0.153575266591495,
-0.15145641397253));
#38036=CARTESIAN_POINT('Ctrl Pts',(0.198150120668658,0.023912409129983,
-0.14033676823093));
#38037=CARTESIAN_POINT('Ctrl Pts',(0.0872809477146552,0.179491816318678,
-0.12921712248933));
#38038=CARTESIAN_POINT('Ctrl Pts',(-0.103554299087435,0.170621451982705,
-0.11809747674773));
#38039=CARTESIAN_POINT('Ctrl Pts',(-0.199514163646704,0.00542916575673231,
-0.10697783100613));
#38040=CARTESIAN_POINT('Ctrl Pts',(-0.112679174471304,-0.164738377528375,
-0.09585818526453));
#38041=CARTESIAN_POINT('Ctrl Pts',(0.0773899674941174,-0.183971408977363,
-0.0847385395229295));
#38042=CARTESIAN_POINT('Ctrl Pts',(0.196558484758314,-0.0346547172938525,
-0.0736188937813297));
#38043=CARTESIAN_POINT('Ctrl Pts',(0.135634160884303,0.146419929403477,
-0.0624992480397295));
#38044=CARTESIAN_POINT('Ctrl Pts',(-0.0495441958477198,0.193331145609538,
-0.0513796022981294));
#38045=CARTESIAN_POINT('Ctrl Pts',(-0.189355714081398,0.0631405057044453,
-0.0402599565565294));
#38046=CARTESIAN_POINT('Ctrl Pts',(-0.155632314932806,-0.124950848232207,
-0.0291403108149293));
#38047=CARTESIAN_POINT('Ctrl Pts',(0.0205886678373547,-0.198464154088089,
-0.0180206650733292));
#38048=CARTESIAN_POINT('Ctrl Pts',(0.178122917610402,-0.09033586191714,
-0.00690101933172914));
#38049=CARTESIAN_POINT('Ctrl Pts',(0.172113458958819,0.100939087356816,
0.00421862640987089));
#38050=CARTESIAN_POINT('Ctrl Pts',(0.0634944322694335,0.166217620505429,
0.0116317235709377));
#38051=CARTESIAN_POINT('Ctrl Pts',(0.00737739821677849,0.168672073681435,
0.015338272151471));
#38052=CARTESIAN_POINT('Ctrl Pts',(-0.107438039834496,-0.112484977203719,
-1.));
#38053=CARTESIAN_POINT('Ctrl Pts',(-0.070014397862351,-0.148229508046032,
-0.996293451419467));
#38054=CARTESIAN_POINT('Ctrl Pts',(0.0426645675892999,-0.178810969987729,
-0.988880354258401));
#38055=CARTESIAN_POINT('Ctrl Pts',(0.173668580798161,-0.0608101377048221,
-0.977760708516799));
#38056=CARTESIAN_POINT('Ctrl Pts',(0.145082536077593,0.112893009936692,
-0.9666410627752));
#38057=CARTESIAN_POINT('Ctrl Pts',(-0.016188327655916,0.183168151262569,
-0.9555214170336));
#38058=CARTESIAN_POINT('Ctrl Pts',(-0.162751807953678,0.0856237371731279,
-0.944401771292001));
#38059=CARTESIAN_POINT('Ctrl Pts',(-0.160137807296644,-0.0903677622082326,
-0.933282125550398));
#38060=CARTESIAN_POINT('Ctrl Pts',(-0.0108405547554956,-0.183565275721231,
-0.922162479808802));
#38061=CARTESIAN_POINT('Ctrl Pts',(0.148406703733419,-0.108580977171968,
-0.911042834067198));
#38062=CARTESIAN_POINT('Ctrl Pts',(0.171675085100322,0.0658845155887245,
-0.899923188325601));
#38063=CARTESIAN_POINT('Ctrl Pts',(0.037660590930604,0.179987027118587,
-0.888803542583998));
#38064=CARTESIAN_POINT('Ctrl Pts',(-0.130860940250355,0.129186319149918,
-0.8776838968424));
#38065=CARTESIAN_POINT('Ctrl Pts',(-0.179486990953555,-0.0399742059974294,
-0.866564251100799));
#38066=CARTESIAN_POINT('Ctrl Pts',(-0.0636687064710734,-0.17251058084216,
-0.8554446053592));
#38067=CARTESIAN_POINT('Ctrl Pts',(0.110482893512257,-0.146993649357098,
-0.844324959617598));
#38068=CARTESIAN_POINT('Ctrl Pts',(0.18341044091426,0.0131980997397562,
-0.833205313875999));
#38069=CARTESIAN_POINT('Ctrl Pts',(0.0882983957762384,0.161297819676871,
-0.822085668134399));
#38070=CARTESIAN_POINT('Ctrl Pts',(-0.0877122368719845,0.161617311611651,
-0.810966022392799));
#38071=CARTESIAN_POINT('Ctrl Pts',(-0.183361343639036,0.0138638598769447,
-0.799846376651199));
#38072=CARTESIAN_POINT('Ctrl Pts',(-0.111015751795564,-0.146591588707962,
-0.7887267309096));
#38073=CARTESIAN_POINT('Ctrl Pts',(0.0630419049178878,-0.172740582625397,
-0.777607085167998));
#38074=CARTESIAN_POINT('Ctrl Pts',(0.179340890619455,-0.0406255492142766,
-0.766487439426399));
#38075=CARTESIAN_POINT('Ctrl Pts',(0.131328683099859,0.128710402067756,
-0.755367793684797));
#38076=CARTESIAN_POINT('Ctrl Pts',(-0.037006185026792,0.180122549393705,
-0.7442481479432));
#38077=CARTESIAN_POINT('Ctrl Pts',(-0.171436177441942,0.0665073496095001,
-0.733128502201597));
#38078=CARTESIAN_POINT('Ctrl Pts',(-0.148797232059476,-0.108041539530703,
-0.722008856459999));
#38079=CARTESIAN_POINT('Ctrl Pts',(0.0101689670613149,-0.183603329566334,
-0.710889210718397));
#38080=CARTESIAN_POINT('Ctrl Pts',(0.159818411126364,-0.0909486997130359,
-0.6997695649768));
#38081=CARTESIAN_POINT('Ctrl Pts',(0.163043054468382,0.0850326579052167,
-0.688649919235197));
#38082=CARTESIAN_POINT('Ctrl Pts',(0.0168884954843339,0.183107534631158,
-0.677530273493599));
#38083=CARTESIAN_POINT('Ctrl Pts',(-0.144739215604886,0.113420236219596,
-0.666410627751997));
#38084=CARTESIAN_POINT('Ctrl Pts',(-0.173757606792006,-0.0601820953508962,
-0.655290982010399));
#38085=CARTESIAN_POINT('Ctrl Pts',(-0.0435801783122908,-0.178645902770777,
-0.644171336268797));
#38086=CARTESIAN_POINT('Ctrl Pts',(0.126525183886544,-0.133435259062113,
-0.633051690527199));
#38087=CARTESIAN_POINT('Ctrl Pts',(0.180708827729641,0.0340280781002357,
-0.621932044785597));
#38088=CARTESIAN_POINT('Ctrl Pts',(0.0693279792777336,0.170315066297202,
-0.610812399043998));
#38089=CARTESIAN_POINT('Ctrl Pts',(-0.105570804822823,0.150560272607413,
-0.599692753302398));
#38090=CARTESIAN_POINT('Ctrl Pts',(-0.18374616416774,-0.00713706327662168,
-0.588573107560797));
#38091=CARTESIAN_POINT('Ctrl Pts',(-0.0935742393001708,-0.15829545874079,
-0.577453461819198));
#38092=CARTESIAN_POINT('Ctrl Pts',(0.0823299191069159,-0.164424374526445,
-0.566333816077597));
#38093=CARTESIAN_POINT('Ctrl Pts',(0.182803831914859,-0.0199085297249743,
-0.555214170335998));
#38094=CARTESIAN_POINT('Ctrl Pts',(0.115793820441273,0.142847406928437,
-0.544094524594397));
#38095=CARTESIAN_POINT('Ctrl Pts',(-0.057305889765134,0.174727288987128,
-0.532974878852797));
#38096=CARTESIAN_POINT('Ctrl Pts',(-0.177902240486286,0.0465229335760867,
-0.521855233111197));
#38097=CARTESIAN_POINT('Ctrl Pts',(-0.135505479613391,-0.124305492691633,
-0.510735587369597));
#38098=CARTESIAN_POINT('Ctrl Pts',(0.0310407000630972,-0.181245870182351,
-0.499615941627997));
#38099=CARTESIAN_POINT('Ctrl Pts',(0.169147551063838,-0.0721297198640855,
-0.488496295886397));
#38100=CARTESIAN_POINT('Ctrl Pts',(0.152282291589484,0.103071306321499,
-0.477376650144796));
#38101=CARTESIAN_POINT('Ctrl Pts',(-0.00410321495424111,0.183838935336354,
-0.466257004403197));
#38102=CARTESIAN_POINT('Ctrl Pts',(-0.156729377202455,0.096174283674461,
-0.455137358661596));
#38103=CARTESIAN_POINT('Ctrl Pts',(-0.165760895568743,-0.0796047487202445,
-0.444017712919997));
#38104=CARTESIAN_POINT('Ctrl Pts',(-0.0229231396891714,-0.182450322513706,
-0.432898067178396));
#38105=CARTESIAN_POINT('Ctrl Pts',(0.140916678082541,-0.118135855508594,
-0.421778421436797));
#38106=CARTESIAN_POINT('Ctrl Pts',(0.175649365031236,0.0544140706314786,
-0.410658775695196));
#38107=CARTESIAN_POINT('Ctrl Pts',(0.0494530132129136,0.177110107003317,
-0.399539129953596));
#38108=CARTESIAN_POINT('Ctrl Pts',(-0.122051933254053,0.137538780376738,
-0.388419484211996));
#38109=CARTESIAN_POINT('Ctrl Pts',(-0.181733530432234,-0.0280448646848738,
-0.377299838470396));
#38110=CARTESIAN_POINT('Ctrl Pts',(-0.0749118080055823,-0.167933949932374,
-0.366180192728796));
#38111=CARTESIAN_POINT('Ctrl Pts',(0.100543725038754,-0.153962819777854,
-0.355060546987196));
#38112=CARTESIAN_POINT('Ctrl Pts',(0.183881617795998,0.00106824867117576,
-0.343940901245595));
#38113=CARTESIAN_POINT('Ctrl Pts',(0.0987481244286207,0.155120593218137,
-0.332821255503996));
#38114=CARTESIAN_POINT('Ctrl Pts',(-0.0768578892449788,0.167052253441001,
-0.321701609762395));
#38115=CARTESIAN_POINT('Ctrl Pts',(-0.182047102743562,0.025931504019276,
-0.310581964020796));
#38116=CARTESIAN_POINT('Ctrl Pts',(-0.120445703313694,-0.138947555112332,
-0.299462318279195));
#38117=CARTESIAN_POINT('Ctrl Pts',(0.0515074258588442,-0.176523583699745,
-0.288342672537596));
#38118=CARTESIAN_POINT('Ctrl Pts',(0.176269718137531,-0.0523696188850282,
-0.277223026795995));
#38119=CARTESIAN_POINT('Ctrl Pts',(0.139534607376368,0.119765119560166,
-0.266103381054396));
#38120=CARTESIAN_POINT('Ctrl Pts',(-0.0250413882421251,0.182171675645894,
-0.254983735312795));
#38121=CARTESIAN_POINT('Ctrl Pts',(-0.166674593499267,0.0776734856295233,
-0.243864089571196));
#38122=CARTESIAN_POINT('Ctrl Pts',(-0.155601399412401,-0.0979887495135398,
-0.232744443829595));
#38123=CARTESIAN_POINT('Ctrl Pts',(-0.00196700844525682,-0.183874200155875,
-0.221624798087995));
#38124=CARTESIAN_POINT('Ctrl Pts',(0.153469544695492,-0.101295059840545,
-0.210505152346395));
#38125=CARTESIAN_POINT('Ctrl Pts',(0.168298097102307,0.074090088224943,
-0.199385506604795));
#38126=CARTESIAN_POINT('Ctrl Pts',(0.0289328015296395,0.181594284112427,
-0.188265860863195));
#38127=CARTESIAN_POINT('Ctrl Pts',(-0.136940571615754,0.122722731379931,
-0.177146215121595));
#38128=CARTESIAN_POINT('Ctrl Pts',(-0.177349712342497,-0.0485867414188046,
-0.166026569379995));
#38129=CARTESIAN_POINT('Ctrl Pts',(-0.0552719453863964,-0.175381314233795,
-0.154906923638395));
#38130=CARTESIAN_POINT('Ctrl Pts',(0.117445654587239,-0.141492395172598,
-0.143787277896795));
#38131=CARTESIAN_POINT('Ctrl Pts',(0.182560224698972,0.0220310478193626,
-0.132667632155195));
#38132=CARTESIAN_POINT('Ctrl Pts',(0.0804139274452977,0.165369903425689,
-0.121547986413595));
#38133=CARTESIAN_POINT('Ctrl Pts',(-0.0954069371552854,0.157197434487125,
-0.110428340671994));
#38134=CARTESIAN_POINT('Ctrl Pts',(-0.183816948599673,0.00500201421594969,
-0.0993086949303943));
#38135=CARTESIAN_POINT('Ctrl Pts',(-0.103813892926028,-0.151777223837348,
-0.0881890491887944));
#38136=CARTESIAN_POINT('Ctrl Pts',(0.0713011418186189,-0.169497054292766,
-0.0770694034471942));
#38137=CARTESIAN_POINT('Ctrl Pts',(0.181093814239817,-0.0319281812935353,
-0.065949757705594));
#38138=CARTESIAN_POINT('Ctrl Pts',(0.124962845363592,0.134900019854162,
-0.0548301119639941));
#38139=CARTESIAN_POINT('Ctrl Pts',(-0.045646197418241,0.178120393087247,
-0.0437104662223939));
#38140=CARTESIAN_POINT('Ctrl Pts',(-0.174457737366406,0.0581727877334231,
-0.0325908204807939));
#38141=CARTESIAN_POINT('Ctrl Pts',(-0.143387600717461,-0.115120065799724,
-0.0214711747391938));
#38142=CARTESIAN_POINT('Ctrl Pts',(0.0189688091733509,-0.182849550849372,
-0.0103515289975937));
#38143=CARTESIAN_POINT('Ctrl Pts',(0.164108705829999,-0.0832284895629474,
0.00076811674400635));
#38144=CARTESIAN_POINT('Ctrl Pts',(0.158572054537281,0.0929974829517444,
0.0118877624856064));
#38145=CARTESIAN_POINT('Ctrl Pts',(0.0584988683485304,0.153140084124104,
0.0193008596466731));
#38146=CARTESIAN_POINT('Ctrl Pts',(0.00679696520801413,0.155401427805413,
0.0230074082272065));
#38147=CARTESIAN_POINT('',(0.00853826423430722,0.195213365433479,0.));
#38148=CARTESIAN_POINT('Ctrl Pts',(0.133822070517493,-0.0798006560480865,
1.04083408558608E-17));
#38149=CARTESIAN_POINT('Ctrl Pts',(0.136054490212563,-0.0769648097335247,
3.49555778604013E-18));
#38150=CARTESIAN_POINT('Ctrl Pts',(0.13817734199536,-0.0740511128945859,
1.83743250757632E-16));
#38151=CARTESIAN_POINT('Ctrl Pts',(0.14018477846174,-0.0710636564573235,
1.94289029309402E-16));
#38152=CARTESIAN_POINT('Ctrl Pts',(0.145087642260683,-0.063767240225737,
2.23391728783535E-16));
#38153=CARTESIAN_POINT('Ctrl Pts',(0.149303339241034,-0.0560321219577389,
1.56818419132082E-16));
#38154=CARTESIAN_POINT('Ctrl Pts',(0.152847589720857,-0.0479613923182007,
1.2490009027033E-16));
#38155=CARTESIAN_POINT('Ctrl Pts',(0.15455977808461,-0.0440625117355556,
1.09480697205803E-16));
#38156=CARTESIAN_POINT('Ctrl Pts',(0.156114761257445,-0.0400845646834566,
-1.25648886706941E-16));
#38157=CARTESIAN_POINT('Ctrl Pts',(0.157508730347866,-0.0360533266198954,
-6.93889390390723E-17));
#38158=CARTESIAN_POINT('Ctrl Pts',(0.160055180865878,-0.0286892119306038,
3.3384625932115E-17));
#38159=CARTESIAN_POINT('Ctrl Pts',(0.162070216310737,-0.0211365082118436,
8.06994689406633E-17));
#38160=CARTESIAN_POINT('Ctrl Pts',(0.163561952707671,-0.0134617511743051,
6.93889390390723E-17));
#38161=CARTESIAN_POINT('Ctrl Pts',(0.164339267575536,-0.00946258432097103,
6.34952415506897E-17));
#38162=CARTESIAN_POINT('Ctrl Pts',(0.164974517612341,-0.00542855824006687,
1.57353126539468E-16));
#38163=CARTESIAN_POINT('Ctrl Pts',(0.165467142704647,-0.00137336699737669,
1.35308431126191E-16));
#38164=CARTESIAN_POINT('Ctrl Pts',(0.166873643263939,0.0102046643290036,
7.23683232988437E-17));
#38165=CARTESIAN_POINT('Ctrl Pts',(0.167113195337005,0.0218827002968643,
1.56622012929874E-16));
#38166=CARTESIAN_POINT('Ctrl Pts',(0.166211473778159,0.0334541513985393,
2.42861286636753E-16));
#38167=CARTESIAN_POINT('Ctrl Pts',(0.165524281373494,0.0422726311498785,
3.08583319445951E-16));
#38168=CARTESIAN_POINT('Ctrl Pts',(0.164173427571641,0.0510302884111691,
1.90686017996932E-16));
#38169=CARTESIAN_POINT('Ctrl Pts',(0.162151293669402,0.0596413236714313,
2.39391839684799E-16));
#38170=CARTESIAN_POINT('Ctrl Pts',(0.161342806590566,0.0630841771519127,
2.58865341145375E-16));
#38171=CARTESIAN_POINT('Ctrl Pts',(0.160426561788868,0.0665033606500684,
2.97312651021588E-16));
#38172=CARTESIAN_POINT('Ctrl Pts',(0.159406336715296,0.0698797924692321,
2.84494650060196E-16));
#38173=CARTESIAN_POINT('Ctrl Pts',(0.157424304970836,0.0764393205791983,
2.59592610829727E-16));
#38174=CARTESIAN_POINT('Ctrl Pts',(0.155047364014314,0.0828505294531396,
1.84123669457675E-18));
#38175=CARTESIAN_POINT('Ctrl Pts',(0.152277239552743,0.0890746728807261,
3.46944695195361E-18));
#38176=CARTESIAN_POINT('Ctrl Pts',(0.149146033051636,0.0961101251265181,
5.25576150690907E-18));
#38177=CARTESIAN_POINT('Ctrl Pts',(0.145512730626329,0.102906823780167,
-5.8747241662667E-17));
#38178=CARTESIAN_POINT('Ctrl Pts',(0.141425681028324,0.109443008062494,
-1.21430643318376E-16));
#38179=CARTESIAN_POINT('Ctrl Pts',(0.138942944415873,0.113413506495247,
-1.59508570329487E-16));
#38180=CARTESIAN_POINT('Ctrl Pts',(0.13629256386344,0.117287832803984,1.53692496207997E-16));
#38181=CARTESIAN_POINT('Ctrl Pts',(0.133483702160606,0.121060495400109,
1.6306400674182E-16));
#38182=CARTESIAN_POINT('Ctrl Pts',(0.131345168294252,0.123932821481525,
1.70199029671303E-16));
#38183=CARTESIAN_POINT('Ctrl Pts',(0.129114839715568,0.126745619606885,
5.90473990481052E-17));
#38184=CARTESIAN_POINT('Ctrl Pts',(0.126805988740716,0.129486179768006,
4.5102810375397E-17));
#38185=CARTESIAN_POINT('Ctrl Pts',(0.11940504484662,0.138270952891856,4.03901906608835E-19));
#38186=CARTESIAN_POINT('Ctrl Pts',(0.111179428463956,0.146343614865738,
2.51922702503768E-18));
#38187=CARTESIAN_POINT('Ctrl Pts',(0.102279336934698,0.153635544773705,
-1.4658413372004E-16));
#38188=CARTESIAN_POINT('Ctrl Pts',(0.0968240568380823,0.158105107807083,
-2.37976519240706E-16));
#38189=CARTESIAN_POINT('Ctrl Pts',(0.0911145357147371,0.162281120633163,
-2.06184360493938E-16));
#38190=CARTESIAN_POINT('Ctrl Pts',(0.0851790897705271,0.166143964756861,
-1.63931368479808E-16));
#38191=CARTESIAN_POINT('Ctrl Pts',(0.0807002479834999,0.169058837175987,
-1.32047586193085E-16));
#38192=CARTESIAN_POINT('Ctrl Pts',(0.0760870922293099,0.171797833033742,
-1.31664209440999E-18));
#38193=CARTESIAN_POINT('Ctrl Pts',(0.0713813828666237,0.174335786156758,
-3.46944695195361E-18));
#38194=CARTESIAN_POINT('Ctrl Pts',(0.060093655680461,0.180423650972855,
-8.63344499009989E-18));
#38195=CARTESIAN_POINT('Ctrl Pts',(0.0482526397033331,0.185375716453591,
2.38150771112053E-17));
#38196=CARTESIAN_POINT('Ctrl Pts',(0.0360316133450007,0.189089719698973,
2.86229373536173E-17));
#38197=CARTESIAN_POINT('Ctrl Pts',(0.0270536221211358,0.191818155721019,
3.21549587891586E-17));
#38198=CARTESIAN_POINT('Ctrl Pts',(0.0178694527935419,0.19387797767402,
2.08963768332319E-17));
#38199=CARTESIAN_POINT('Ctrl Pts',(0.00853826423430726,0.195213365433479,
-1.73472347597681E-18));
#38200=CARTESIAN_POINT('Ctrl Pts',(0.00853826423430726,0.195213365433479,
-1.73472347597681E-18));
#38201=CARTESIAN_POINT('Ctrl Pts',(0.0734855601112398,0.192372693268079,
-0.00370654858053334));
#38202=CARTESIAN_POINT('Ctrl Pts',(0.136340913956568,0.154597494717519,
-0.00741309716106669));
#38203=CARTESIAN_POINT('Ctrl Pts',(0.168927769774117,0.0988144116434918,
-0.0111196457416));
#38204=CARTESIAN_POINT('Ctrl Pts',(0.201514625591668,0.0430313285694631,
-0.0148261943221335));
#38205=CARTESIAN_POINT('Ctrl Pts',(0.203832983381438,-0.0307596390280334,
-0.0185327429026669));
#38206=CARTESIAN_POINT('Ctrl Pts',(0.174605002942014,-0.0885122484834479,
-0.0222392914832004));
#38207=CARTESIAN_POINT('Ctrl Pts',(0.145377022502591,-0.14626485793886,
-0.0259458400637337));
#38208=CARTESIAN_POINT('Ctrl Pts',(0.0846027038339767,-0.187979109252192,
-0.0296523886442669));
#38209=CARTESIAN_POINT('Ctrl Pts',(0.0202238564115267,-0.194656076997466,
-0.0333589372248002));
#38210=CARTESIAN_POINT('Ctrl Pts',(-0.0441549910109242,-0.201333044742741,
-0.0370654858053336));
#38211=CARTESIAN_POINT('Ctrl Pts',(-0.112138367187211,-0.172972728919958,
-0.0407720343858669));
#38212=CARTESIAN_POINT('Ctrl Pts',(-0.152635042633335,-0.122511178551289,
-0.0444785829664003));
#38213=CARTESIAN_POINT('Ctrl Pts',(-0.180074773643688,-0.0883194491505946,
-0.0469900655734589));
#38214=CARTESIAN_POINT('Ctrl Pts',(-0.194894963322837,-0.0439807237331546,
-0.0495015481805176));
#38215=CARTESIAN_POINT('Ctrl Pts',(-0.195233177397639,0.000155192514023357,
-0.0520130307875762));
#38216=CARTESIAN_POINT('Origin',(0.,0.,-0.56));
#38217=CARTESIAN_POINT('Origin',(0.,0.,0.));
#38218=CARTESIAN_POINT('Origin',(0.,0.,0.67));
#38219=CARTESIAN_POINT('',(0.,0.,0.64));
#38220=CARTESIAN_POINT('',(-0.2,-2.44929359829471E-17,0.7));
#38221=CARTESIAN_POINT('',(-0.1,-1.22464679914735E-17,0.67));
#38222=CARTESIAN_POINT('Origin',(0.,0.,0.7));
#38223=CARTESIAN_POINT('Origin',(0.545748091853324,-0.146232760482925,0.06));
#38224=CARTESIAN_POINT('',(0.574066611494015,-0.174492193429331,0.06));
#38225=CARTESIAN_POINT('',(0.574066611494015,-0.174492193429331,0.59));
#38226=CARTESIAN_POINT('',(0.574066611494015,-0.174492193429331,0.325));
#38227=CARTESIAN_POINT('',(0.545748091853324,-0.146232760482925,0.06));
#38228=CARTESIAN_POINT('',(0.545748091853324,-0.146232760482925,0.06));
#38229=CARTESIAN_POINT('',(0.545748091853324,-0.146232760482925,0.59));
#38230=CARTESIAN_POINT('',(0.545748091853324,-0.146232760482925,0.06));
#38231=CARTESIAN_POINT('',(0.545748091853324,-0.146232760482925,0.59));
#38232=CARTESIAN_POINT('Origin',(0.581970310339164,-0.155938474674269,0.59));
#38233=CARTESIAN_POINT('',(0.584402365732934,-0.13591863347514,0.59));
#38234=CARTESIAN_POINT('Origin',(0.,0.,0.59));
#38235=CARTESIAN_POINT('',(0.629372708972173,-0.123919188518606,0.59));
#38236=CARTESIAN_POINT('Origin',(0.629372708972173,-0.123919188518606,0.06));
#38237=CARTESIAN_POINT('',(0.584402365732934,-0.13591863347514,0.06));
#38238=CARTESIAN_POINT('',(0.584402365732934,-0.13591863347514,0.325));
#38239=CARTESIAN_POINT('',(0.629372708972173,-0.123919188518606,0.06));
#38240=CARTESIAN_POINT('Origin',(0.581970310339164,-0.155938474674269,0.06));
#38241=CARTESIAN_POINT('Origin',(0.,0.,0.06));
#38242=CARTESIAN_POINT('Origin',(0.489304353138208,-0.2825,0.06));
#38243=CARTESIAN_POINT('',(0.509343863171099,-0.317125888331339,0.06));
#38244=CARTESIAN_POINT('',(0.509343863171099,-0.317125888331339,0.59));
#38245=CARTESIAN_POINT('',(0.509343863171099,-0.317125888331339,0.325));
#38246=CARTESIAN_POINT('',(0.489304353138208,-0.2825,0.06));
#38247=CARTESIAN_POINT('',(0.489304353138208,-0.2825,0.06));
#38248=CARTESIAN_POINT('',(0.489304353138208,-0.2825,0.59));
#38249=CARTESIAN_POINT('',(0.489304353138208,-0.2825,0.06));
#38250=CARTESIAN_POINT('',(0.489304353138208,-0.2825,0.59));
#38251=CARTESIAN_POINT('Origin',(0.521780305780124,-0.30125,0.59));
#38252=CARTESIAN_POINT('',(0.529311007078196,-0.282541780602208,0.59));
#38253=CARTESIAN_POINT('Origin',(0.,0.,0.59));
#38254=CARTESIAN_POINT('',(0.57585470791547,-0.28259038811267,0.59));
#38255=CARTESIAN_POINT('Origin',(0.57585470791547,-0.28259038811267,0.06));
#38256=CARTESIAN_POINT('',(0.529311007078196,-0.282541780602208,0.06));
#38257=CARTESIAN_POINT('',(0.529311007078196,-0.282541780602208,0.325));
#38258=CARTESIAN_POINT('',(0.57585470791547,-0.28259038811267,0.06));
#38259=CARTESIAN_POINT('Origin',(0.521780305780124,-0.30125,0.06));
#38260=CARTESIAN_POINT('Origin',(0.,0.,0.06));
#38261=CARTESIAN_POINT('Origin',(0.399515331370399,-0.3995153313704,0.06));
#38262=CARTESIAN_POINT('',(0.409910172303604,-0.438147978018876,0.06));
#38263=CARTESIAN_POINT('',(0.409910172303604,-0.438147978018876,0.59));
#38264=CARTESIAN_POINT('',(0.409910172303604,-0.438147978018876,0.325));
#38265=CARTESIAN_POINT('',(0.399515331370399,-0.3995153313704,0.06));
#38266=CARTESIAN_POINT('',(0.399515331370399,-0.3995153313704,0.06));
#38267=CARTESIAN_POINT('',(0.399515331370399,-0.3995153313704,0.59));
#38268=CARTESIAN_POINT('',(0.399515331370399,-0.3995153313704,0.06));
#38269=CARTESIAN_POINT('',(0.399515331370399,-0.3995153313704,0.59));
#38270=CARTESIAN_POINT('Origin',(0.426031835664895,-0.426031835664895,0.59));
#38271=CARTESIAN_POINT('',(0.438147978018876,-0.409910172303604,0.59));
#38272=CARTESIAN_POINT('Origin',(0.,0.,0.59));
#38273=CARTESIAN_POINT('',(0.483093160159229,-0.422003519759552,0.59));
#38274=CARTESIAN_POINT('Origin',(0.483093160159229,-0.422003519759552,0.06));
#38275=CARTESIAN_POINT('',(0.438147978018876,-0.409910172303604,0.06));
#38276=CARTESIAN_POINT('',(0.438147978018876,-0.409910172303604,0.325));
#38277=CARTESIAN_POINT('',(0.483093160159229,-0.422003519759552,0.06));
#38278=CARTESIAN_POINT('Origin',(0.426031835664895,-0.426031835664895,0.06));
#38279=CARTESIAN_POINT('Origin',(0.,0.,0.06));
#38280=CARTESIAN_POINT('Origin',(0.2825,-0.489304353138208,0.06));
#38281=CARTESIAN_POINT('',(0.282541780602207,-0.529311007078196,0.06));
#38282=CARTESIAN_POINT('',(0.282541780602207,-0.529311007078196,0.59));
#38283=CARTESIAN_POINT('',(0.282541780602207,-0.529311007078196,0.325));
#38284=CARTESIAN_POINT('',(0.2825,-0.489304353138208,0.06));
#38285=CARTESIAN_POINT('',(0.2825,-0.489304353138208,0.06));
#38286=CARTESIAN_POINT('',(0.2825,-0.489304353138208,0.59));
#38287=CARTESIAN_POINT('',(0.2825,-0.489304353138208,0.06));
#38288=CARTESIAN_POINT('',(0.2825,-0.489304353138208,0.59));
#38289=CARTESIAN_POINT('Origin',(0.30125,-0.521780305780125,0.59));
#38290=CARTESIAN_POINT('',(0.317125888331339,-0.509343863171099,0.59));
#38291=CARTESIAN_POINT('Origin',(0.,0.,0.59));
#38292=CARTESIAN_POINT('',(0.35740961188733,-0.532657808928611,0.59));
#38293=CARTESIAN_POINT('Origin',(0.35740961188733,-0.532657808928611,0.06));
#38294=CARTESIAN_POINT('',(0.317125888331339,-0.509343863171099,0.06));
#38295=CARTESIAN_POINT('',(0.317125888331338,-0.509343863171099,0.325));
#38296=CARTESIAN_POINT('',(0.35740961188733,-0.532657808928611,0.06));
#38297=CARTESIAN_POINT('Origin',(0.30125,-0.521780305780125,0.06));
#38298=CARTESIAN_POINT('Origin',(0.,0.,0.06));
#38299=CARTESIAN_POINT('Origin',(0.146232760482924,-0.545748091853324,0.06));
#38300=CARTESIAN_POINT('',(0.135918633475139,-0.584402365732935,0.06));
#38301=CARTESIAN_POINT('',(0.135918633475139,-0.584402365732935,0.59));
#38302=CARTESIAN_POINT('',(0.135918633475139,-0.584402365732935,0.325));
#38303=CARTESIAN_POINT('',(0.146232760482924,-0.545748091853324,0.06));
#38304=CARTESIAN_POINT('',(0.146232760482924,-0.545748091853324,0.06));
#38305=CARTESIAN_POINT('',(0.146232760482924,-0.545748091853324,0.59));
#38306=CARTESIAN_POINT('',(0.146232760482924,-0.545748091853324,0.06));
#38307=CARTESIAN_POINT('',(0.146232760482924,-0.545748091853324,0.59));
#38308=CARTESIAN_POINT('Origin',(0.155938474674268,-0.581970310339164,0.59));
#38309=CARTESIAN_POINT('',(0.17449219342933,-0.574066611494016,0.59));
#38310=CARTESIAN_POINT('Origin',(0.,0.,0.59));
#38311=CARTESIAN_POINT('',(0.207369189212621,-0.607012348677835,0.59));
#38312=CARTESIAN_POINT('Origin',(0.207369189212621,-0.607012348677835,0.06));
#38313=CARTESIAN_POINT('',(0.17449219342933,-0.574066611494016,0.06));
#38314=CARTESIAN_POINT('',(0.17449219342933,-0.574066611494016,0.325));
#38315=CARTESIAN_POINT('',(0.207369189212621,-0.607012348677835,0.06));
#38316=CARTESIAN_POINT('Origin',(0.155938474674268,-0.581970310339164,0.06));
#38317=CARTESIAN_POINT('Origin',(0.,0.,0.06));
#38318=CARTESIAN_POINT('Origin',(-1.11022302462516E-16,-0.565,0.06));
#38319=CARTESIAN_POINT('',(-0.0199671439070973,-0.599667668933546,0.06));
#38320=CARTESIAN_POINT('',(-0.0199671439070973,-0.599667668933546,0.59));
#38321=CARTESIAN_POINT('',(-0.0199671439070973,-0.599667668933546,0.325));
#38322=CARTESIAN_POINT('',(-1.11022302462516E-16,-0.565,0.06));
#38323=CARTESIAN_POINT('',(-1.11022302462516E-16,-0.565,0.06));
#38324=CARTESIAN_POINT('',(-1.11022302462516E-16,-0.565,0.59));
#38325=CARTESIAN_POINT('',(-1.11022302462516E-16,-0.565,0.06));
#38326=CARTESIAN_POINT('',(-1.11022302462516E-16,-0.565,0.59));
#38327=CARTESIAN_POINT('Origin',(-8.32667268468867E-17,-0.6025,0.59));
#38328=CARTESIAN_POINT('',(0.0199671439070971,-0.599667668933546,0.59));
#38329=CARTESIAN_POINT('Origin',(0.,0.,0.59));
#38330=CARTESIAN_POINT('',(0.0431968989868596,-0.64,0.59));
#38331=CARTESIAN_POINT('Origin',(0.0431968989868596,-0.64,0.06));
#38332=CARTESIAN_POINT('',(0.0199671439070971,-0.599667668933546,0.06));
#38333=CARTESIAN_POINT('',(0.019967143907097,-0.599667668933546,0.325));
#38334=CARTESIAN_POINT('',(0.0431968989868596,-0.64,0.06));
#38335=CARTESIAN_POINT('Origin',(-8.32667268468867E-17,-0.6025,0.06));
#38336=CARTESIAN_POINT('Origin',(0.,0.,0.06));
#38337=CARTESIAN_POINT('Origin',(-0.146232760482925,-0.545748091853324,
0.06));
#38338=CARTESIAN_POINT('',(-0.174492193429331,-0.574066611494015,0.06));
#38339=CARTESIAN_POINT('',(-0.174492193429331,-0.574066611494015,0.59));
#38340=CARTESIAN_POINT('',(-0.174492193429331,-0.574066611494015,0.325));
#38341=CARTESIAN_POINT('',(-0.146232760482925,-0.545748091853324,0.06));
#38342=CARTESIAN_POINT('',(-0.146232760482925,-0.545748091853324,0.06));
#38343=CARTESIAN_POINT('',(-0.146232760482925,-0.545748091853324,0.59));
#38344=CARTESIAN_POINT('',(-0.146232760482925,-0.545748091853324,0.06));
#38345=CARTESIAN_POINT('',(-0.146232760482925,-0.545748091853324,0.59));
#38346=CARTESIAN_POINT('Origin',(-0.155938474674269,-0.581970310339164,
0.59));
#38347=CARTESIAN_POINT('',(-0.13591863347514,-0.584402365732934,0.59));
#38348=CARTESIAN_POINT('Origin',(0.,0.,0.59));
#38349=CARTESIAN_POINT('',(-0.123919188518606,-0.629372708972173,0.59));
#38350=CARTESIAN_POINT('Origin',(-0.123919188518606,-0.629372708972173,
0.06));
#38351=CARTESIAN_POINT('',(-0.13591863347514,-0.584402365732934,0.06));
#38352=CARTESIAN_POINT('',(-0.13591863347514,-0.584402365732934,0.325));
#38353=CARTESIAN_POINT('',(-0.123919188518606,-0.629372708972173,0.06));
#38354=CARTESIAN_POINT('Origin',(-0.155938474674269,-0.581970310339164,
0.06));
#38355=CARTESIAN_POINT('Origin',(0.,0.,0.06));
#38356=CARTESIAN_POINT('Origin',(-0.2825,-0.489304353138208,0.06));
#38357=CARTESIAN_POINT('',(-0.317125888331339,-0.509343863171099,0.06));
#38358=CARTESIAN_POINT('',(-0.317125888331339,-0.509343863171099,0.59));
#38359=CARTESIAN_POINT('',(-0.317125888331339,-0.509343863171099,0.325));
#38360=CARTESIAN_POINT('',(-0.2825,-0.489304353138208,0.06));
#38361=CARTESIAN_POINT('',(-0.2825,-0.489304353138208,0.06));
#38362=CARTESIAN_POINT('',(-0.2825,-0.489304353138208,0.59));
#38363=CARTESIAN_POINT('',(-0.2825,-0.489304353138208,0.06));
#38364=CARTESIAN_POINT('',(-0.2825,-0.489304353138208,0.59));
#38365=CARTESIAN_POINT('Origin',(-0.30125,-0.521780305780124,0.59));
#38366=CARTESIAN_POINT('',(-0.282541780602208,-0.529311007078196,0.59));
#38367=CARTESIAN_POINT('Origin',(0.,0.,0.59));
#38368=CARTESIAN_POINT('',(-0.28259038811267,-0.57585470791547,0.59));
#38369=CARTESIAN_POINT('Origin',(-0.28259038811267,-0.57585470791547,0.06));
#38370=CARTESIAN_POINT('',(-0.282541780602208,-0.529311007078196,0.06));
#38371=CARTESIAN_POINT('',(-0.282541780602208,-0.529311007078196,0.325));
#38372=CARTESIAN_POINT('',(-0.28259038811267,-0.57585470791547,0.06));
#38373=CARTESIAN_POINT('Origin',(-0.30125,-0.521780305780124,0.06));
#38374=CARTESIAN_POINT('Origin',(0.,0.,0.06));
#38375=CARTESIAN_POINT('Origin',(-0.3995153313704,-0.399515331370399,0.06));
#38376=CARTESIAN_POINT('',(-0.438147978018877,-0.409910172303604,0.06));
#38377=CARTESIAN_POINT('',(-0.438147978018877,-0.409910172303604,0.59));
#38378=CARTESIAN_POINT('',(-0.438147978018876,-0.409910172303604,0.325));
#38379=CARTESIAN_POINT('',(-0.3995153313704,-0.399515331370399,0.06));
#38380=CARTESIAN_POINT('',(-0.3995153313704,-0.399515331370399,0.06));
#38381=CARTESIAN_POINT('',(-0.3995153313704,-0.399515331370399,0.59));
#38382=CARTESIAN_POINT('',(-0.3995153313704,-0.399515331370399,0.06));
#38383=CARTESIAN_POINT('',(-0.3995153313704,-0.399515331370399,0.59));
#38384=CARTESIAN_POINT('Origin',(-0.426031835664895,-0.426031835664895,
0.59));
#38385=CARTESIAN_POINT('',(-0.409910172303604,-0.438147978018876,0.59));
#38386=CARTESIAN_POINT('Origin',(0.,0.,0.59));
#38387=CARTESIAN_POINT('',(-0.422003519759552,-0.483093160159229,0.59));
#38388=CARTESIAN_POINT('Origin',(-0.422003519759552,-0.483093160159229,
0.06));
#38389=CARTESIAN_POINT('',(-0.409910172303604,-0.438147978018876,0.06));
#38390=CARTESIAN_POINT('',(-0.409910172303604,-0.438147978018876,0.325));
#38391=CARTESIAN_POINT('',(-0.422003519759552,-0.483093160159229,0.06));
#38392=CARTESIAN_POINT('Origin',(-0.426031835664895,-0.426031835664895,
0.06));
#38393=CARTESIAN_POINT('Origin',(0.,0.,0.06));
#38394=CARTESIAN_POINT('Origin',(-0.489304353138208,-0.2825,0.06));
#38395=CARTESIAN_POINT('',(-0.529311007078196,-0.282541780602207,0.06));
#38396=CARTESIAN_POINT('',(-0.529311007078196,-0.282541780602207,0.59));
#38397=CARTESIAN_POINT('',(-0.529311007078196,-0.282541780602207,0.325));
#38398=CARTESIAN_POINT('',(-0.489304353138208,-0.2825,0.06));
#38399=CARTESIAN_POINT('',(-0.489304353138208,-0.2825,0.06));
#38400=CARTESIAN_POINT('',(-0.489304353138208,-0.2825,0.59));
#38401=CARTESIAN_POINT('',(-0.489304353138208,-0.2825,0.06));
#38402=CARTESIAN_POINT('',(-0.489304353138208,-0.2825,0.59));
#38403=CARTESIAN_POINT('Origin',(-0.521780305780124,-0.30125,0.59));
#38404=CARTESIAN_POINT('',(-0.509343863171099,-0.317125888331339,0.59));
#38405=CARTESIAN_POINT('Origin',(0.,0.,0.59));
#38406=CARTESIAN_POINT('',(-0.532657808928611,-0.357409611887331,0.59));
#38407=CARTESIAN_POINT('Origin',(-0.532657808928611,-0.357409611887331,
0.06));
#38408=CARTESIAN_POINT('',(-0.509343863171099,-0.317125888331339,0.06));
#38409=CARTESIAN_POINT('',(-0.509343863171099,-0.317125888331339,0.325));
#38410=CARTESIAN_POINT('',(-0.532657808928611,-0.357409611887331,0.06));
#38411=CARTESIAN_POINT('Origin',(-0.521780305780124,-0.30125,0.06));
#38412=CARTESIAN_POINT('Origin',(0.,0.,0.06));
#38413=CARTESIAN_POINT('Origin',(-0.545748091853324,-0.146232760482924,
0.06));
#38414=CARTESIAN_POINT('',(-0.584402365732935,-0.135918633475139,0.06));
#38415=CARTESIAN_POINT('',(-0.584402365732935,-0.135918633475139,0.59));
#38416=CARTESIAN_POINT('',(-0.584402365732935,-0.135918633475139,0.325));
#38417=CARTESIAN_POINT('',(-0.545748091853324,-0.146232760482924,0.06));
#38418=CARTESIAN_POINT('',(-0.545748091853324,-0.146232760482924,0.06));
#38419=CARTESIAN_POINT('',(-0.545748091853324,-0.146232760482924,0.59));
#38420=CARTESIAN_POINT('',(-0.545748091853324,-0.146232760482924,0.06));
#38421=CARTESIAN_POINT('',(-0.545748091853324,-0.146232760482924,0.59));
#38422=CARTESIAN_POINT('Origin',(-0.581970310339164,-0.155938474674269,
0.59));
#38423=CARTESIAN_POINT('',(-0.574066611494016,-0.17449219342933,0.59));
#38424=CARTESIAN_POINT('Origin',(0.,0.,0.59));
#38425=CARTESIAN_POINT('',(-0.607012348677835,-0.207369189212621,0.59));
#38426=CARTESIAN_POINT('Origin',(-0.607012348677835,-0.207369189212621,
0.06));
#38427=CARTESIAN_POINT('',(-0.574066611494016,-0.17449219342933,0.06));
#38428=CARTESIAN_POINT('',(-0.574066611494016,-0.17449219342933,0.325));
#38429=CARTESIAN_POINT('',(-0.607012348677835,-0.207369189212621,0.06));
#38430=CARTESIAN_POINT('Origin',(-0.581970310339164,-0.155938474674269,
0.06));
#38431=CARTESIAN_POINT('Origin',(0.,0.,0.06));
#38432=CARTESIAN_POINT('Origin',(-0.565,8.32667268468867E-17,0.06));
#38433=CARTESIAN_POINT('',(-0.599667668933546,0.0199671439070973,0.06));
#38434=CARTESIAN_POINT('',(-0.599667668933546,0.0199671439070973,0.59));
#38435=CARTESIAN_POINT('',(-0.599667668933546,0.0199671439070973,0.325));
#38436=CARTESIAN_POINT('',(-0.565,8.32667268468867E-17,0.06));
#38437=CARTESIAN_POINT('',(-0.565,8.32667268468867E-17,0.06));
#38438=CARTESIAN_POINT('',(-0.565,8.32667268468867E-17,0.59));
#38439=CARTESIAN_POINT('',(-0.565,8.32667268468867E-17,0.06));
#38440=CARTESIAN_POINT('',(-0.565,8.32667268468867E-17,0.59));
#38441=CARTESIAN_POINT('Origin',(-0.6025,5.55111512312578E-17,0.59));
#38442=CARTESIAN_POINT('',(-0.6,-7.34788079488412E-17,0.59));
#38443=CARTESIAN_POINT('Origin',(0.,0.,0.59));
#38444=CARTESIAN_POINT('',(-0.599667668933546,-0.0199671439070971,0.59));
#38445=CARTESIAN_POINT('',(-0.64,-0.0431968989868596,0.59));
#38446=CARTESIAN_POINT('Origin',(0.,0.,0.59));
#38447=CARTESIAN_POINT('Origin',(-0.64,-0.0431968989868596,0.06));
#38448=CARTESIAN_POINT('',(-0.599667668933546,-0.0199671439070971,0.06));
#38449=CARTESIAN_POINT('',(-0.599667668933546,-0.019967143907097,0.325));
#38450=CARTESIAN_POINT('',(-0.64,-0.0431968989868596,0.06));
#38451=CARTESIAN_POINT('Origin',(-0.6025,5.55111512312578E-17,0.06));
#38452=CARTESIAN_POINT('',(-0.6,-7.34788079488412E-17,0.06));
#38453=CARTESIAN_POINT('Origin',(0.,0.,0.06));
#38454=CARTESIAN_POINT('Origin',(0.,0.,0.06));
#38455=CARTESIAN_POINT('Origin',(-0.545748091853324,0.146232760482924,0.06));
#38456=CARTESIAN_POINT('',(-0.574066611494016,0.174492193429331,0.06));
#38457=CARTESIAN_POINT('',(-0.574066611494016,0.174492193429331,0.59));
#38458=CARTESIAN_POINT('',(-0.574066611494016,0.174492193429331,0.325));
#38459=CARTESIAN_POINT('',(-0.545748091853324,0.146232760482924,0.06));
#38460=CARTESIAN_POINT('',(-0.545748091853324,0.146232760482924,0.06));
#38461=CARTESIAN_POINT('',(-0.545748091853324,0.146232760482924,0.59));
#38462=CARTESIAN_POINT('',(-0.545748091853324,0.146232760482924,0.06));
#38463=CARTESIAN_POINT('',(-0.545748091853324,0.146232760482924,0.59));
#38464=CARTESIAN_POINT('Origin',(-0.581970310339164,0.155938474674269,0.59));
#38465=CARTESIAN_POINT('',(-0.584402365732935,0.13591863347514,0.59));
#38466=CARTESIAN_POINT('Origin',(0.,0.,0.59));
#38467=CARTESIAN_POINT('',(-0.629372708972173,0.123919188518606,0.59));
#38468=CARTESIAN_POINT('Origin',(-0.629372708972173,0.123919188518606,0.06));
#38469=CARTESIAN_POINT('',(-0.584402365732935,0.13591863347514,0.06));
#38470=CARTESIAN_POINT('',(-0.584402365732934,0.13591863347514,0.325));
#38471=CARTESIAN_POINT('',(-0.629372708972173,0.123919188518606,0.06));
#38472=CARTESIAN_POINT('Origin',(-0.581970310339164,0.155938474674269,0.06));
#38473=CARTESIAN_POINT('Origin',(0.,0.,0.06));
#38474=CARTESIAN_POINT('Origin',(-0.489304353138208,0.2825,0.06));
#38475=CARTESIAN_POINT('',(-0.509343863171099,0.317125888331339,0.06));
#38476=CARTESIAN_POINT('',(-0.509343863171099,0.317125888331339,0.59));
#38477=CARTESIAN_POINT('',(-0.509343863171099,0.317125888331339,0.325));
#38478=CARTESIAN_POINT('',(-0.489304353138208,0.2825,0.06));
#38479=CARTESIAN_POINT('',(-0.489304353138208,0.2825,0.06));
#38480=CARTESIAN_POINT('',(-0.489304353138208,0.2825,0.59));
#38481=CARTESIAN_POINT('',(-0.489304353138208,0.2825,0.06));
#38482=CARTESIAN_POINT('',(-0.489304353138208,0.2825,0.59));
#38483=CARTESIAN_POINT('Origin',(-0.521780305780124,0.30125,0.59));
#38484=CARTESIAN_POINT('',(-0.529311007078196,0.282541780602208,0.59));
#38485=CARTESIAN_POINT('Origin',(0.,0.,0.59));
#38486=CARTESIAN_POINT('',(-0.57585470791547,0.28259038811267,0.59));
#38487=CARTESIAN_POINT('Origin',(-0.57585470791547,0.28259038811267,0.06));
#38488=CARTESIAN_POINT('',(-0.529311007078196,0.282541780602208,0.06));
#38489=CARTESIAN_POINT('',(-0.529311007078196,0.282541780602208,0.325));
#38490=CARTESIAN_POINT('',(-0.57585470791547,0.28259038811267,0.06));
#38491=CARTESIAN_POINT('Origin',(-0.521780305780124,0.30125,0.06));
#38492=CARTESIAN_POINT('Origin',(0.,0.,0.06));
#38493=CARTESIAN_POINT('Origin',(-0.399515331370399,0.399515331370399,0.06));
#38494=CARTESIAN_POINT('',(-0.409910172303604,0.438147978018876,0.06));
#38495=CARTESIAN_POINT('',(-0.409910172303604,0.438147978018876,0.59));
#38496=CARTESIAN_POINT('',(-0.409910172303604,0.438147978018876,0.325));
#38497=CARTESIAN_POINT('',(-0.399515331370399,0.399515331370399,0.06));
#38498=CARTESIAN_POINT('',(-0.399515331370399,0.399515331370399,0.06));
#38499=CARTESIAN_POINT('',(-0.399515331370399,0.399515331370399,0.59));
#38500=CARTESIAN_POINT('',(-0.399515331370399,0.399515331370399,0.06));
#38501=CARTESIAN_POINT('',(-0.399515331370399,0.399515331370399,0.59));
#38502=CARTESIAN_POINT('Origin',(-0.426031835664895,0.426031835664895,0.59));
#38503=CARTESIAN_POINT('',(-0.438147978018876,0.409910172303604,0.59));
#38504=CARTESIAN_POINT('Origin',(0.,0.,0.59));
#38505=CARTESIAN_POINT('',(-0.483093160159229,0.422003519759552,0.59));
#38506=CARTESIAN_POINT('Origin',(-0.483093160159229,0.422003519759552,0.06));
#38507=CARTESIAN_POINT('',(-0.438147978018876,0.409910172303604,0.06));
#38508=CARTESIAN_POINT('',(-0.438147978018876,0.409910172303604,0.325));
#38509=CARTESIAN_POINT('',(-0.483093160159229,0.422003519759552,0.06));
#38510=CARTESIAN_POINT('Origin',(-0.426031835664895,0.426031835664895,0.06));
#38511=CARTESIAN_POINT('Origin',(0.,0.,0.06));
#38512=CARTESIAN_POINT('Origin',(-0.2825,0.489304353138208,0.06));
#38513=CARTESIAN_POINT('',(-0.282541780602207,0.529311007078196,0.06));
#38514=CARTESIAN_POINT('',(-0.282541780602207,0.529311007078196,0.59));
#38515=CARTESIAN_POINT('',(-0.282541780602207,0.529311007078196,0.325));
#38516=CARTESIAN_POINT('',(-0.2825,0.489304353138208,0.06));
#38517=CARTESIAN_POINT('',(-0.2825,0.489304353138208,0.06));
#38518=CARTESIAN_POINT('',(-0.2825,0.489304353138208,0.59));
#38519=CARTESIAN_POINT('',(-0.2825,0.489304353138208,0.06));
#38520=CARTESIAN_POINT('',(-0.2825,0.489304353138208,0.59));
#38521=CARTESIAN_POINT('Origin',(-0.30125,0.521780305780125,0.59));
#38522=CARTESIAN_POINT('',(-0.317125888331339,0.509343863171099,0.59));
#38523=CARTESIAN_POINT('Origin',(0.,0.,0.59));
#38524=CARTESIAN_POINT('',(-0.357409611887331,0.532657808928611,0.59));
#38525=CARTESIAN_POINT('Origin',(-0.357409611887331,0.532657808928611,0.06));
#38526=CARTESIAN_POINT('',(-0.317125888331339,0.509343863171099,0.06));
#38527=CARTESIAN_POINT('',(-0.317125888331339,0.509343863171099,0.325));
#38528=CARTESIAN_POINT('',(-0.357409611887331,0.532657808928611,0.06));
#38529=CARTESIAN_POINT('Origin',(-0.30125,0.521780305780125,0.06));
#38530=CARTESIAN_POINT('Origin',(0.,0.,0.06));
#38531=CARTESIAN_POINT('Origin',(-0.146232760482924,0.545748091853324,0.06));
#38532=CARTESIAN_POINT('',(-0.135918633475139,0.584402365732935,0.06));
#38533=CARTESIAN_POINT('',(-0.135918633475139,0.584402365732935,0.59));
#38534=CARTESIAN_POINT('',(-0.135918633475139,0.584402365732935,0.325));
#38535=CARTESIAN_POINT('',(-0.146232760482924,0.545748091853324,0.06));
#38536=CARTESIAN_POINT('',(-0.146232760482924,0.545748091853324,0.06));
#38537=CARTESIAN_POINT('',(-0.146232760482924,0.545748091853324,0.59));
#38538=CARTESIAN_POINT('',(-0.146232760482924,0.545748091853324,0.06));
#38539=CARTESIAN_POINT('',(-0.146232760482924,0.545748091853324,0.59));
#38540=CARTESIAN_POINT('Origin',(-0.155938474674269,0.581970310339164,0.59));
#38541=CARTESIAN_POINT('',(-0.17449219342933,0.574066611494016,0.59));
#38542=CARTESIAN_POINT('Origin',(0.,0.,0.59));
#38543=CARTESIAN_POINT('',(-0.207369189212621,0.607012348677835,0.59));
#38544=CARTESIAN_POINT('Origin',(-0.207369189212621,0.607012348677835,0.06));
#38545=CARTESIAN_POINT('',(-0.17449219342933,0.574066611494016,0.06));
#38546=CARTESIAN_POINT('',(-0.17449219342933,0.574066611494016,0.325));
#38547=CARTESIAN_POINT('',(-0.207369189212621,0.607012348677835,0.06));
#38548=CARTESIAN_POINT('Origin',(-0.155938474674269,0.581970310339164,0.06));
#38549=CARTESIAN_POINT('Origin',(0.,0.,0.06));
#38550=CARTESIAN_POINT('Origin',(5.55111512312578E-17,0.565,0.06));
#38551=CARTESIAN_POINT('',(0.0199671439070973,0.599667668933546,0.06));
#38552=CARTESIAN_POINT('',(0.0199671439070973,0.599667668933546,0.59));
#38553=CARTESIAN_POINT('',(0.0199671439070972,0.599667668933546,0.325));
#38554=CARTESIAN_POINT('',(5.55111512312578E-17,0.565,0.06));
#38555=CARTESIAN_POINT('',(5.55111512312578E-17,0.565,0.06));
#38556=CARTESIAN_POINT('',(5.55111512312578E-17,0.565,0.59));
#38557=CARTESIAN_POINT('',(5.55111512312578E-17,0.565,0.06));
#38558=CARTESIAN_POINT('',(5.55111512312578E-17,0.565,0.59));
#38559=CARTESIAN_POINT('Origin',(2.77555756156289E-17,0.6025,0.59));
#38560=CARTESIAN_POINT('',(-0.0199671439070972,0.599667668933546,0.59));
#38561=CARTESIAN_POINT('Origin',(0.,0.,0.59));
#38562=CARTESIAN_POINT('',(-0.0431968989868596,0.64,0.59));
#38563=CARTESIAN_POINT('Origin',(-0.0431968989868596,0.64,0.06));
#38564=CARTESIAN_POINT('',(-0.0199671439070972,0.599667668933546,0.06));
#38565=CARTESIAN_POINT('',(-0.0199671439070972,0.599667668933546,0.325));
#38566=CARTESIAN_POINT('',(-0.0431968989868596,0.64,0.06));
#38567=CARTESIAN_POINT('Origin',(2.77555756156289E-17,0.6025,0.06));
#38568=CARTESIAN_POINT('Origin',(0.,0.,0.06));
#38569=CARTESIAN_POINT('Origin',(0.146232760482924,0.545748091853324,0.06));
#38570=CARTESIAN_POINT('',(0.174492193429331,0.574066611494016,0.06));
#38571=CARTESIAN_POINT('',(0.174492193429331,0.574066611494016,0.59));
#38572=CARTESIAN_POINT('',(0.174492193429331,0.574066611494016,0.325));
#38573=CARTESIAN_POINT('',(0.146232760482924,0.545748091853324,0.06));
#38574=CARTESIAN_POINT('',(0.146232760482924,0.545748091853324,0.06));
#38575=CARTESIAN_POINT('',(0.146232760482924,0.545748091853324,0.59));
#38576=CARTESIAN_POINT('',(0.146232760482924,0.545748091853324,0.06));
#38577=CARTESIAN_POINT('',(0.146232760482924,0.545748091853324,0.59));
#38578=CARTESIAN_POINT('Origin',(0.155938474674269,0.581970310339164,0.59));
#38579=CARTESIAN_POINT('',(0.13591863347514,0.584402365732935,0.59));
#38580=CARTESIAN_POINT('Origin',(0.,0.,0.59));
#38581=CARTESIAN_POINT('',(0.123919188518606,0.629372708972173,0.59));
#38582=CARTESIAN_POINT('Origin',(0.123919188518606,0.629372708972173,0.06));
#38583=CARTESIAN_POINT('',(0.13591863347514,0.584402365732935,0.06));
#38584=CARTESIAN_POINT('',(0.13591863347514,0.584402365732934,0.325));
#38585=CARTESIAN_POINT('',(0.123919188518606,0.629372708972173,0.06));
#38586=CARTESIAN_POINT('Origin',(0.155938474674269,0.581970310339164,0.06));
#38587=CARTESIAN_POINT('Origin',(0.,0.,0.06));
#38588=CARTESIAN_POINT('Origin',(0.2825,0.489304353138208,0.06));
#38589=CARTESIAN_POINT('',(0.317125888331339,0.509343863171099,0.06));
#38590=CARTESIAN_POINT('',(0.317125888331339,0.509343863171099,0.59));
#38591=CARTESIAN_POINT('',(0.317125888331339,0.509343863171099,0.325));
#38592=CARTESIAN_POINT('',(0.2825,0.489304353138208,0.06));
#38593=CARTESIAN_POINT('',(0.2825,0.489304353138208,0.06));
#38594=CARTESIAN_POINT('',(0.2825,0.489304353138208,0.59));
#38595=CARTESIAN_POINT('',(0.2825,0.489304353138208,0.06));
#38596=CARTESIAN_POINT('',(0.2825,0.489304353138208,0.59));
#38597=CARTESIAN_POINT('Origin',(0.30125,0.521780305780124,0.59));
#38598=CARTESIAN_POINT('',(0.282541780602207,0.529311007078196,0.59));
#38599=CARTESIAN_POINT('Origin',(0.,0.,0.59));
#38600=CARTESIAN_POINT('',(0.282590388112669,0.575854707915471,0.59));
#38601=CARTESIAN_POINT('Origin',(0.282590388112669,0.575854707915471,0.06));
#38602=CARTESIAN_POINT('',(0.282541780602207,0.529311007078196,0.06));
#38603=CARTESIAN_POINT('',(0.282541780602207,0.529311007078196,0.325));
#38604=CARTESIAN_POINT('',(0.282590388112669,0.575854707915471,0.06));
#38605=CARTESIAN_POINT('Origin',(0.30125,0.521780305780124,0.06));
#38606=CARTESIAN_POINT('Origin',(0.,0.,0.06));
#38607=CARTESIAN_POINT('Origin',(0.399515331370399,0.399515331370399,0.06));
#38608=CARTESIAN_POINT('',(0.438147978018876,0.409910172303604,0.06));
#38609=CARTESIAN_POINT('',(0.438147978018876,0.409910172303604,0.59));
#38610=CARTESIAN_POINT('',(0.438147978018876,0.409910172303604,0.325));
#38611=CARTESIAN_POINT('',(0.399515331370399,0.399515331370399,0.06));
#38612=CARTESIAN_POINT('',(0.399515331370399,0.399515331370399,0.06));
#38613=CARTESIAN_POINT('',(0.399515331370399,0.399515331370399,0.59));
#38614=CARTESIAN_POINT('',(0.399515331370399,0.399515331370399,0.06));
#38615=CARTESIAN_POINT('',(0.399515331370399,0.399515331370399,0.59));
#38616=CARTESIAN_POINT('Origin',(0.426031835664895,0.426031835664895,0.59));
#38617=CARTESIAN_POINT('',(0.409910172303604,0.438147978018876,0.59));
#38618=CARTESIAN_POINT('Origin',(0.,0.,0.59));
#38619=CARTESIAN_POINT('',(0.422003519759552,0.483093160159229,0.59));
#38620=CARTESIAN_POINT('Origin',(0.422003519759552,0.483093160159229,0.06));
#38621=CARTESIAN_POINT('',(0.409910172303604,0.438147978018876,0.06));
#38622=CARTESIAN_POINT('',(0.409910172303604,0.438147978018876,0.325));
#38623=CARTESIAN_POINT('',(0.422003519759552,0.483093160159229,0.06));
#38624=CARTESIAN_POINT('Origin',(0.426031835664895,0.426031835664895,0.06));
#38625=CARTESIAN_POINT('Origin',(0.,0.,0.06));
#38626=CARTESIAN_POINT('Origin',(0.489304353138208,0.2825,0.06));
#38627=CARTESIAN_POINT('',(0.529311007078196,0.282541780602207,0.06));
#38628=CARTESIAN_POINT('',(0.529311007078196,0.282541780602207,0.59));
#38629=CARTESIAN_POINT('',(0.529311007078196,0.282541780602207,0.325));
#38630=CARTESIAN_POINT('',(0.489304353138208,0.2825,0.06));
#38631=CARTESIAN_POINT('',(0.489304353138208,0.2825,0.06));
#38632=CARTESIAN_POINT('',(0.489304353138208,0.2825,0.59));
#38633=CARTESIAN_POINT('',(0.489304353138208,0.2825,0.06));
#38634=CARTESIAN_POINT('',(0.489304353138208,0.2825,0.59));
#38635=CARTESIAN_POINT('Origin',(0.521780305780124,0.30125,0.59));
#38636=CARTESIAN_POINT('',(0.509343863171099,0.317125888331339,0.59));
#38637=CARTESIAN_POINT('Origin',(0.,0.,0.59));
#38638=CARTESIAN_POINT('',(0.532657808928611,0.357409611887331,0.59));
#38639=CARTESIAN_POINT('Origin',(0.532657808928611,0.357409611887331,0.06));
#38640=CARTESIAN_POINT('',(0.509343863171099,0.317125888331339,0.06));
#38641=CARTESIAN_POINT('',(0.509343863171099,0.317125888331339,0.325));
#38642=CARTESIAN_POINT('',(0.532657808928611,0.357409611887331,0.06));
#38643=CARTESIAN_POINT('Origin',(0.521780305780124,0.30125,0.06));
#38644=CARTESIAN_POINT('Origin',(0.,0.,0.06));
#38645=CARTESIAN_POINT('Origin',(0.545748091853324,0.146232760482924,0.06));
#38646=CARTESIAN_POINT('',(0.584402365732935,0.135918633475139,0.06));
#38647=CARTESIAN_POINT('',(0.584402365732935,0.135918633475139,0.59));
#38648=CARTESIAN_POINT('',(0.584402365732935,0.135918633475139,0.325));
#38649=CARTESIAN_POINT('',(0.545748091853324,0.146232760482924,0.06));
#38650=CARTESIAN_POINT('',(0.545748091853324,0.146232760482924,0.06));
#38651=CARTESIAN_POINT('',(0.545748091853324,0.146232760482924,0.59));
#38652=CARTESIAN_POINT('',(0.545748091853324,0.146232760482924,0.06));
#38653=CARTESIAN_POINT('',(0.545748091853324,0.146232760482924,0.59));
#38654=CARTESIAN_POINT('Origin',(0.581970310339164,0.155938474674269,0.59));
#38655=CARTESIAN_POINT('',(0.574066611494016,0.17449219342933,0.59));
#38656=CARTESIAN_POINT('Origin',(0.,0.,0.59));
#38657=CARTESIAN_POINT('',(0.607012348677835,0.207369189212621,0.59));
#38658=CARTESIAN_POINT('Origin',(0.607012348677835,0.207369189212621,0.06));
#38659=CARTESIAN_POINT('',(0.574066611494016,0.17449219342933,0.06));
#38660=CARTESIAN_POINT('',(0.574066611494016,0.174492193429331,0.325));
#38661=CARTESIAN_POINT('',(0.607012348677835,0.207369189212621,0.06));
#38662=CARTESIAN_POINT('Origin',(0.581970310339164,0.155938474674269,0.06));
#38663=CARTESIAN_POINT('Origin',(0.,0.,0.06));
#38664=CARTESIAN_POINT('Origin',(0.565,0.,0.06));
#38665=CARTESIAN_POINT('',(0.599667668933546,-0.0199671439070972,0.06));
#38666=CARTESIAN_POINT('',(0.599667668933546,-0.0199671439070972,0.59));
#38667=CARTESIAN_POINT('',(0.599667668933546,-0.0199671439070972,0.325));
#38668=CARTESIAN_POINT('',(0.565,0.,0.06));
#38669=CARTESIAN_POINT('',(0.565,0.,0.06));
#38670=CARTESIAN_POINT('',(0.565,0.,0.59));
#38671=CARTESIAN_POINT('',(0.565,0.,0.06));
#38672=CARTESIAN_POINT('',(0.565,0.,0.59));
#38673=CARTESIAN_POINT('Origin',(0.6025,0.,0.59));
#38674=CARTESIAN_POINT('',(0.599667668933546,0.0199671439070972,0.59));
#38675=CARTESIAN_POINT('Origin',(0.,0.,0.59));
#38676=CARTESIAN_POINT('',(0.64,0.0431968989868597,0.59));
#38677=CARTESIAN_POINT('Origin',(0.64,0.0431968989868597,0.06));
#38678=CARTESIAN_POINT('',(0.599667668933546,0.0199671439070972,0.06));
#38679=CARTESIAN_POINT('',(0.599667668933546,0.0199671439070972,0.325));
#38680=CARTESIAN_POINT('',(0.64,0.0431968989868597,0.06));
#38681=CARTESIAN_POINT('Origin',(0.6025,0.,0.06));
#38682=CARTESIAN_POINT('Origin',(0.,0.,0.06));
#38683=CARTESIAN_POINT('Origin',(0.16,0.,-1.16));
#38684=CARTESIAN_POINT('',(-0.16,-1.95943487863577E-17,-1.16));
#38685=CARTESIAN_POINT('Origin',(0.,0.,-1.16));
#38686=CARTESIAN_POINT('Origin',(0.,0.,-1.14));
#38687=CARTESIAN_POINT('',(-0.18,-2.20436423846524E-17,-1.14));
#38688=CARTESIAN_POINT('Origin',(0.55,0.,0.));
#38689=CARTESIAN_POINT('',(-0.55,-6.73555739531044E-17,3.81639164714898E-17));
#38690=CARTESIAN_POINT('Origin',(0.,0.,0.));
#38691=CARTESIAN_POINT('Origin',(0.,0.,0.025));
#38692=CARTESIAN_POINT('',(-0.6,-7.34788079488412E-17,0.0500000000000001));
#38693=CARTESIAN_POINT('Origin',(0.,0.,0.05));
#38694=CARTESIAN_POINT('',(-0.575,-7.04171909509728E-17,0.025));
#38695=CARTESIAN_POINT('Origin',(0.,0.,0.325));
#38696=CARTESIAN_POINT('',(-0.6,-7.34788079488412E-17,0.6));
#38697=CARTESIAN_POINT('Origin',(0.,0.,0.6));
#38698=CARTESIAN_POINT('',(-0.6,-7.34788079488412E-17,0.325));
#38699=CARTESIAN_POINT('',(-0.6,-7.34788079488412E-17,0.325));
#38700=CARTESIAN_POINT('Origin',(0.,0.,0.65));
#38701=CARTESIAN_POINT('',(-0.5,-6.12323399573677E-17,0.7));
#38702=CARTESIAN_POINT('Origin',(0.,0.,0.7));
#38703=CARTESIAN_POINT('',(-0.55,-6.73555739531044E-17,0.65));
#38704=CARTESIAN_POINT('Origin',(0.,0.,0.7));
#38705=CARTESIAN_POINT('',(0.,0.,0.));
#38706=CARTESIAN_POINT('Origin',(0.,0.,-0.387));
#38707=CARTESIAN_POINT('',(-0.146224572111309,-0.000111330236089668,-0.701584495415709));
#38708=CARTESIAN_POINT('',(-0.146224247785679,-0.000114915057078579,-0.708715504584291));
#38709=CARTESIAN_POINT('',(-0.14635,-1.79227059055215E-17,-0.387));
#38710=CARTESIAN_POINT('',(0.0262121662178374,-0.144200775921424,-0.73765));
#38711=CARTESIAN_POINT('Ctrl Pts',(-0.146224572111309,-0.000111330236089668,
-0.701584495415709));
#38712=CARTESIAN_POINT('Ctrl Pts',(-0.145989829674467,0.0324236203490019,
-0.703350319592403));
#38713=CARTESIAN_POINT('Ctrl Pts',(-0.135250992528874,0.0650987548480176,
-0.705116143769096));
#38714=CARTESIAN_POINT('Ctrl Pts',(-0.115283301657821,0.090528281986044,
-0.70688196794579));
#38715=CARTESIAN_POINT('Ctrl Pts',(-0.085590235853855,0.12834340179881,
-0.709507846612251));
#38716=CARTESIAN_POINT('Ctrl Pts',(-0.0354890897229695,0.150136061895647,
-0.712133725278713));
#38717=CARTESIAN_POINT('Ctrl Pts',(0.012418606607114,0.146058623298872,
-0.714759603945174));
#38718=CARTESIAN_POINT('Ctrl Pts',(0.0603263029371975,0.141981184702096,
-0.717385482611635));
#38719=CARTESIAN_POINT('Ctrl Pts',(0.106040549466479,0.112033647411709,
-0.720011361278096));
#38720=CARTESIAN_POINT('Ctrl Pts',(0.128919625858718,0.0697558642001005,
-0.722637239944558));
#38721=CARTESIAN_POINT('Ctrl Pts',(0.151798702250957,0.0274780809884917,
-0.725263118611019));
#38722=CARTESIAN_POINT('Ctrl Pts',(0.151842608506152,-0.0271299481443382,
-0.727888997277481));
#38723=CARTESIAN_POINT('Ctrl Pts',(0.129056444743052,-0.0694756899781577,
-0.730514875943942));
#38724=CARTESIAN_POINT('Ctrl Pts',(0.108418006355686,-0.107830105091238,
-0.732893250629295));
#38725=CARTESIAN_POINT('Ctrl Pts',(0.069050400143189,-0.136124873582162,
-0.735271625314647));
#38726=CARTESIAN_POINT('Ctrl Pts',(0.0262121662178374,-0.144200775921424,
-0.73765));
#38727=CARTESIAN_POINT('',(-0.14635,-1.79227059055215E-17,-0.73765));
#38728=CARTESIAN_POINT('Origin',(0.,0.,-0.73765));
#38729=CARTESIAN_POINT('',(-0.14635,-1.79227059055215E-17,-0.76765));
#38730=CARTESIAN_POINT('',(-0.14635,-1.79227059055215E-17,-0.387));
#38731=CARTESIAN_POINT('Origin',(0.,0.,-0.76765));
#38732=CARTESIAN_POINT('',(0.128823493644034,-0.0694465980833158,-0.73765));
#38733=CARTESIAN_POINT('Origin',(0.,0.,-0.73765));
#38734=CARTESIAN_POINT('Ctrl Pts',(0.128823493644033,-0.0694465980833164,
-0.73765));
#38735=CARTESIAN_POINT('Ctrl Pts',(0.15173931854053,-0.0269377250156972,
-0.735024121333539));
#38736=CARTESIAN_POINT('Ctrl Pts',(0.151797682753626,0.0274336672197081,
-0.732398242667077));
#38737=CARTESIAN_POINT('Ctrl Pts',(0.128963169514332,0.0696551524900372,
-0.729772364000616));
#38738=CARTESIAN_POINT('Ctrl Pts',(0.106128656275037,0.111876637760367,
-0.727146485334154));
#38739=CARTESIAN_POINT('Ctrl Pts',(0.0604012655833517,0.141948216065621,
-0.724520606667693));
#38740=CARTESIAN_POINT('Ctrl Pts',(0.0124881793788399,0.146075689420542,
-0.721894728001232));
#38741=CARTESIAN_POINT('Ctrl Pts',(-0.0354249068256719,0.150203162775464,
-0.719268849334771));
#38742=CARTESIAN_POINT('Ctrl Pts',(-0.0855236885430102,0.128386531180054,
-0.716642970668309));
#38743=CARTESIAN_POINT('Ctrl Pts',(-0.115232990782446,0.0905747836436524,
-0.714017092001848));
#38744=CARTESIAN_POINT('Ctrl Pts',(-0.135227118836764,0.0651277732727103,
-0.712249896195996));
#38745=CARTESIAN_POINT('Ctrl Pts',(-0.14598647497743,0.0324362794117622,
-0.710482700390144));
#38746=CARTESIAN_POINT('Ctrl Pts',(-0.146224247785679,-0.000114915057078579,
-0.708715504584291));
#38747=CARTESIAN_POINT('Origin',(0.,0.,-0.387));
#38748=CARTESIAN_POINT('',(-0.146579286092913,1.69649698835653E-5,-0.651584495415709));
#38749=CARTESIAN_POINT('',(-0.146579188640296,1.75704817259698E-5,-0.658715504584291));
#38750=CARTESIAN_POINT('',(-0.14635,-1.79227059055215E-17,-0.387));
#38751=CARTESIAN_POINT('Ctrl Pts',(-0.146579286092913,1.69649698835653E-5,
-0.651584495415709));
#38752=CARTESIAN_POINT('Ctrl Pts',(-0.146580846380414,0.000957028414167882,
-0.65163583559384));
#38753=CARTESIAN_POINT('Ctrl Pts',(-0.146572572236328,0.0018970636499291,
-0.651687175771971));
#38754=CARTESIAN_POINT('Ctrl Pts',(-0.146554379287511,0.00283690686036914,
-0.651738515950102));
#38755=CARTESIAN_POINT('Ctrl Pts',(-0.145623870708881,0.0509067485703208,
-0.654364394616563));
#38756=CARTESIAN_POINT('Ctrl Pts',(-0.118745958487551,0.0984742557093859,
-0.656990273283025));
#38757=CARTESIAN_POINT('Ctrl Pts',(-0.0780494861654621,0.124074549119317,
-0.659616151949486));
#38758=CARTESIAN_POINT('Ctrl Pts',(-0.0373530138433729,0.149674842529248,
-0.662242030615947));
#38759=CARTESIAN_POINT('Ctrl Pts',(0.0171620185794759,0.153307922210045,
-0.664867909282409));
#38760=CARTESIAN_POINT('Ctrl Pts',(0.0608956254433934,0.133334057017124,
-0.66749378794887));
#38761=CARTESIAN_POINT('Ctrl Pts',(0.104629232307311,0.113360191824202,
-0.670119666615332));
#38762=CARTESIAN_POINT('Ctrl Pts',(0.137581413612297,0.0697793817575608,
-0.672745545281793));
#38763=CARTESIAN_POINT('Ctrl Pts',(0.144882088293867,0.0222581942498008,
-0.675371423948254));
#38764=CARTESIAN_POINT('Ctrl Pts',(0.152182762975438,-0.0252629932579592,
-0.677997302614715));
#38765=CARTESIAN_POINT('Ctrl Pts',(0.133831931033593,-0.076724558206838,
-0.680623181281177));
#38766=CARTESIAN_POINT('Ctrl Pts',(0.0981110027231639,-0.108905303707465,
-0.683249059947638));
#38767=CARTESIAN_POINT('Ctrl Pts',(0.0623900744127351,-0.141086049208091,
-0.685874938614099));
#38768=CARTESIAN_POINT('Ctrl Pts',(0.00929904973372216,-0.153985975260466,
-0.688500817280561));
#38769=CARTESIAN_POINT('Ctrl Pts',(-0.0372055231842157,-0.141781954215198,
-0.691126695947022));
#38770=CARTESIAN_POINT('Ctrl Pts',(-0.0837100961021536,-0.12957793316993,
-0.693752574613483));
#38771=CARTESIAN_POINT('Ctrl Pts',(-0.123628217259017,-0.0922699650270199,
-0.696378453279944));
#38772=CARTESIAN_POINT('Ctrl Pts',(-0.138944785098925,-0.0466971911912179,
-0.699004331946406));
#38773=CARTESIAN_POINT('Ctrl Pts',(-0.143961423189176,-0.0317707327644562,
-0.699864386436174));
#38774=CARTESIAN_POINT('Ctrl Pts',(-0.146338904721208,-0.0159576589331395,
-0.700724440925942));
#38775=CARTESIAN_POINT('Ctrl Pts',(-0.146224572111309,-0.000111330236089668,
-0.701584495415709));
#38776=CARTESIAN_POINT('Ctrl Pts',(-0.146224247785679,-0.000114915057078579,
-0.708715504584291));
#38777=CARTESIAN_POINT('Ctrl Pts',(-0.146339781918618,-0.0159315849983372,
-0.707856821723683));
#38778=CARTESIAN_POINT('Ctrl Pts',(-0.143971168753899,-0.0317151302334793,
-0.706998138863074));
#38779=CARTESIAN_POINT('Ctrl Pts',(-0.138970783508294,-0.046618358270845,
-0.706139456002465));
#38780=CARTESIAN_POINT('Ctrl Pts',(-0.123679451233175,-0.0921928891715474,
-0.703513577336003));
#38781=CARTESIAN_POINT('Ctrl Pts',(-0.0837769639214024,-0.129535087495559,
-0.700887698669541));
#38782=CARTESIAN_POINT('Ctrl Pts',(-0.0372778401516794,-0.141766375685469,
-0.69826182000308));
#38783=CARTESIAN_POINT('Ctrl Pts',(0.00922128361804363,-0.153997663875379,
-0.695635941336619));
#38784=CARTESIAN_POINT('Ctrl Pts',(0.0623170438457172,-0.141118041931188,
-0.693010062670158));
#38785=CARTESIAN_POINT('Ctrl Pts',(0.0980541504731311,-0.108954078842552,
-0.690384184003697));
#38786=CARTESIAN_POINT('Ctrl Pts',(0.133791257100545,-0.0767901157539168,
-0.687758305337235));
#38787=CARTESIAN_POINT('Ctrl Pts',(0.152169710127699,-0.0253418115208371,
-0.685132426670773));
#38788=CARTESIAN_POINT('Ctrl Pts',(0.144893849521265,0.0221822521721539,
-0.682506548004312));
#38789=CARTESIAN_POINT('Ctrl Pts',(0.137617988914832,0.0697063158651454,
-0.679880669337851));
#38790=CARTESIAN_POINT('Ctrl Pts',(0.104687814674811,0.113306139018048,
-0.67725479067139));
#38791=CARTESIAN_POINT('Ctrl Pts',(0.0609644168294508,0.133303084391365,
-0.674628912004929));
#38792=CARTESIAN_POINT('Ctrl Pts',(0.0172410189840913,0.153300029764682,
-0.672003033338467));
#38793=CARTESIAN_POINT('Ctrl Pts',(-0.0372756024666062,0.149694097358414,
-0.669377154672006));
#38794=CARTESIAN_POINT('Ctrl Pts',(-0.0779852394339466,0.124114604981169,
-0.666751276005544));
#38795=CARTESIAN_POINT('Ctrl Pts',(-0.118694876401287,0.0985351126039237,
-0.664125397339083));
#38796=CARTESIAN_POINT('Ctrl Pts',(-0.14559752888527,0.050982060255701,
-0.661499518672622));
#38797=CARTESIAN_POINT('Ctrl Pts',(-0.146552928848993,0.00291283741010483,
-0.65887364000616));
#38798=CARTESIAN_POINT('Ctrl Pts',(-0.146572107518371,0.00194789731459742,
-0.658820928198871));
#38799=CARTESIAN_POINT('Ctrl Pts',(-0.146580830372945,0.000982749220839569,
-0.658768216391581));
#38800=CARTESIAN_POINT('Ctrl Pts',(-0.146579188640296,1.75704817259698E-5,
-0.658715504584291));
#38801=CARTESIAN_POINT('Origin',(0.,0.,-0.387));
#38802=CARTESIAN_POINT('',(-0.146183638882289,9.23670094306398E-5,-0.601584495415709));
#38803=CARTESIAN_POINT('',(-0.146183142687711,9.20871909961158E-5,-0.608715504584291));
#38804=CARTESIAN_POINT('',(-0.14635,-1.79227059055215E-17,-0.387));
#38805=CARTESIAN_POINT('Ctrl Pts',(-0.146183638882289,9.23670094306398E-5,
-0.601584495415709));
#38806=CARTESIAN_POINT('Ctrl Pts',(-0.146288013988482,0.0178439142218399,
-0.602547230261739));
#38807=CARTESIAN_POINT('Ctrl Pts',(-0.143291093723304,0.0355614332192032,
-0.603509965107768));
#38808=CARTESIAN_POINT('Ctrl Pts',(-0.137032927084621,0.0520404416997214,
-0.604472699953798));
#38809=CARTESIAN_POINT('Ctrl Pts',(-0.119963651639312,0.0969872689511545,
-0.60709857862026));
#38810=CARTESIAN_POINT('Ctrl Pts',(-0.0786327707208103,0.132720363140831,
-0.609724457286721));
#38811=CARTESIAN_POINT('Ctrl Pts',(-0.0316910142969177,0.143115023213958,
-0.612350335953183));
#38812=CARTESIAN_POINT('Ctrl Pts',(0.0152507421269743,0.153509683287086,
-0.614976214619644));
#38813=CARTESIAN_POINT('Ctrl Pts',(0.0678033740562569,0.138565909243665,
-0.617602093286105));
#38814=CARTESIAN_POINT('Ctrl Pts',(0.102252295370017,0.105027133840093,
-0.620227971952566));
#38815=CARTESIAN_POINT('Ctrl Pts',(0.136701216683777,0.0714883584365206,
-0.622853850619027));
#38816=CARTESIAN_POINT('Ctrl Pts',(0.153046427382013,0.0193545816727964,
-0.625479729285489));
#38817=CARTESIAN_POINT('Ctrl Pts',(0.143912078720802,-0.027848605678599,
-0.62810560795195));
#38818=CARTESIAN_POINT('Ctrl Pts',(0.134777730059591,-0.0750517930299941,
-0.630731486618412));
#38819=CARTESIAN_POINT('Ctrl Pts',(0.100163822038932,-0.117324390969061,
-0.633357365284873));
#38820=CARTESIAN_POINT('Ctrl Pts',(0.0556900327358894,-0.135590739689116,
-0.635983243951334));
#38821=CARTESIAN_POINT('Ctrl Pts',(0.0112162434328469,-0.153857088409171,
-0.638609122617795));
#38822=CARTESIAN_POINT('Ctrl Pts',(-0.0431174271525793,-0.148117187910216,
-0.641235001284257));
#38823=CARTESIAN_POINT('Ctrl Pts',(-0.0827927099773264,-0.120961149520319,
-0.643860879950718));
#38824=CARTESIAN_POINT('Ctrl Pts',(-0.121692276805127,-0.094336055635236,
-0.646435418439049));
#38825=CARTESIAN_POINT('Ctrl Pts',(-0.146501042885148,-0.047124077521472,
-0.649009956927379));
#38826=CARTESIAN_POINT('Ctrl Pts',(-0.146579286092913,1.69649698835653E-5,
-0.651584495415709));
#38827=CARTESIAN_POINT('Ctrl Pts',(-0.146579188640296,1.75704817259698E-5,
-0.658715504584291));
#38828=CARTESIAN_POINT('Ctrl Pts',(-0.146499046215644,-0.0470983618370304,
-0.656142337725119));
#38829=CARTESIAN_POINT('Ctrl Pts',(-0.121720317494026,-0.0942873213731057,
-0.653569170865948));
#38830=CARTESIAN_POINT('Ctrl Pts',(-0.0828552235665306,-0.120918396970429,
-0.650996004006776));
#38831=CARTESIAN_POINT('Ctrl Pts',(-0.0431939708768843,-0.148095015162397,
-0.648370125340315));
#38832=CARTESIAN_POINT('Ctrl Pts',(0.0111366819458703,-0.153862858203364,
-0.645744246673854));
#38833=CARTESIAN_POINT('Ctrl Pts',(0.0556198997683811,-0.13561947345926,
-0.643118368007392));
#38834=CARTESIAN_POINT('Ctrl Pts',(0.100103117590892,-0.117376088715157,
-0.640492489340931));
#38835=CARTESIAN_POINT('Ctrl Pts',(0.134738900413159,-0.0751214761859832,
-0.637866610674469));
#38836=CARTESIAN_POINT('Ctrl Pts',(0.143897661097196,-0.0279230386888887,
-0.635240732008008));
#38837=CARTESIAN_POINT('Ctrl Pts',(0.153056421781233,0.0192753988082057,
-0.632614853341547));
#38838=CARTESIAN_POINT('Ctrl Pts',(0.136738160327041,0.071417661273221,
-0.629988974675086));
#38839=CARTESIAN_POINT('Ctrl Pts',(0.102306584507141,0.104974254510237,
-0.627363096008625));
#38840=CARTESIAN_POINT('Ctrl Pts',(0.0678750086872403,0.138530847747253,
-0.624737217342164));
#38841=CARTESIAN_POINT('Ctrl Pts',(0.0153301185016322,0.15350177175627,
-0.622111338675701));
#38842=CARTESIAN_POINT('Ctrl Pts',(-0.031617003941353,0.143131381312434,
-0.61948546000924));
#38843=CARTESIAN_POINT('Ctrl Pts',(-0.0785641263843382,0.132760990868598,
-0.616859581342778));
#38844=CARTESIAN_POINT('Ctrl Pts',(-0.119913481084701,0.0970492859719075,
-0.614233702676318));
#38845=CARTESIAN_POINT('Ctrl Pts',(-0.137005996168408,0.0521112951099759,
-0.611607824009857));
#38846=CARTESIAN_POINT('Ctrl Pts',(-0.143281611519541,0.0356120529609342,
-0.610643717534669));
#38847=CARTESIAN_POINT('Ctrl Pts',(-0.146287323594326,0.017869076542175,
-0.60967961105948));
#38848=CARTESIAN_POINT('Ctrl Pts',(-0.146183142687711,9.20871909961158E-5,
-0.608715504584291));
#38849=CARTESIAN_POINT('Origin',(0.,0.,-0.387));
#38850=CARTESIAN_POINT('',(-0.146276019243273,-0.00012357004413352,-0.55158449541571));
#38851=CARTESIAN_POINT('',(-0.146276703831537,-0.000123683174109515,-0.558715504584291));
#38852=CARTESIAN_POINT('',(-0.14635,-1.79227059055215E-17,-0.387));
#38853=CARTESIAN_POINT('Ctrl Pts',(-0.146276019243273,-0.00012357004413352,
-0.55158449541571));
#38854=CARTESIAN_POINT('Ctrl Pts',(-0.145991697039028,0.0343777221702149,
-0.553458624929638));
#38855=CARTESIAN_POINT('Ctrl Pts',(-0.133769924250195,0.0690603428635732,
-0.555332754443566));
#38856=CARTESIAN_POINT('Ctrl Pts',(-0.111492926407665,0.0951606952569379,
-0.557206883957495));
#38857=CARTESIAN_POINT('Ctrl Pts',(-0.0802801991373442,0.131730397632097,
-0.559832762623956));
#38858=CARTESIAN_POINT('Ctrl Pts',(-0.0293277101925237,0.151451950914244,
-0.562458641290417));
#38859=CARTESIAN_POINT('Ctrl Pts',(0.0183720222342842,0.145425923930635,
-0.565084519956878));
#38860=CARTESIAN_POINT('Ctrl Pts',(0.066071754661092,0.139399896947026,
-0.56771039862334));
#38861=CARTESIAN_POINT('Ctrl Pts',(0.110518730569887,0.107626289697661,
-0.570336277289801));
#38862=CARTESIAN_POINT('Ctrl Pts',(0.131656071121403,0.0644430717323258,
-0.572962155956262));
#38863=CARTESIAN_POINT('Ctrl Pts',(0.152793411672919,0.021259853766991,
-0.575588034622724));
#38864=CARTESIAN_POINT('Ctrl Pts',(0.150621116867156,-0.0333329749143135,
-0.578213913289185));
#38865=CARTESIAN_POINT('Ctrl Pts',(0.126119443458436,-0.0747001777727409,
-0.580839791955647));
#38866=CARTESIAN_POINT('Ctrl Pts',(0.101617770049717,-0.116067380631168,
-0.583465670622108));
#38867=CARTESIAN_POINT('Ctrl Pts',(0.0547867180380415,-0.144208957666719,
-0.586091549288569));
#38868=CARTESIAN_POINT('Ctrl Pts',(0.00675899061544872,-0.146425908097131,
-0.58871742795503));
#38869=CARTESIAN_POINT('Ctrl Pts',(-0.0412687368071444,-0.148642858527543,
-0.591343306621491));
#38870=CARTESIAN_POINT('Ctrl Pts',(-0.0904931396406548,-0.124935182352816,
-0.593969185287953));
#38871=CARTESIAN_POINT('Ctrl Pts',(-0.118701506071351,-0.086001064108858,
-0.596595063954414));
#38872=CARTESIAN_POINT('Ctrl Pts',(-0.136567742966793,-0.0613414943471455,
-0.598258207774846));
#38873=CARTESIAN_POINT('Ctrl Pts',(-0.146003328785914,-0.0305737880291827,
-0.599921351595278));
#38874=CARTESIAN_POINT('Ctrl Pts',(-0.146183638882289,9.23670094306398E-5,
-0.601584495415709));
#38875=CARTESIAN_POINT('Ctrl Pts',(-0.146183142687711,9.20871909961158E-5,
-0.608715504584291));
#38876=CARTESIAN_POINT('Ctrl Pts',(-0.146003572341562,-0.0305490373202445,
-0.607053732393019));
#38877=CARTESIAN_POINT('Ctrl Pts',(-0.136584715823453,-0.0612912120020383,
-0.605391960201745));
#38878=CARTESIAN_POINT('Ctrl Pts',(-0.118745956960722,-0.0859396723257687,
-0.603730188010472));
#38879=CARTESIAN_POINT('Ctrl Pts',(-0.0905577272022776,-0.124888372072408,
-0.601104309344011));
#38880=CARTESIAN_POINT('Ctrl Pts',(-0.0413455922183362,-0.148621494738514,
-0.59847843067755));
#38881=CARTESIAN_POINT('Ctrl Pts',(0.00668327362850226,-0.146429378651901,
-0.595852552011089));
#38882=CARTESIAN_POINT('Ctrl Pts',(0.0547121394753407,-0.144237262565288,
-0.593226673344627));
#38883=CARTESIAN_POINT('Ctrl Pts',(0.101557736185076,-0.116119907725956,
-0.590600794678166));
#38884=CARTESIAN_POINT('Ctrl Pts',(0.126080796403966,-0.0747653815530347,
-0.587974916011705));
#38885=CARTESIAN_POINT('Ctrl Pts',(0.150603856622856,-0.0334108553801132,
-0.585349037345243));
#38886=CARTESIAN_POINT('Ctrl Pts',(0.152804380350901,0.021180842126398,
-0.582723158678783));
#38887=CARTESIAN_POINT('Ctrl Pts',(0.131689372842645,0.0643749832966417,
-0.580097280012321));
#38888=CARTESIAN_POINT('Ctrl Pts',(0.110574365334389,0.107569124466885,
-0.57747140134586));
#38889=CARTESIAN_POINT('Ctrl Pts',(0.0661438265898331,0.139365709300861,
-0.574845522679397));
#38890=CARTESIAN_POINT('Ctrl Pts',(0.0184472178872199,0.145416400350861,
-0.572219644012936));
#38891=CARTESIAN_POINT('Ctrl Pts',(-0.0292493908153934,0.15146709140086,
-0.569593765346475));
#38892=CARTESIAN_POINT('Ctrl Pts',(-0.080212069476064,0.131771888666882,
-0.566967886680015));
#38893=CARTESIAN_POINT('Ctrl Pts',(-0.111443701633747,0.0952183320922368,
-0.564342008013553));
#38894=CARTESIAN_POINT('Ctrl Pts',(-0.133750506041868,0.069110409431805,
-0.562466506870466));
#38895=CARTESIAN_POINT('Ctrl Pts',(-0.145991807584391,0.0344024457716816,
-0.560591005727379));
#38896=CARTESIAN_POINT('Ctrl Pts',(-0.146276703831537,-0.000123683174109515,
-0.558715504584291));
#38897=CARTESIAN_POINT('Origin',(0.,0.,-0.387));
#38898=CARTESIAN_POINT('',(-0.146558953229823,5.11349905732411E-5,-0.501584495415709));
#38899=CARTESIAN_POINT('',(-0.146558577250774,5.15455280380561E-5,-0.508715504584291));
#38900=CARTESIAN_POINT('',(-0.14635,-1.79227059055215E-17,-0.387));
#38901=CARTESIAN_POINT('Ctrl Pts',(-0.146558953229823,5.11349905732411E-5,
-0.501584495415709));
#38902=CARTESIAN_POINT('Ctrl Pts',(-0.146572307834264,0.00297540766026488,
-0.501744140931075));
#38903=CARTESIAN_POINT('Ctrl Pts',(-0.146492243279588,0.00589893547541245,
-0.501903786446441));
#38904=CARTESIAN_POINT('Ctrl Pts',(-0.14631642585259,0.00881669344130144,
-0.502063431961807));
#38905=CARTESIAN_POINT('Ctrl Pts',(-0.143424548622659,0.0568085106807304,
-0.504689310628268));
#38906=CARTESIAN_POINT('Ctrl Pts',(-0.114627428195741,0.103239337167309,
-0.507315189294729));
#38907=CARTESIAN_POINT('Ctrl Pts',(-0.0729198824504026,0.127157073342488,
-0.509941067961191));
#38908=CARTESIAN_POINT('Ctrl Pts',(-0.0312123367050647,0.151074809517666,
-0.512566946627652));
#38909=CARTESIAN_POINT('Ctrl Pts',(0.0234056343586937,0.152479455381444,
-0.515192825294113));
#38910=CARTESIAN_POINT('Ctrl Pts',(0.0662874488469095,0.130737158768342,
-0.517818703960575));
#38911=CARTESIAN_POINT('Ctrl Pts',(0.109169263335126,0.108994862155241,
-0.520444582627036));
#38912=CARTESIAN_POINT('Ctrl Pts',(0.140314921247799,0.0641056230652594,
-0.523070461293497));
#38913=CARTESIAN_POINT('Ctrl Pts',(0.145669817601684,0.0163258934620395,
-0.525696339959959));
#38914=CARTESIAN_POINT('Ctrl Pts',(0.151024713955569,-0.0314538361411797,
-0.52832221862642));
#38915=CARTESIAN_POINT('Ctrl Pts',(0.130588848750667,-0.0821240562576371,
-0.530948097292881));
#38916=CARTESIAN_POINT('Ctrl Pts',(0.093583989390229,-0.112819623682389,
-0.533573975959343));
#38917=CARTESIAN_POINT('Ctrl Pts',(0.0565791300297904,-0.143515191107141,
-0.536199854625804));
#38918=CARTESIAN_POINT('Ctrl Pts',(0.00300527651381574,-0.154236105840187,
-0.538825733292265));
#38919=CARTESIAN_POINT('Ctrl Pts',(-0.0429621515554171,-0.140144511453598,
-0.541451611958726));
#38920=CARTESIAN_POINT('Ctrl Pts',(-0.0889295796246497,-0.126052917067009,
-0.544077490625188));
#38921=CARTESIAN_POINT('Ctrl Pts',(-0.12729058224714,-0.0871488135607851,
-0.546703369291649));
#38922=CARTESIAN_POINT('Ctrl Pts',(-0.140734600760475,-0.040987836073588,
-0.54932924795811));
#38923=CARTESIAN_POINT('Ctrl Pts',(-0.144583418930606,-0.0277726498011545,
-0.550080997110644));
#38924=CARTESIAN_POINT('Ctrl Pts',(-0.146390066311258,-0.0139626974847263,
-0.550832746263176));
#38925=CARTESIAN_POINT('Ctrl Pts',(-0.146276019243273,-0.00012357004413352,
-0.55158449541571));
#38926=CARTESIAN_POINT('Ctrl Pts',(-0.146276703831537,-0.000123683174109515,
-0.558715504584291));
#38927=CARTESIAN_POINT('Ctrl Pts',(-0.146390689227462,-0.0139373943656652,
-0.557965127060917));
#38928=CARTESIAN_POINT('Ctrl Pts',(-0.144590746625787,-0.0277219982676888,
-0.557214749537542));
#38929=CARTESIAN_POINT('Ctrl Pts',(-0.140755772561096,-0.0409150567738682,
-0.556464372014168));
#38930=CARTESIAN_POINT('Ctrl Pts',(-0.127335625676068,-0.0870829786500136,
-0.553838493347707));
#38931=CARTESIAN_POINT('Ctrl Pts',(-0.088994746251319,-0.126006911986991,
-0.551212614681246));
#38932=CARTESIAN_POINT('Ctrl Pts',(-0.0430346122416979,-0.140122273475387,
-0.548586736014785));
#38933=CARTESIAN_POINT('Ctrl Pts',(0.00292552176792324,-0.154237634963784,
-0.545960857348324));
#38934=CARTESIAN_POINT('Ctrl Pts',(0.0565049103624161,-0.1435444246036,
-0.543334978681862));
#38935=CARTESIAN_POINT('Ctrl Pts',(0.0935256361956055,-0.112867997047911,
-0.540709100015401));
#38936=CARTESIAN_POINT('Ctrl Pts',(0.130546362028795,-0.082191569492223,
-0.538083221348939));
#38937=CARTESIAN_POINT('Ctrl Pts',(0.151008425100681,-0.0315319247410302,
-0.535457342682478));
#38938=CARTESIAN_POINT('Ctrl Pts',(0.145678236122874,0.0162505661438082,
-0.532831464016017));
#38939=CARTESIAN_POINT('Ctrl Pts',(0.140348047145067,0.0640330570286466,
-0.530205585349556));
#38940=CARTESIAN_POINT('Ctrl Pts',(0.109225606117568,0.108938394047131,
-0.527579706683094));
#38941=CARTESIAN_POINT('Ctrl Pts',(0.0663550413048699,0.130702860997484,
-0.524953828016633));
#38942=CARTESIAN_POINT('Ctrl Pts',(0.0234844764921716,0.152467327947837,
-0.522327949350172));
#38943=CARTESIAN_POINT('Ctrl Pts',(-0.0311342121057257,0.151090924830058,
-0.519702070683711));
#38944=CARTESIAN_POINT('Ctrl Pts',(-0.0728541188021517,0.127194759146169,
-0.517076192017249));
#38945=CARTESIAN_POINT('Ctrl Pts',(-0.114574025498578,0.103298593462279,
-0.514450313350788));
#38946=CARTESIAN_POINT('Ctrl Pts',(-0.143395150293532,0.0568826652122784,
-0.511824434684326));
#38947=CARTESIAN_POINT('Ctrl Pts',(-0.146311843240925,0.0088923510696771,
-0.509198556017865));
#38948=CARTESIAN_POINT('Ctrl Pts',(-0.146490692924973,0.00594961672068545,
-0.50903753887334));
#38949=CARTESIAN_POINT('Ctrl Pts',(-0.146572140355928,0.00300096258414241,
-0.508876521728815));
#38950=CARTESIAN_POINT('Ctrl Pts',(-0.146558577250774,5.15455280380561E-5,
-0.508715504584291));
#38951=CARTESIAN_POINT('Origin',(0.,0.,-0.387));
#38952=CARTESIAN_POINT('',(-0.146149944725445,6.74938752725091E-5,-0.45158449541571));
#38953=CARTESIAN_POINT('',(-0.146149585450786,6.71495220561266E-5,-0.458715504584291));
#38954=CARTESIAN_POINT('',(-0.14635,-1.79227059055215E-17,-0.387));
#38955=CARTESIAN_POINT('Ctrl Pts',(-0.146149944725445,6.74938752725091E-5,
-0.45158449541571));
#38956=CARTESIAN_POINT('Ctrl Pts',(-0.146233574579168,0.0198274883748786,
-0.452655535598974));
#38957=CARTESIAN_POINT('Ctrl Pts',(-0.142499208073291,0.0395571999694397,
-0.453726575782238));
#38958=CARTESIAN_POINT('Ctrl Pts',(-0.134794490127502,0.0575905894118108,
-0.454797615965503));
#38959=CARTESIAN_POINT('Ctrl Pts',(-0.115904765165658,0.101803209405565,
-0.457423494631964));
#38960=CARTESIAN_POINT('Ctrl Pts',(-0.0731497494270609,0.135819447032232,
-0.460049373298425));
#38961=CARTESIAN_POINT('Ctrl Pts',(-0.0258228178984385,0.144289336519784,
-0.462675251964887));
#38962=CARTESIAN_POINT('Ctrl Pts',(0.0215041136301832,0.152759226007335,
-0.465301130631348));
#38963=CARTESIAN_POINT('Ctrl Pts',(0.07340296094883,0.135682767355774,-0.467927009297809));
#38964=CARTESIAN_POINT('Ctrl Pts',(0.106454157828814,0.100765782081473,
-0.470552887964271));
#38965=CARTESIAN_POINT('Ctrl Pts',(0.139505354708799,0.0658487968071709,
-0.473178766630732));
#38966=CARTESIAN_POINT('Ctrl Pts',(0.153708901150121,0.0130912849101291,
-0.475804645297193));
#38967=CARTESIAN_POINT('Ctrl Pts',(0.142655388972272,-0.0336997114928278,
-0.478430523963655));
#38968=CARTESIAN_POINT('Ctrl Pts',(0.131601876794424,-0.080490707895784,
-0.481056402630116));
#38969=CARTESIAN_POINT('Ctrl Pts',(0.0952913059974063,-0.121315188804656,
-0.483682281296577));
#38970=CARTESIAN_POINT('Ctrl Pts',(0.0501089695407642,-0.137750940937284,
-0.486308159963038));
#38971=CARTESIAN_POINT('Ctrl Pts',(0.00492663308412149,-0.154186693069913,
-0.4889340386295));
#38972=CARTESIAN_POINT('Ctrl Pts',(-0.0491274690321459,-0.146233716426298,
-0.491559917295961));
#38973=CARTESIAN_POINT('Ctrl Pts',(-0.0876612030738067,-0.117480824108352,
-0.494185795962423));
#38974=CARTESIAN_POINT('Ctrl Pts',(-0.123852202125988,-0.09047602105705,
-0.496652029113518));
#38975=CARTESIAN_POINT('Ctrl Pts',(-0.146352648855303,-0.0451235646200959,
-0.499118262264614));
#38976=CARTESIAN_POINT('Ctrl Pts',(-0.146558953229823,5.11349905732411E-5,
-0.501584495415709));
#38977=CARTESIAN_POINT('Ctrl Pts',(-0.146558577250774,5.15455280380561E-5,
-0.508715504584291));
#38978=CARTESIAN_POINT('Ctrl Pts',(-0.146350952304311,-0.0450983336056391,
-0.506250643062354));
#38979=CARTESIAN_POINT('Ctrl Pts',(-0.123878846251419,-0.0904269929973202,
-0.503785781540418));
#38980=CARTESIAN_POINT('Ctrl Pts',(-0.0877219373438008,-0.117435476278519,
-0.501320920018481));
#38981=CARTESIAN_POINT('Ctrl Pts',(-0.0492030773994497,-0.146208289448912,
-0.49869504135202));
#38982=CARTESIAN_POINT('Ctrl Pts',(0.00484690358908479,-0.154189215754497,
-0.496069162685559));
#38983=CARTESIAN_POINT('Ctrl Pts',(0.0500377315628808,-0.137776829693206,
-0.493443284019097));
#38984=CARTESIAN_POINT('Ctrl Pts',(0.0952285595366766,-0.121364443631916,
-0.490817405352636));
#38985=CARTESIAN_POINT('Ctrl Pts',(0.131560234495734,-0.08055874520375,
-0.488191526686174));
#38986=CARTESIAN_POINT('Ctrl Pts',(0.142637940141625,-0.0337734720206651,
-0.485565648019713));
#38987=CARTESIAN_POINT('Ctrl Pts',(0.153715645787515,0.0130118011624195,
-0.482939769353252));
#38988=CARTESIAN_POINT('Ctrl Pts',(0.13953938212024,0.0657766491004227,
-0.480313890686791));
#38989=CARTESIAN_POINT('Ctrl Pts',(0.106506245857298,0.100710719258534,
-0.477688012020329));
#38990=CARTESIAN_POINT('Ctrl Pts',(0.0734731095943562,0.135644789416646,
-0.475062133353868));
#38991=CARTESIAN_POINT('Ctrl Pts',(0.0215831007357463,0.152748081794866,
-0.472436254687406));
#38992=CARTESIAN_POINT('Ctrl Pts',(-0.0257482028808791,0.144302666048177,
-0.469810376020945));
#38993=CARTESIAN_POINT('Ctrl Pts',(-0.0730795064975037,0.135857250301488,
-0.467184497354483));
#38994=CARTESIAN_POINT('Ctrl Pts',(-0.115852104872144,0.101863126429891,
-0.464558618688023));
#38995=CARTESIAN_POINT('Ctrl Pts',(-0.134764688781975,0.0576602812834753,
-0.461932740021561));
#38996=CARTESIAN_POINT('Ctrl Pts',(-0.142488609406108,0.0396077894135385,
-0.460860328209138));
#38997=CARTESIAN_POINT('Ctrl Pts',(-0.14623288284995,0.0198525697897848,
-0.459787916396715));
#38998=CARTESIAN_POINT('Ctrl Pts',(-0.146149585450786,6.71495220561266E-5,
-0.458715504584291));
#38999=CARTESIAN_POINT('Origin',(0.,0.,-0.387));
#39000=CARTESIAN_POINT('',(-0.146332552080289,-0.000128504436232912,-0.401584495415709));
#39001=CARTESIAN_POINT('',(-0.146333285427459,-0.000128513713091357,-0.408715504584291));
#39002=CARTESIAN_POINT('',(-0.14635,-1.79227059055215E-17,-0.387));
#39003=CARTESIAN_POINT('Ctrl Pts',(-0.146332552080289,-0.000128504436232912,
-0.401584495415709));
#39004=CARTESIAN_POINT('Ctrl Pts',(-0.146009415250695,0.0363306749157212,
-0.403566930266872));
#39005=CARTESIAN_POINT('Ctrl Pts',(-0.132187350767056,0.0730085897307187,
-0.405549365118036));
#39006=CARTESIAN_POINT('Ctrl Pts',(-0.10751565831347,0.0996323932009806,
-0.407531799969199));
#39007=CARTESIAN_POINT('Ctrl Pts',(-0.07483621321526,0.134897550848709,
-0.41015767863566));
#39008=CARTESIAN_POINT('Ctrl Pts',(-0.0231211795979774,0.152522847755272,
-0.412783557302122));
#39009=CARTESIAN_POINT('Ctrl Pts',(0.0242928229910914,0.144554796906423,
-0.415409435968583));
#39010=CARTESIAN_POINT('Ctrl Pts',(0.0717068255801609,0.136586746057574,
-0.418035314635044));
#39011=CARTESIAN_POINT('Ctrl Pts',(0.114819797141016,0.103025347453312,
-0.420661193301506));
#39012=CARTESIAN_POINT('Ctrl Pts',(0.134176833664228,0.0590153189042965,
-0.423287071967967));
#39013=CARTESIAN_POINT('Ctrl Pts',(0.153533870187439,0.0150052903552816,
-0.425912950634428));
#39014=CARTESIAN_POINT('Ctrl Pts',(0.149134971673008,-0.0394533681384863,
-0.428538829300889));
#39015=CARTESIAN_POINT('Ctrl Pts',(0.122965158991617,-0.0797859651298404,
-0.431164707967351));
#39016=CARTESIAN_POINT('Ctrl Pts',(0.0967953463102253,-0.120118562121195,
-0.433790586633812));
#39017=CARTESIAN_POINT('Ctrl Pts',(0.0488546194618744,-0.146325097610136,
-0.436416465300273));
#39018=CARTESIAN_POINT('Ctrl Pts',(0.000776426692189965,-0.146579765722031,
-0.439042343966735));
#39019=CARTESIAN_POINT('Ctrl Pts',(-0.0473017660774945,-0.146834433833927,
-0.441668222633196));
#39020=CARTESIAN_POINT('Ctrl Pts',(-0.0955174247685125,-0.121137234568778,
-0.444294101299657));
#39021=CARTESIAN_POINT('Ctrl Pts',(-0.122113037021476,-0.0810841337557813,
-0.446919979966119));
#39022=CARTESIAN_POINT('Ctrl Pts',(-0.137860863432212,-0.057367842782088,
-0.448474818449316));
#39023=CARTESIAN_POINT('Ctrl Pts',(-0.146028538528979,-0.0286182644705103,
-0.450029656932513));
#39024=CARTESIAN_POINT('Ctrl Pts',(-0.146149944725445,6.74938752725091E-5,
-0.45158449541571));
#39025=CARTESIAN_POINT('Ctrl Pts',(-0.146149585450786,6.71495220561266E-5,
-0.458715504584291));
#39026=CARTESIAN_POINT('Ctrl Pts',(-0.146028923082908,-0.0285934771356052,
-0.457162037730253));
#39027=CARTESIAN_POINT('Ctrl Pts',(-0.137876624263401,-0.0573174757341037,
-0.455608570876215));
#39028=CARTESIAN_POINT('Ctrl Pts',(-0.122154945305088,-0.0810209770226571,
-0.454055104022177));
#39029=CARTESIAN_POINT('Ctrl Pts',(-0.0955800484733484,-0.121087823761136,
-0.451429225355716));
#39030=CARTESIAN_POINT('Ctrl Pts',(-0.0473776853648489,-0.146809950816859,
-0.448803346689255));
#39031=CARTESIAN_POINT('Ctrl Pts',(0.000700631346777343,-0.146580143593576,
-0.446177468022793));
#39032=CARTESIAN_POINT('Ctrl Pts',(0.0487789480584043,-0.146350336370292,
-0.443551589356332));
#39033=CARTESIAN_POINT('Ctrl Pts',(0.0967332183731576,-0.120168594868002,
-0.44092571068987));
#39034=CARTESIAN_POINT('Ctrl Pts',(0.122923882501041,-0.0798495365738923,
-0.438299832023409));
#39035=CARTESIAN_POINT('Ctrl Pts',(0.149114546628924,-0.0395304782797837,
-0.435673953356947));
#39036=CARTESIAN_POINT('Ctrl Pts',(0.153541604569938,0.0149258968061441,
-0.433048074690487));
#39037=CARTESIAN_POINT('Ctrl Pts',(0.134207328397462,0.0589459276338191,
-0.430422196024026));
#39038=CARTESIAN_POINT('Ctrl Pts',(0.114873052224986,0.102965958461495,
-0.427796317357564));
#39039=CARTESIAN_POINT('Ctrl Pts',(0.0717774419390191,0.136549645030918,
-0.425170438691102));
#39040=CARTESIAN_POINT('Ctrl Pts',(0.0243675672029892,0.144542211996371,
-0.422544560024641));
#39041=CARTESIAN_POINT('Ctrl Pts',(-0.0230423075330403,0.152534778961823,
-0.419918681358179));
#39042=CARTESIAN_POINT('Ctrl Pts',(-0.0747664467191323,0.134936226323305,
-0.417292802691719));
#39043=CARTESIAN_POINT('Ctrl Pts',(-0.107464121882991,0.0996879726351853,
-0.414666924025257));
#39044=CARTESIAN_POINT('Ctrl Pts',(-0.132166656965825,0.0730585190432724,
-0.412683117544935));
#39045=CARTESIAN_POINT('Ctrl Pts',(-0.146009753208469,0.0363554201922197,
-0.410699311064613));
#39046=CARTESIAN_POINT('Ctrl Pts',(-0.146333285427459,-0.000128513713091357,
-0.408715504584291));
#39047=CARTESIAN_POINT('Origin',(0.,0.,-0.387));
#39048=CARTESIAN_POINT('',(-0.146522325141606,8.10297640452141E-5,-0.35158449541571));
#39049=CARTESIAN_POINT('',(-0.146521772955861,8.13712719715056E-5,-0.358715504584291));
#39050=CARTESIAN_POINT('',(-0.14635,-1.79227059055215E-17,-0.387));
#39051=CARTESIAN_POINT('Ctrl Pts',(-0.146522325141606,8.10297640452141E-5,
-0.35158449541571));
#39052=CARTESIAN_POINT('Ctrl Pts',(-0.146555231621681,0.00499241344169051,
-0.35185244626831));
#39053=CARTESIAN_POINT('Ctrl Pts',(-0.146329339568258,0.00990073582968819,
-0.352120397120911));
#39054=CARTESIAN_POINT('Ctrl Pts',(-0.145834593749664,0.0147818071765353,
-0.352388347973511));
#39055=CARTESIAN_POINT('Ctrl Pts',(-0.140986158009458,0.0626155833887401,
-0.355014226639972));
#39056=CARTESIAN_POINT('Ctrl Pts',(-0.110317787182484,0.107832248722449,
-0.357640105306433));
#39057=CARTESIAN_POINT('Ctrl Pts',(-0.0676687085120385,0.130027598785206,
-0.360265983972895));
#39058=CARTESIAN_POINT('Ctrl Pts',(-0.0250196298415937,0.152222948847963,
-0.362891862639356));
#39059=CARTESIAN_POINT('Ctrl Pts',(0.0296101566723226,0.151396983639769,
-0.365517741305818));
#39060=CARTESIAN_POINT('Ctrl Pts',(0.071568737366472,0.127922423324852,
-0.368143619972279));
#39061=CARTESIAN_POINT('Ctrl Pts',(0.113527318060621,0.104447863009936,
-0.37076949863874));
#39062=CARTESIAN_POINT('Ctrl Pts',(0.142814692935004,0.0583247075882974,
-0.373395377305201));
#39063=CARTESIAN_POINT('Ctrl Pts',(0.146214814794519,0.0103662187965668,
-0.376021255971663));
#39064=CARTESIAN_POINT('Ctrl Pts',(0.149614936654034,-0.0375922699951634,
-0.378647134638124));
#39065=CARTESIAN_POINT('Ctrl Pts',(0.127127805498682,-0.0873860921569855,
-0.381273013304586));
#39066=CARTESIAN_POINT('Ctrl Pts',(0.0889008308489892,-0.116545582635693,
-0.383898891971047));
#39067=CARTESIAN_POINT('Ctrl Pts',(0.0506738561992962,-0.145705073114401,
-0.386524770637508));
#39068=CARTESIAN_POINT('Ctrl Pts',(-0.00329296194473747,-0.154230231909994,
-0.38915064930397));
#39069=CARTESIAN_POINT('Ctrl Pts',(-0.0486468770969522,-0.138274046394281,
-0.391776527970431));
#39070=CARTESIAN_POINT('Ctrl Pts',(-0.0940007922491663,-0.122317860878569,
-0.394402406636892));
#39071=CARTESIAN_POINT('Ctrl Pts',(-0.130741804409562,-0.0818803310515519,
-0.397028285303353));
#39072=CARTESIAN_POINT('Ctrl Pts',(-0.14229038220019,-0.0352090569435971,
-0.399654163969815));
#39073=CARTESIAN_POINT('Ctrl Pts',(-0.145120239135235,-0.0237727544744814,
-0.400297607785113));
#39074=CARTESIAN_POINT('Ctrl Pts',(-0.146437433405582,-0.0119621510506967,
-0.400941051600411));
#39075=CARTESIAN_POINT('Ctrl Pts',(-0.146332552080289,-0.000128504436232912,
-0.401584495415709));
#39076=CARTESIAN_POINT('Ctrl Pts',(-0.146333285427459,-0.000128513713091357,
-0.408715504584291));
#39077=CARTESIAN_POINT('Ctrl Pts',(-0.146437998785942,-0.0119367820265121,
-0.408073432398151));
#39078=CARTESIAN_POINT('Ctrl Pts',(-0.145126488659511,-0.0237220920150426,
-0.407431360212012));
#39079=CARTESIAN_POINT('Ctrl Pts',(-0.142308565599436,-0.0351354740572363,
-0.406789288025873));
#39080=CARTESIAN_POINT('Ctrl Pts',(-0.130784123010399,-0.0818127123238171,
-0.404163409359411));
#39081=CARTESIAN_POINT('Ctrl Pts',(-0.0940640266907015,-0.122269234119258,
-0.401537530692951));
#39082=CARTESIAN_POINT('Ctrl Pts',(-0.0487183696599885,-0.13824886921009,
-0.398911652026489));
#39083=CARTESIAN_POINT('Ctrl Pts',(-0.00337271262927494,-0.154228504300922,
-0.396285773360028));
#39084=CARTESIAN_POINT('Ctrl Pts',(0.0505985051124538,-0.145731252687143,
-0.393659894693567));
#39085=CARTESIAN_POINT('Ctrl Pts',(0.0888405517426594,-0.116591533767489,
-0.391034016027105));
#39086=CARTESIAN_POINT('Ctrl Pts',(0.127082598372864,-0.087451814847836,
-0.388408137360644));
#39087=CARTESIAN_POINT('Ctrl Pts',(0.149595473891547,-0.0376696286223078,
-0.385782258694183));
#39088=CARTESIAN_POINT('Ctrl Pts',(0.146220151529374,0.0102906106195329,
-0.383156380027721));
#39089=CARTESIAN_POINT('Ctrl Pts',(0.142844829167201,0.0582508498613742,
-0.38053050136126));
#39090=CARTESIAN_POINT('Ctrl Pts',(0.113581308924171,0.104389142119528,
-0.377904622694799));
#39091=CARTESIAN_POINT('Ctrl Pts',(0.0716348734958325,0.127885395098236,
-0.375278744028337));
#39092=CARTESIAN_POINT('Ctrl Pts',(0.0296884380674942,0.151381648076943,
-0.372652865361876));
#39093=CARTESIAN_POINT('Ctrl Pts',(-0.0249409125461535,0.152235861776206,
-0.370026986695415));
#39094=CARTESIAN_POINT('Ctrl Pts',(-0.0676014613836439,0.130062568785149,
-0.367401108028953));
#39095=CARTESIAN_POINT('Ctrl Pts',(-0.110262010221135,0.107889275794091,
-0.364775229362492));
#39096=CARTESIAN_POINT('Ctrl Pts',(-0.140953757282468,0.062688476112713,
-0.362149350696031));
#39097=CARTESIAN_POINT('Ctrl Pts',(-0.145826926703387,0.0148572146932371,
-0.359523472029569));
#39098=CARTESIAN_POINT('Ctrl Pts',(-0.146326741907813,0.00995141527618409,
-0.35925414954781));
#39099=CARTESIAN_POINT('Ctrl Pts',(-0.146554958079519,0.00501794466540278,
-0.35898482706605));
#39100=CARTESIAN_POINT('Ctrl Pts',(-0.146521772955861,8.13712719715056E-5,
-0.358715504584291));
#39101=CARTESIAN_POINT('Origin',(0.,0.,-0.387));
#39102=CARTESIAN_POINT('',(-0.146127820803365,3.85940253507244E-5,-0.301584495415709));
#39103=CARTESIAN_POINT('',(-0.14612761578604,3.82095679274467E-5,-0.308715504584291));
#39104=CARTESIAN_POINT('',(-0.14635,-1.79227059055215E-17,-0.387));
#39105=CARTESIAN_POINT('Ctrl Pts',(-0.146127820803365,3.85940253507244E-5,
-0.301584495415709));
#39106=CARTESIAN_POINT('Ctrl Pts',(-0.146180003049472,0.0218050073068917,
-0.302763840936209));
#39107=CARTESIAN_POINT('Ctrl Pts',(-0.141618666722499,0.0435506356661818,
-0.303943186456708));
#39108=CARTESIAN_POINT('Ctrl Pts',(-0.132331368584888,0.0630447416204224,
-0.305122531977207));
#39109=CARTESIAN_POINT('Ctrl Pts',(-0.111652680596745,0.106449457250585,
-0.307748410643668));
#39110=CARTESIAN_POINT('Ctrl Pts',(-0.067544796154219,0.138692135847224,
-0.31037428931013));
#39111=CARTESIAN_POINT('Ctrl Pts',(-0.0199115777567349,0.145223137374079,
-0.313000167976591));
#39112=CARTESIAN_POINT('Ctrl Pts',(0.02772164064075,0.151754138900935,-0.315626046643052));
#39113=CARTESIAN_POINT('Ctrl Pts',(0.0788801929931927,0.132573463358006,
-0.318251925309514));
#39114=CARTESIAN_POINT('Ctrl Pts',(0.110478574190537,0.0963364687040155,
-0.320877803975975));
#39115=CARTESIAN_POINT('Ctrl Pts',(0.142076955387881,0.0600994740500249,
-0.323503682642436));
#39116=CARTESIAN_POINT('Ctrl Pts',(0.154115165430126,0.00680616028497251,
-0.326129561308898));
#39117=CARTESIAN_POINT('Ctrl Pts',(0.141160913005902,-0.0394946476990751,
-0.328755439975359));
#39118=CARTESIAN_POINT('Ctrl Pts',(0.128206660581679,-0.085795455683122,
-0.33138131864182));
#39119=CARTESIAN_POINT('Ctrl Pts',(0.0902599456909862,-0.125103757886164,
-0.334007197308282));
#39120=CARTESIAN_POINT('Ctrl Pts',(0.0444443779794659,-0.139681522842329,
-0.336633075974743));
#39121=CARTESIAN_POINT('Ctrl Pts',(-0.00137118973205505,-0.154259287798493,
-0.339258954641204));
#39122=CARTESIAN_POINT('Ctrl Pts',(-0.0550556102644042,-0.14410651550778,
-0.341884833307666));
#39123=CARTESIAN_POINT('Ctrl Pts',(-0.0923835702038583,-0.113804685817072,
-0.344510711974127));
#39124=CARTESIAN_POINT('Ctrl Pts',(-0.125902497068263,-0.086594926298794,
-0.346868639787988));
#39125=CARTESIAN_POINT('Ctrl Pts',(-0.146232752991076,-0.0431384191224556,
-0.349226567601849));
#39126=CARTESIAN_POINT('Ctrl Pts',(-0.146522325141606,8.10297640452141E-5,
-0.35158449541571));
#39127=CARTESIAN_POINT('Ctrl Pts',(-0.146521772955861,8.13712719715056E-5,
-0.358715504584291));
#39128=CARTESIAN_POINT('Ctrl Pts',(-0.146231405037506,-0.0431133612491548,
-0.356358948399589));
#39129=CARTESIAN_POINT('Ctrl Pts',(-0.12592776423548,-0.0865456474357522,
-0.354002392214887));
#39130=CARTESIAN_POINT('Ctrl Pts',(-0.0924424028114175,-0.113756896681685,
-0.351645836030186));
#39131=CARTESIAN_POINT('Ctrl Pts',(-0.0551301177180251,-0.144078023479557,
-0.349019957363724));
#39132=CARTESIAN_POINT('Ctrl Pts',(-0.00145095575073629,-0.154258553917727,
-0.346394078697263));
#39133=CARTESIAN_POINT('Ctrl Pts',(0.0443721426256257,-0.139704482172216,
-0.343768200030801));
#39134=CARTESIAN_POINT('Ctrl Pts',(0.090195241001987,-0.125150410426704,
-0.34114232136434));
#39135=CARTESIAN_POINT('Ctrl Pts',(0.128162275787421,-0.0858617364975109,
-0.338516442697879));
#39136=CARTESIAN_POINT('Ctrl Pts',(0.141140467901028,-0.0395676345119932,
-0.335890564031418));
#39137=CARTESIAN_POINT('Ctrl Pts',(0.154118660014635,0.00672646747352509,
-0.333264685364956));
#39138=CARTESIAN_POINT('Ctrl Pts',(0.142108009456413,0.0600259975153678,
-0.330638806698495));
#39139=CARTESIAN_POINT('Ctrl Pts',(0.110528371208319,0.0962793256012516,
-0.328012928032033));
#39140=CARTESIAN_POINT('Ctrl Pts',(0.0789487329602256,0.132532653687135,
-0.325387049365572));
#39141=CARTESIAN_POINT('Ctrl Pts',(0.0278001070222592,0.15173977981706,
-0.322761170699111));
#39142=CARTESIAN_POINT('Ctrl Pts',(-0.0198364808304775,0.145233410097187,
-0.32013529203265));
#39143=CARTESIAN_POINT('Ctrl Pts',(-0.0674730686832152,0.138727040377315,
-0.317509413366188));
#39144=CARTESIAN_POINT('Ctrl Pts',(-0.111597618450724,0.106507174807645,
-0.314883534699727));
#39145=CARTESIAN_POINT('Ctrl Pts',(-0.132298747337815,0.0631131589531134,
-0.312257656033265));
#39146=CARTESIAN_POINT('Ctrl Pts',(-0.141606937471067,0.0436011916385575,
-0.311076938883607));
#39147=CARTESIAN_POINT('Ctrl Pts',(-0.146179334127518,0.0218300125590762,
-0.309896221733949));
#39148=CARTESIAN_POINT('Ctrl Pts',(-0.14612761578604,3.82095679274467E-5,
-0.308715504584291));
#39149=CARTESIAN_POINT('Origin',(0.,0.,-0.387));
#39150=CARTESIAN_POINT('',(-0.146391321186674,-0.000125022356020285,-0.251584495415709));
#39151=CARTESIAN_POINT('',(-0.146392060940901,-0.000124923264760741,-0.258715504584291));
#39152=CARTESIAN_POINT('',(-0.14635,-1.79227059055215E-17,-0.387));
#39153=CARTESIAN_POINT('Ctrl Pts',(-0.146391321186674,-0.000125022356020285,
-0.251584495415709));
#39154=CARTESIAN_POINT('Ctrl Pts',(-0.146046214648355,0.038286396641969,
-0.253675235604107));
#39155=CARTESIAN_POINT('Ctrl Pts',(-0.130503182125338,0.0769451781813335,
-0.255765975792505));
#39156=CARTESIAN_POINT('Ctrl Pts',(-0.103359175644828,0.103938016950627,
-0.257856715980903));
#39157=CARTESIAN_POINT('Ctrl Pts',(-0.0692674850871064,0.13783984744341,
-0.260482594647365));
#39158=CARTESIAN_POINT('Ctrl Pts',(-0.0168761089937022,0.153339508863856,
-0.263108473313826));
#39159=CARTESIAN_POINT('Ctrl Pts',(0.0301731307904698,0.143442715868794,
-0.265734351980287));
#39160=CARTESIAN_POINT('Ctrl Pts',(0.0772223705746437,0.133545922873731,
-0.268360230646749));
#39161=CARTESIAN_POINT('Ctrl Pts',(0.118929474049585,0.0982526754631585,
-0.27098610931321));
#39162=CARTESIAN_POINT('Ctrl Pts',(0.136473940905855,0.0534891952748376,
-0.273611987979671));
#39163=CARTESIAN_POINT('Ctrl Pts',(0.154018407762125,0.00872571508651834,
-0.276237866646132));
#39164=CARTESIAN_POINT('Ctrl Pts',(0.147400237999727,-0.0455079978795489,
-0.278863745312594));
#39165=CARTESIAN_POINT('Ctrl Pts',(0.119605907678566,-0.0847387597615798,
-0.281489623979055));
#39166=CARTESIAN_POINT('Ctrl Pts',(0.0918115773574051,-0.123969521643612,
-0.284115502645516));
#39167=CARTESIAN_POINT('Ctrl Pts',(0.0428410864774815,-0.148197332441607,
-0.286741381311978));
#39168=CARTESIAN_POINT('Ctrl Pts',(-0.00520743150216466,-0.146489293856856,
-0.289367259978439));
#39169=CARTESIAN_POINT('Ctrl Pts',(-0.0532559494818108,-0.144781255272105,
-0.291993138644901));
#39170=CARTESIAN_POINT('Ctrl Pts',(-0.100382494561179,-0.117137367304608,
-0.294619017311362));
#39171=CARTESIAN_POINT('Ctrl Pts',(-0.125321021333984,-0.0760320469890165,
-0.297244895977823));
#39172=CARTESIAN_POINT('Ctrl Pts',(-0.139059053501684,-0.0533881186646286,
-0.298691429123785));
#39173=CARTESIAN_POINT('Ctrl Pts',(-0.146063816364198,-0.0266591274932147,
-0.300137962269747));
#39174=CARTESIAN_POINT('Ctrl Pts',(-0.146127820803365,3.85940253507244E-5,
-0.301584495415709));
#39175=CARTESIAN_POINT('Ctrl Pts',(-0.14612761578604,3.82095679274467E-5,
-0.308715504584291));
#39176=CARTESIAN_POINT('Ctrl Pts',(-0.146064314124979,-0.0266342877983396,
-0.307270343067488));
#39177=CARTESIAN_POINT('Ctrl Pts',(-0.139073622120044,-0.0533376818630241,
-0.305825181550685));
#39178=CARTESIAN_POINT('Ctrl Pts',(-0.125360316707312,-0.0759672322467926,
-0.304380020033882));
#39179=CARTESIAN_POINT('Ctrl Pts',(-0.100443049183043,-0.117085441452778,
-0.30175414136742));
#39180=CARTESIAN_POINT('Ctrl Pts',(-0.0533308061278312,-0.144753693725355,
-0.299128262700959));
#39181=CARTESIAN_POINT('Ctrl Pts',(-0.0052831791013535,-0.146486577537938,
-0.296502384034497));
#39182=CARTESIAN_POINT('Ctrl Pts',(0.0427644479251232,-0.14821946135052,
-0.293876505368036));
#39183=CARTESIAN_POINT('Ctrl Pts',(0.0917474589228652,-0.124016976703108,
-0.291250626701575));
#39184=CARTESIAN_POINT('Ctrl Pts',(0.119562070678756,-0.0848005933658808,
-0.288624748035114));
#39185=CARTESIAN_POINT('Ctrl Pts',(0.147376682434647,-0.045584210028653,
-0.285998869368652));
#39186=CARTESIAN_POINT('Ctrl Pts',(0.154022894948687,0.00864607199839097,
-0.283372990702191));
#39187=CARTESIAN_POINT('Ctrl Pts',(0.136501577754921,0.0534186170788067,
-0.280747112035729));
#39188=CARTESIAN_POINT('Ctrl Pts',(0.118980260561155,0.0981911621592217,
-0.278121233369268));
#39189=CARTESIAN_POINT('Ctrl Pts',(0.0772914136595841,0.133505970293009,
-0.275495354702807));
#39190=CARTESIAN_POINT('Ctrl Pts',(0.0302472990068507,0.143427090477993,
-0.272869476036346));
#39191=CARTESIAN_POINT('Ctrl Pts',(-0.0167968156458838,0.153348210662977,
-0.270243597369885));
#39192=CARTESIAN_POINT('Ctrl Pts',(-0.0691961980497802,0.137875642899156,
-0.267617718703423));
#39193=CARTESIAN_POINT('Ctrl Pts',(-0.103305413480267,0.103991446407277,
-0.264991840036961));
#39194=CARTESIAN_POINT('Ctrl Pts',(-0.130481190335898,0.0769949485056395,
-0.262899728219404));
#39195=CARTESIAN_POINT('Ctrl Pts',(-0.146046808768056,0.0383111911777933,
-0.260807616401848));
#39196=CARTESIAN_POINT('Ctrl Pts',(-0.146392060940901,-0.000124923264760741,
-0.258715504584291));
#39197=CARTESIAN_POINT('Origin',(0.,0.,-0.387));
#39198=CARTESIAN_POINT('',(-0.146474049564045,0.000104587793401157,-0.201584495415709));
#39199=CARTESIAN_POINT('',(-0.146473378794998,0.000104839022694492,-0.208715504584291));
#39200=CARTESIAN_POINT('',(-0.14635,-1.79227059055215E-17,-0.387));
#39201=CARTESIAN_POINT('Ctrl Pts',(-0.146474049564045,0.000104587793401157,
-0.201584495415709));
#39202=CARTESIAN_POINT('Ctrl Pts',(-0.146530019115592,0.00700710845801674,
-0.201960751605545));
#39203=CARTESIAN_POINT('Ctrl Pts',(-0.14608358854416,0.0139023584599612,
-0.20233700779538));
#39204=CARTESIAN_POINT('Ctrl Pts',(-0.145109674382301,0.0207222815519516,
-0.202713263985215));
#39205=CARTESIAN_POINT('Ctrl Pts',(-0.138312761827298,0.0683182840575807,
-0.205339142651677));
#39206=CARTESIAN_POINT('Ctrl Pts',(-0.105824260807261,0.11224541798416,
-0.207965021318138));
#39207=CARTESIAN_POINT('Ctrl Pts',(-0.0623047396710364,0.132681385187423,
-0.210590899984599));
#39208=CARTESIAN_POINT('Ctrl Pts',(-0.0187852185348116,0.153117352390686,
-0.213216778651061));
#39209=CARTESIAN_POINT('Ctrl Pts',(0.0357653227176007,0.150062152870633,
-0.215842657317522));
#39210=CARTESIAN_POINT('Ctrl Pts',(0.0767307301398749,0.124894457881073,
-0.218468535983983));
#39211=CARTESIAN_POINT('Ctrl Pts',(0.117696137562149,0.0997267628915141,
-0.221094414650445));
#39212=CARTESIAN_POINT('Ctrl Pts',(0.145076411154285,0.0524465724324491,
-0.223720293316906));
#39213=CARTESIAN_POINT('Ctrl Pts',(0.146516090957969,0.00438926499935377,
-0.226346171983367));
#39214=CARTESIAN_POINT('Ctrl Pts',(0.147955770761653,-0.043668042433743,
-0.228972050649829));
#39215=CARTESIAN_POINT('Ctrl Pts',(0.123454856776884,-0.0925024668408702,
-0.23159792931629));
#39216=CARTESIAN_POINT('Ctrl Pts',(0.08406948621946,-0.120077275305623,
-0.234223807982751));
#39217=CARTESIAN_POINT('Ctrl Pts',(0.0446841156620375,-0.147652083770375,
-0.236849686649213));
#39218=CARTESIAN_POINT('Ctrl Pts',(-0.00958571146803889,-0.153967276292754,
-0.239475565315674));
#39219=CARTESIAN_POINT('Ctrl Pts',(-0.0542505146411621,-0.136173096530155,
-0.242101443982135));
#39220=CARTESIAN_POINT('Ctrl Pts',(-0.0989153178142867,-0.118378916767556,
-0.244727322648597));
#39221=CARTESIAN_POINT('Ctrl Pts',(-0.133975097030458,-0.0764753647199769,
-0.247353201315058));
#39222=CARTESIAN_POINT('Ctrl Pts',(-0.143608984127524,-0.029371588913627,
-0.249979079981519));
#39223=CARTESIAN_POINT('Ctrl Pts',(-0.145572313105669,-0.0197721191369005,
-0.250514218459583));
#39224=CARTESIAN_POINT('Ctrl Pts',(-0.146479653437955,-0.00995667356591409,
-0.251049356937646));
#39225=CARTESIAN_POINT('Ctrl Pts',(-0.146391321186674,-0.000125022356020285,
-0.251584495415709));
#39226=CARTESIAN_POINT('Ctrl Pts',(-0.146392060940901,-0.000124923264760741,
-0.258715504584291));
#39227=CARTESIAN_POINT('Ctrl Pts',(-0.146480146177469,-0.00993124600428374,
-0.258181737735387));
#39228=CARTESIAN_POINT('Ctrl Pts',(-0.145577494117458,-0.019721448958086,
-0.257647970886482));
#39229=CARTESIAN_POINT('Ctrl Pts',(-0.143624148806805,-0.029297325128882,
-0.257114204037578));
#39230=CARTESIAN_POINT('Ctrl Pts',(-0.134014620245779,-0.0764060749532282,
-0.254488325371117));
#39231=CARTESIAN_POINT('Ctrl Pts',(-0.0989765146666498,-0.118327749381984,
-0.251862446704655));
#39232=CARTESIAN_POINT('Ctrl Pts',(-0.0543209199166082,-0.13614502208891,
-0.249236568038194));
#39233=CARTESIAN_POINT('Ctrl Pts',(-0.00966532516656721,-0.153962294795835,
-0.246610689371732));
#39234=CARTESIAN_POINT('Ctrl Pts',(0.0446077587543858,-0.14767516578093,
-0.243984810705271));
#39235=CARTESIAN_POINT('Ctrl Pts',(0.0840073816803498,-0.120120727618016,
-0.24135893203881));
#39236=CARTESIAN_POINT('Ctrl Pts',(0.123407004606315,-0.0925662894551019,
-0.238733053372349));
#39237=CARTESIAN_POINT('Ctrl Pts',(0.14793316653729,-0.0437445421441763,
-0.236107174705887));
#39238=CARTESIAN_POINT('Ctrl Pts',(0.146518337011597,0.0043135019958444,
-0.233481296039426));
#39239=CARTESIAN_POINT('Ctrl Pts',(0.145103507485905,0.0523715461358634,
-0.230855417372964));
#39240=CARTESIAN_POINT('Ctrl Pts',(0.117747686503548,0.0996658871049781,
-0.228229538706503));
#39241=CARTESIAN_POINT('Ctrl Pts',(0.076795299696999,0.124854760920646,
-0.225603660040042));
#39242=CARTESIAN_POINT('Ctrl Pts',(0.0358429128904488,0.150043634736315,
-0.222977781373581));
#39243=CARTESIAN_POINT('Ctrl Pts',(-0.0187060397402936,0.153127041398535,
-0.220351902707119));
#39244=CARTESIAN_POINT('Ctrl Pts',(-0.0622361211473401,0.132713581088084,
-0.217726024040658));
#39245=CARTESIAN_POINT('Ctrl Pts',(-0.105766202554386,0.112300120777634,
-0.215100145374196));
#39246=CARTESIAN_POINT('Ctrl Pts',(-0.138277412737736,0.0683897934945145,
-0.212474266707735));
#39247=CARTESIAN_POINT('Ctrl Pts',(-0.145098935695872,0.0207973132741649,
-0.209848388041274));
#39248=CARTESIAN_POINT('Ctrl Pts',(-0.146079939452749,0.0139530349243349,
-0.20947076022228));
#39249=CARTESIAN_POINT('Ctrl Pts',(-0.146529646082409,0.00703260472180356,
-0.209093132403285));
#39250=CARTESIAN_POINT('Ctrl Pts',(-0.146473378794998,0.000104839022694492,
-0.208715504584291));
#39251=CARTESIAN_POINT('Origin',(0.,0.,-0.387));
#39252=CARTESIAN_POINT('',(-0.146118283015211,7.41336224649447E-6,-0.151584495415709));
#39253=CARTESIAN_POINT('',(-0.146118240456221,7.01092482352256E-6,-0.158715504584291));
#39254=CARTESIAN_POINT('',(-0.14635,-1.79227059055215E-17,-0.387));
#39255=CARTESIAN_POINT('Ctrl Pts',(-0.146118283015211,7.41336224649447E-6,
-0.151584495415709));
#39256=CARTESIAN_POINT('Ctrl Pts',(-0.14612918343829,0.0237766293842829,
-0.152872146273443));
#39257=CARTESIAN_POINT('Ctrl Pts',(-0.14064821628497,0.0475411064603244,
-0.154159797131177));
#39258=CARTESIAN_POINT('Ctrl Pts',(-0.129647667122561,0.0683938057602947,
-0.155447447988912));
#39259=CARTESIAN_POINT('Ctrl Pts',(-0.107214484096722,0.110918266409727,
-0.158073326655373));
#39260=CARTESIAN_POINT('Ctrl Pts',(-0.061827254568182,0.141333643007611,
-0.160699205321834));
#39261=CARTESIAN_POINT('Ctrl Pts',(-0.0139671480261764,0.14591487057081,
-0.163325083988295));
#39262=CARTESIAN_POINT('Ctrl Pts',(0.0338929585158298,0.150496098134008,
-0.165950962654757));
#39263=CARTESIAN_POINT('Ctrl Pts',(0.084225942071302,0.129243176662519,
-0.168576841321218));
#39264=CARTESIAN_POINT('Ctrl Pts',(0.114318837396064,0.0917465748018712,
-0.17120271998768));
#39265=CARTESIAN_POINT('Ctrl Pts',(0.144411732720825,0.0542499729412243,
-0.173828598654141));
#39266=CARTESIAN_POINT('Ctrl Pts',(0.154264539814876,0.000509690691419144,
-0.176454477320602));
#39267=CARTESIAN_POINT('Ctrl Pts',(0.139431140093356,-0.0452237513755338,
-0.179080355987063));
#39268=CARTESIAN_POINT('Ctrl Pts',(0.124597740371835,-0.0909571934424881,
-0.181706234653525));
#39269=CARTESIAN_POINT('Ctrl Pts',(0.0850781338347429,-0.128683795326589,
-0.184332113319986));
#39270=CARTESIAN_POINT('Ctrl Pts',(0.0387057034970471,-0.141379273920697,
-0.186957991986448));
#39271=CARTESIAN_POINT('Ctrl Pts',(-0.00766672684064738,-0.154074752514805,
-0.189583870652909));
#39272=CARTESIAN_POINT('Ctrl Pts',(-0.0608919809789443,-0.141739107818921,
-0.19220974931937));
#39273=CARTESIAN_POINT('Ctrl Pts',(-0.0969519460031083,-0.10993884992864,
-0.194835627985831));
#39274=CARTESIAN_POINT('Ctrl Pts',(-0.127844960543657,-0.0826951787620337,
-0.197085250462457));
#39275=CARTESIAN_POINT('Ctrl Pts',(-0.146139409591153,-0.0411653395911477,
-0.199334872939083));
#39276=CARTESIAN_POINT('Ctrl Pts',(-0.146474049564045,0.000104587793401157,
-0.201584495415709));
#39277=CARTESIAN_POINT('Ctrl Pts',(-0.146473378794998,0.000104839022694492,
-0.208715504584291));
#39278=CARTESIAN_POINT('Ctrl Pts',(-0.146138384998877,-0.0411404144269961,
-0.206467253736824));
#39279=CARTESIAN_POINT('Ctrl Pts',(-0.127868873563498,-0.0826456784984334,
-0.204219002889357));
#39280=CARTESIAN_POINT('Ctrl Pts',(-0.0970087788541284,-0.109888699169191,
-0.20197075204189));
#39281=CARTESIAN_POINT('Ctrl Pts',(-0.0609652633213293,-0.141707598234614,
-0.199344873375428));
#39282=CARTESIAN_POINT('Ctrl Pts',(-0.00774639652281044,-0.154070763207882,
-0.196718994708967));
#39283=CARTESIAN_POINT('Ctrl Pts',(0.0386325911211531,-0.141399265509641,
-0.194093116042506));
#39284=CARTESIAN_POINT('Ctrl Pts',(0.085011578765118,-0.128727767811399,
-0.191467237376045));
#39285=CARTESIAN_POINT('Ctrl Pts',(0.124550687254527,-0.091021607441645,
-0.188841358709583));
#39286=CARTESIAN_POINT('Ctrl Pts',(0.139407732894378,-0.0452958428992574,
-0.186215480043122));
#39287=CARTESIAN_POINT('Ctrl Pts',(0.154264778534229,0.000429921643130132,
-0.183589601376661));
#39288=CARTESIAN_POINT('Ctrl Pts',(0.144439761324521,0.0541752903581515,
-0.180963722710199));
#39289=CARTESIAN_POINT('Ctrl Pts',(0.11436626020644,0.0916874468314653,
-0.178337844043738));
#39290=CARTESIAN_POINT('Ctrl Pts',(0.0842927590883588,0.129199603304779,
-0.175711965377277));
#39291=CARTESIAN_POINT('Ctrl Pts',(0.0339707740619053,0.150478547536385,
-0.173086086710815));
#39292=CARTESIAN_POINT('Ctrl Pts',(-0.0138916940039819,0.145922069057284,
-0.170460208044354));
#39293=CARTESIAN_POINT('Ctrl Pts',(-0.0617541620698691,0.141365590578183,
-0.167834329377893));
#39294=CARTESIAN_POINT('Ctrl Pts',(-0.10715711317519,0.110973689388375,
-0.165208450711431));
#39295=CARTESIAN_POINT('Ctrl Pts',(-0.129612281041003,0.0684608350966334,
-0.16258257204497));
#39296=CARTESIAN_POINT('Ctrl Pts',(-0.140635340368035,0.0475916205879853,
-0.161293549558077));
#39297=CARTESIAN_POINT('Ctrl Pts',(-0.146128561593049,0.0238015614994364,
-0.160004527071184));
#39298=CARTESIAN_POINT('Ctrl Pts',(-0.146118240456221,7.01092482352256E-6,
-0.158715504584291));
#39299=CARTESIAN_POINT('Origin',(0.,0.,-0.387));
#39300=CARTESIAN_POINT('',(-0.146448857461917,-0.000112937673885413,-0.101584495415709));
#39301=CARTESIAN_POINT('',(-0.146449480434,-0.000112796118272305,-0.108715504584291));
#39302=CARTESIAN_POINT('',(-0.14635,-1.79227059055215E-17,-0.387));
#39303=CARTESIAN_POINT('Ctrl Pts',(-0.146448857461917,-0.000112937673885413,
-0.101584495415709));
#39304=CARTESIAN_POINT('Ctrl Pts',(-0.146104431800015,0.0402472859926994,
-0.103783540941342));
#39305=CARTESIAN_POINT('Ctrl Pts',(-0.128715625084515,0.0808682927490122,
-0.105982586466975));
#39306=CARTESIAN_POINT('Ctrl Pts',(-0.0990303696629292,0.10807035631605,
-0.108181631992607));
#39307=CARTESIAN_POINT('Ctrl Pts',(-0.0635832277045705,0.140552320682775,
-0.110807510659069));
#39308=CARTESIAN_POINT('Ctrl Pts',(-0.0106029105929107,0.153900575233485,
-0.11343338932553));
#39309=CARTESIAN_POINT('Ctrl Pts',(0.0360031244180305,0.142091552039598,
-0.116059267991992));
#39310=CARTESIAN_POINT('Ctrl Pts',(0.082609159428971,0.130282528845712,
-0.118685146658453));
#39311=CARTESIAN_POINT('Ctrl Pts',(0.122840912339193,0.0933162279072309,
-0.121311025324914));
#39312=CARTESIAN_POINT('Ctrl Pts',(0.138543574148993,0.0478739029189084,
-0.123936903991376));
#39313=CARTESIAN_POINT('Ctrl Pts',(0.154246235958793,0.00243157793058653,
-0.126562782657837));
#39314=CARTESIAN_POINT('Ctrl Pts',(0.145419806668172,-0.0514867711075763,
-0.129188661324298));
#39315=CARTESIAN_POINT('Ctrl Pts',(0.116047283516059,-0.0895503010832982,
-0.13181453999076));
#39316=CARTESIAN_POINT('Ctrl Pts',(0.0866747603639465,-0.127613831059021,
-0.134440418657221));
#39317=CARTESIAN_POINT('Ctrl Pts',(0.0367561433503418,-0.149822541972302,
-0.137066297323682));
#39318=CARTESIAN_POINT('Ctrl Pts',(-0.011182606745029,-0.146154645996528,
-0.139692175990144));
#39319=CARTESIAN_POINT('Ctrl Pts',(-0.0591213568403991,-0.142486750020755,
-0.142318054656605));
#39320=CARTESIAN_POINT('Ctrl Pts',(-0.105080240017535,-0.112942247155927,
-0.144943933323066));
#39321=CARTESIAN_POINT('Ctrl Pts',(-0.128320113344536,-0.070853223373023,
-0.147569811989528));
#39322=CARTESIAN_POINT('Ctrl Pts',(-0.140163861174438,-0.0494033739234423,
-0.148908039798255));
#39323=CARTESIAN_POINT('Ctrl Pts',(-0.14610695444023,-0.0246954210134512,
-0.150246267606982));
#39324=CARTESIAN_POINT('Ctrl Pts',(-0.146118283015211,7.41336224649447E-6,
-0.151584495415709));
#39325=CARTESIAN_POINT('Ctrl Pts',(-0.146118240456221,7.01092482352256E-6,
-0.158715504584291));
#39326=CARTESIAN_POINT('Ctrl Pts',(-0.146107536317474,-0.0246705197615437,
-0.157378648404722));
#39327=CARTESIAN_POINT('Ctrl Pts',(-0.140177254795957,-0.0493528814635679,
-0.156041792225154));
#39328=CARTESIAN_POINT('Ctrl Pts',(-0.128356728993014,-0.0707868597717533,
-0.154704936045586));
#39329=CARTESIAN_POINT('Ctrl Pts',(-0.105138624452908,-0.11288789295472,
-0.152079057379125));
#39330=CARTESIAN_POINT('Ctrl Pts',(-0.0591950307463908,-0.142456151926979,
-0.149453178712664));
#39331=CARTESIAN_POINT('Ctrl Pts',(-0.0112581828339444,-0.146148837901321,
-0.146827300046202));
#39332=CARTESIAN_POINT('Ctrl Pts',(0.0366786650785026,-0.149841523875664,
-0.144201421379741));
#39333=CARTESIAN_POINT('Ctrl Pts',(0.0866087671968788,-0.12765863685209,
-0.141575542713279));
#39334=CARTESIAN_POINT('Ctrl Pts',(0.116000963822744,-0.0896102977953412,
-0.138949664046818));
#39335=CARTESIAN_POINT('Ctrl Pts',(0.145393160448608,-0.0515619587385927,
-0.136323785380357));
#39336=CARTESIAN_POINT('Ctrl Pts',(0.154247451581962,0.00235183235133025,
-0.133697906713896));
#39337=CARTESIAN_POINT('Ctrl Pts',(0.138568298030551,0.0478022630729415,
-0.131072028047434));
#39338=CARTESIAN_POINT('Ctrl Pts',(0.122889144479139,0.0932526937945534,
-0.128446149380973));
#39339=CARTESIAN_POINT('Ctrl Pts',(0.0826765462429627,0.130239764147853,
-0.125820270714511));
#39340=CARTESIAN_POINT('Ctrl Pts',(0.0360766101420983,0.142072897713786,
-0.12319439204805));
#39341=CARTESIAN_POINT('Ctrl Pts',(-0.0105233259587662,0.153906031279718,
-0.120568513381589));
#39342=CARTESIAN_POINT('Ctrl Pts',(-0.0635105999243186,0.140585228058283,
-0.117942634715127));
#39343=CARTESIAN_POINT('Ctrl Pts',(-0.0989745039313167,0.108121574286461,
-0.115316756048666));
#39344=CARTESIAN_POINT('Ctrl Pts',(-0.128692321342145,0.0809178875437671,
-0.113116338893874));
#39345=CARTESIAN_POINT('Ctrl Pts',(-0.146105230934553,0.0402720939482578,
-0.110915921739083));
#39346=CARTESIAN_POINT('Ctrl Pts',(-0.146449480434,-0.000112796118272305,
-0.108715504584291));
#39347=CARTESIAN_POINT('Origin',(0.,0.,-0.387));
#39348=CARTESIAN_POINT('',(-0.146419470807316,0.000121292426834327,-0.0515844954157089));
#39349=CARTESIAN_POINT('',(-0.146417921947427,0.000120753153388515,-0.0587155045842908));
#39350=CARTESIAN_POINT('',(-0.14635,-1.79227059055215E-17,-0.387));
#39351=CARTESIAN_POINT('Ctrl Pts',(-0.146419470807316,0.000121292426834327,
-0.0515844954157089));
#39352=CARTESIAN_POINT('Ctrl Pts',(-0.146499213746489,0.00902035961397621,
-0.0520690569427793));
#39353=CARTESIAN_POINT('Ctrl Pts',(-0.145757375492163,0.017906185955658,
-0.0525536184698496));
#39354=CARTESIAN_POINT('Ctrl Pts',(-0.144146186685956,0.0266311864910578,
-0.0530381799969199));
#39355=CARTESIAN_POINT('Ctrl Pts',(-0.135415022370369,0.0739126801525337,
-0.0556640586633812));
#39356=CARTESIAN_POINT('Ctrl Pts',(-0.101154118446619,0.116471290797761,
-0.0582899373298425));
#39357=CARTESIAN_POINT('Ctrl Pts',(-0.0568351738065945,0.135112443908202,
-0.0609158159963038));
#39358=CARTESIAN_POINT('Ctrl Pts',(-0.0125162291665695,0.153753597018643,
-0.0635416946627651));
#39359=CARTESIAN_POINT('Ctrl Pts',(0.0418607561897289,0.148477292594297,
-0.0661675733292264));
#39360=CARTESIAN_POINT('Ctrl Pts',(0.0817639052896394,0.121659133496513,
-0.0687934519956878));
#39361=CARTESIAN_POINT('Ctrl Pts',(0.121667054389549,0.0948409743987301,
-0.0714193306621491));
#39362=CARTESIAN_POINT('Ctrl Pts',(0.147096367233071,0.0464809606275097,
-0.0740452093286105));
#39363=CARTESIAN_POINT('Ctrl Pts',(0.146573626794785,-0.00159543872172704,
-0.0766710879950718));
#39364=CARTESIAN_POINT('Ctrl Pts',(0.146050886356499,-0.0496718380709638,
-0.0792969666615331));
#39365=CARTESIAN_POINT('Ctrl Pts',(0.119576092636403,-0.0974646229982186,
-0.0819228453279944));
#39366=CARTESIAN_POINT('Ctrl Pts',(0.0790977545786269,-0.123408586620134,
-0.0845487239944557));
#39367=CARTESIAN_POINT('Ctrl Pts',(0.0386194165208501,-0.14935255024205,
-0.0871746026609171));
#39368=CARTESIAN_POINT('Ctrl Pts',(-0.0158624658746058,-0.153447692558627,
-0.0898004813273783));
#39369=CARTESIAN_POINT('Ctrl Pts',(-0.0597635898992248,-0.13384528397374,
-0.0924263599938397));
#39370=CARTESIAN_POINT('Ctrl Pts',(-0.103664713923843,-0.114242875388853,
-0.095052238660301));
#39371=CARTESIAN_POINT('Ctrl Pts',(-0.136985079577624,-0.0709429159024997,
-0.0976781173267624));
#39372=CARTESIAN_POINT('Ctrl Pts',(-0.144688279001984,-0.0234850990679547,
-0.100303995993224));
#39373=CARTESIAN_POINT('Ctrl Pts',(-0.145940423987479,-0.0157708930480517,
-0.100730829134052));
#39374=CARTESIAN_POINT('Ctrl Pts',(-0.146515710232966,-0.00794682780091699,
-0.101157662274881));
#39375=CARTESIAN_POINT('Ctrl Pts',(-0.146448857461917,-0.000112937673885413,
-0.101584495415709));
#39376=CARTESIAN_POINT('Ctrl Pts',(-0.146449480434,-0.000112796118272305,
-0.108715504584291));
#39377=CARTESIAN_POINT('Ctrl Pts',(-0.146516042772921,-0.00792141383373452,
-0.108290043072621));
#39378=CARTESIAN_POINT('Ctrl Pts',(-0.145944473964313,-0.0157202773759087,
-0.107864581560952));
#39379=CARTESIAN_POINT('Ctrl Pts',(-0.144700337830555,-0.0234103305235109,
-0.107439120049282));
#39380=CARTESIAN_POINT('Ctrl Pts',(-0.137021733674351,-0.0708720772394546,
-0.104813241382821));
#39381=CARTESIAN_POINT('Ctrl Pts',(-0.103723991313499,-0.114189066349136,
-0.10218736271636));
#39382=CARTESIAN_POINT('Ctrl Pts',(-0.0598329080582324,-0.13381425959949,
-0.0995614840498983));
#39383=CARTESIAN_POINT('Ctrl Pts',(-0.0159418248029649,-0.153439452849846,
-0.096935605383437));
#39384=CARTESIAN_POINT('Ctrl Pts',(0.0385425993467187,-0.149372850240874,
-0.0943097267169755));
#39385=CARTESIAN_POINT('Ctrl Pts',(0.0790341514413548,-0.123449656692746,
-0.0916838480505142));
#39386=CARTESIAN_POINT('Ctrl Pts',(0.11952570353599,-0.0975264631446175,
-0.0890579693840529));
#39387=CARTESIAN_POINT('Ctrl Pts',(0.146024383575578,-0.0497466786573349,
-0.0864320907175918));
#39388=CARTESIAN_POINT('Ctrl Pts',(0.146572354104826,-0.00167087112836006,
-0.0838062120511305));
#39389=CARTESIAN_POINT('Ctrl Pts',(0.147120324634074,0.0464049364006154,
-0.0811803333846691));
#39390=CARTESIAN_POINT('Ctrl Pts',(0.121717585652978,0.0947767669712817,
-0.0785544547182077));
#39391=CARTESIAN_POINT('Ctrl Pts',(0.081827606874047,0.12161615159699,-0.0759285760517464));
#39392=CARTESIAN_POINT('Ctrl Pts',(0.0419376280951157,0.148455536222698,
-0.0733026973852851));
#39393=CARTESIAN_POINT('Ctrl Pts',(-0.0124395904816524,0.153762474903448,
-0.0706768187188237));
#39394=CARTESIAN_POINT('Ctrl Pts',(-0.056766830003724,0.135143108409308,
-0.0680509400523624));
#39395=CARTESIAN_POINT('Ctrl Pts',(-0.101094069525796,0.116523741915167,
-0.0654250613859011));
#39396=CARTESIAN_POINT('Ctrl Pts',(-0.135371329993171,0.0739780702461364,
-0.0627991827194396));
#39397=CARTESIAN_POINT('Ctrl Pts',(-0.144129485340515,0.0267032560390048,
-0.0601733040529783));
#39398=CARTESIAN_POINT('Ctrl Pts',(-0.14575022971269,0.017954794058933,
-0.0596873708967491));
#39399=CARTESIAN_POINT('Ctrl Pts',(-0.146497059078279,0.00904438013685962,
-0.05920143774052));
#39400=CARTESIAN_POINT('Ctrl Pts',(-0.146417921947427,0.000120753153388515,
-0.0587155045842908));
#39401=CARTESIAN_POINT('Origin',(0.,0.,-0.860086711473615));
#39402=CARTESIAN_POINT('',(-0.11783090655505,9.76099458120806E-5,-0.0350867114736151));
#39403=CARTESIAN_POINT('',(-0.117565879451543,-5.36239120088947E-5,-0.0252132885263834));
#39404=CARTESIAN_POINT('',(-0.117775,-1.1488940921122E-14,-0.860086711473615));
#39405=CARTESIAN_POINT('',(0.106341965058147,-0.0510185301167581,-0.01365));
#39406=CARTESIAN_POINT('Ctrl Pts',(-0.11783090655505,9.76099458120895E-5,
-0.0350867114736151));
#39407=CARTESIAN_POINT('Ctrl Pts',(-0.117547320619057,-0.0315497098533478,
-0.0329453943342242));
#39408=CARTESIAN_POINT('Ctrl Pts',(-0.0881713273287959,-0.102469121142594,
-0.0281781985283719));
#39409=CARTESIAN_POINT('Ctrl Pts',(0.0271354482247726,-0.134172264119296,
-0.0210326280371669));
#39410=CARTESIAN_POINT('Ctrl Pts',(0.090961439762511,-0.0825484450221484,
-0.0160283746853528));
#39411=CARTESIAN_POINT('Ctrl Pts',(0.106341965058147,-0.0510185301167582,
-0.01365));
#39412=CARTESIAN_POINT('',(-0.0138313775859342,-0.116960008631478,-0.0136500000000001));
#39413=CARTESIAN_POINT('Origin',(0.,0.,-0.0136499999999999));
#39414=CARTESIAN_POINT('Ctrl Pts',(-0.117565879451543,-5.36239120088964E-5,
-0.0252132885263835));
#39415=CARTESIAN_POINT('Ctrl Pts',(-0.117583343244632,-0.0183158611289637,
-0.0239847376840503));
#39416=CARTESIAN_POINT('Ctrl Pts',(-0.10502991826055,-0.075546691227487,
-0.0201303081752559));
#39417=CARTESIAN_POINT('Ctrl Pts',(-0.0524255658063026,-0.112395963227031,
-0.0162758786664614));
#39418=CARTESIAN_POINT('Ctrl Pts',(-0.0138313775859342,-0.116960008631478,
-0.0136500000000001));
#39419=CARTESIAN_POINT('Origin',(0.,0.,-0.860086711473615));
#39420=CARTESIAN_POINT('',(-0.117854555432711,-9.08864676626378E-5,-0.0850867114736154));
#39421=CARTESIAN_POINT('',(-0.117829660111775,9.71759660986608E-5,-0.0752132885263837));
#39422=CARTESIAN_POINT('',(-0.117775,-1.1488940921122E-14,-0.860086711473615));
#39423=CARTESIAN_POINT('Ctrl Pts',(-0.117854555432711,-9.08864676626335E-5,
-0.0850867114736154));
#39424=CARTESIAN_POINT('Ctrl Pts',(-0.117908355125983,-0.00639520084901597,
-0.084659878332787));
#39425=CARTESIAN_POINT('Ctrl Pts',(-0.114597257003647,-0.0514271270458079,
-0.0816071665254972));
#39426=CARTESIAN_POINT('Ctrl Pts',(-0.0566095361633514,-0.126782421437836,
-0.0759285760517461));
#39427=CARTESIAN_POINT('Ctrl Pts',(0.0749231669276979,-0.116895737741183,
-0.0680509400523622));
#39428=CARTESIAN_POINT('Ctrl Pts',(0.138839849477423,-0.00151216593098895,
-0.0601733040529782));
#39429=CARTESIAN_POINT('Ctrl Pts',(0.0774472156514042,0.115240836226281,
-0.0522956680535942));
#39430=CARTESIAN_POINT('Ctrl Pts',(-0.0538322401122725,0.127979136607092,
-0.0444180320542103));
#39431=CARTESIAN_POINT('Ctrl Pts',(-0.114062929272019,0.053161074172187,
-0.0386817131942172));
#39432=CARTESIAN_POINT('Ctrl Pts',(-0.117895079596807,0.0072591243835695,
-0.0355712730006855));
#39433=CARTESIAN_POINT('Ctrl Pts',(-0.11783090655505,9.76099458120895E-5,
-0.0350867114736151));
#39434=CARTESIAN_POINT('Ctrl Pts',(-0.117829660111775,9.71759660986617E-5,
-0.0752132885263837));
#39435=CARTESIAN_POINT('Ctrl Pts',(-0.117549202734137,-0.0315276377698398,
-0.0730733430161518));
#39436=CARTESIAN_POINT('Ctrl Pts',(-0.0882161036909192,-0.102417796622243,
-0.0683075188394586));
#39437=CARTESIAN_POINT('Ctrl Pts',(0.0310918033177442,-0.135313955894808,
-0.0609158159963039));
#39438=CARTESIAN_POINT('Ctrl Pts',(0.13019812432102,-0.0482707014283373,
-0.0530381799969201));
#39439=CARTESIAN_POINT('Ctrl Pts',(0.111769783231296,0.0823751383704014,
-0.045160543997536));
#39440=CARTESIAN_POINT('Ctrl Pts',(-0.00747498868383688,0.138604580907157,
-0.037282907998152));
#39441=CARTESIAN_POINT('Ctrl Pts',(-0.102520577346041,0.0805987077592062,
-0.0306338228411012));
#39442=CARTESIAN_POINT('Ctrl Pts',(-0.117546016501506,0.0207174596400722,
-0.0266106163505116));
#39443=CARTESIAN_POINT('Ctrl Pts',(-0.117565879451543,-5.36239120088964E-5,
-0.0252132885263835));
#39444=CARTESIAN_POINT('Origin',(0.,0.,-0.860086711473615));
#39445=CARTESIAN_POINT('',(-0.117588526013778,5.9658950325018E-6,-0.135086711473615));
#39446=CARTESIAN_POINT('',(-0.117855056768803,-9.0772550948498E-5,-0.125213288526384));
#39447=CARTESIAN_POINT('',(-0.117775,-1.1488940921122E-14,-0.860086711473615));
#39448=CARTESIAN_POINT('Ctrl Pts',(-0.117588526013778,5.96589503251525E-6,
-0.135086711473615));
#39449=CARTESIAN_POINT('Ctrl Pts',(-0.11757940935564,-0.0198736126399706,
-0.133748483664888));
#39450=CARTESIAN_POINT('Ctrl Pts',(-0.103412073402492,-0.0787732216373988,
-0.1297843771897));
#39451=CARTESIAN_POINT('Ctrl Pts',(-0.01059248606553,-0.138441959744445,
-0.12319439204805));
#39452=CARTESIAN_POINT('Ctrl Pts',(0.10992336877787,-0.0848246534005071,
-0.115316756048666));
#39453=CARTESIAN_POINT('Ctrl Pts',(0.131232546291422,0.045347541159856,
-0.107439120049282));
#39454=CARTESIAN_POINT('Ctrl Pts',(0.034103170842127,0.134593310063775,
-0.099561484049898));
#39455=CARTESIAN_POINT('Ctrl Pts',(-0.0868739814205058,0.104113427887564,
-0.0921106811913426));
#39456=CARTESIAN_POINT('Ctrl Pts',(-0.117577379263731,0.0323889587139717,
-0.0872857569992483));
#39457=CARTESIAN_POINT('Ctrl Pts',(-0.117854555432711,-9.08864676626335E-5,
-0.0850867114736154));
#39458=CARTESIAN_POINT('Ctrl Pts',(-0.117855056768803,-9.07725509484815E-5,
-0.125213288526384));
#39459=CARTESIAN_POINT('Ctrl Pts',(-0.117908622737142,-0.00637474898714989,
-0.124787827014714));
#39460=CARTESIAN_POINT('Ctrl Pts',(-0.114609797901413,-0.0513861008242438,
-0.121736486836584));
#39461=CARTESIAN_POINT('Ctrl Pts',(-0.0566754456467214,-0.126752823243337,
-0.116059267991992));
#39462=CARTESIAN_POINT('Ctrl Pts',(0.0748633938659991,-0.116935041440705,
-0.108181631992608));
#39463=CARTESIAN_POINT('Ctrl Pts',(0.138837743882996,-0.00158285589939853,
-0.100303995993224));
#39464=CARTESIAN_POINT('Ctrl Pts',(0.077509265915822,0.115198674926568,
-0.0924263599938399));
#39465=CARTESIAN_POINT('Ctrl Pts',(-0.0537707528995959,0.128010933958857,
-0.0845487239944558));
#39466=CARTESIAN_POINT('Ctrl Pts',(-0.11404460569689,0.0531977337096131,
-0.0788110335053037));
#39467=CARTESIAN_POINT('Ctrl Pts',(-0.117893345629958,0.00727845487268427,
-0.0756992216826131));
#39468=CARTESIAN_POINT('Ctrl Pts',(-0.117829660111775,9.71759660986617E-5,
-0.0752132885263837));
#39469=CARTESIAN_POINT('Origin',(0.,0.,-0.860086711473615));
#39470=CARTESIAN_POINT('',(-0.117874828748926,8.41669106047294E-5,-0.185086711473615));
#39471=CARTESIAN_POINT('',(-0.117588491764479,5.64203395312518E-6,-0.175213288526384));
#39472=CARTESIAN_POINT('',(-0.117775,-1.1488940921122E-14,-0.860086711473615));
#39473=CARTESIAN_POINT('Ctrl Pts',(-0.117874828748926,8.41669106047436E-5,
-0.185086711473615));
#39474=CARTESIAN_POINT('Ctrl Pts',(-0.117605527602309,-0.0331277613279678,
-0.18283708899699));
#39475=CARTESIAN_POINT('Ctrl Pts',(-0.085698280103056,-0.105559724356163,
-0.177961587853902));
#39476=CARTESIAN_POINT('Ctrl Pts',(0.0366631742567891,-0.133918582381201,
-0.170460208044354));
#39477=CARTESIAN_POINT('Ctrl Pts',(0.132073252696953,-0.042837259451921,
-0.16258257204497));
#39478=CARTESIAN_POINT('Ctrl Pts',(0.108286145990386,0.0869050379577989,
-0.154704936045586));
#39479=CARTESIAN_POINT('Ctrl Pts',(-0.0132300918964409,0.138214832825673,
-0.146827300046202));
#39480=CARTESIAN_POINT('Ctrl Pts',(-0.104191641877288,0.0772587042552975,
-0.140287891855545));
#39481=CARTESIAN_POINT('Ctrl Pts',(-0.117597298117148,0.0191342160965729,
-0.13637436233135));
#39482=CARTESIAN_POINT('Ctrl Pts',(-0.117588526013778,5.96589503251525E-6,
-0.135086711473615));
#39483=CARTESIAN_POINT('Ctrl Pts',(-0.117588491764479,5.64203395314773E-6,
-0.175213288526384));
#39484=CARTESIAN_POINT('Ctrl Pts',(-0.117579877620705,-0.019853573385154,
-0.173876432346816));
#39485=CARTESIAN_POINT('Ctrl Pts',(-0.103433474728503,-0.0787321665347216,
-0.169913697500786));
#39486=CARTESIAN_POINT('Ctrl Pts',(-0.0106640792440769,-0.138436453663531,
-0.163325083988296));
#39487=CARTESIAN_POINT('Ctrl Pts',(0.10987950347526,-0.0848814925592979,
-0.155447447988912));
#39488=CARTESIAN_POINT('Ctrl Pts',(0.13125594634982,0.04527969798971,-0.147569811989528));
#39489=CARTESIAN_POINT('Ctrl Pts',(0.0341728150085339,0.134575609384171,
-0.139692175990144));
#39490=CARTESIAN_POINT('Ctrl Pts',(-0.0868424965679614,0.104152811009239,
-0.132240001502429));
#39491=CARTESIAN_POINT('Ctrl Pts',(-0.117578022366365,0.0324089228886563,
-0.127413705681176));
#39492=CARTESIAN_POINT('Ctrl Pts',(-0.117855056768803,-9.07725509484815E-5,
-0.125213288526384));
#39493=CARTESIAN_POINT('Origin',(0.,0.,-0.860086711473615));
#39494=CARTESIAN_POINT('',(-0.117808253179095,-0.000100611602195776,-0.235086711473615));
#39495=CARTESIAN_POINT('',(-0.117874288948281,8.43690870912656E-5,-0.225213288526384));
#39496=CARTESIAN_POINT('',(-0.117775,-1.1488940921122E-14,-0.860086711473615));
#39497=CARTESIAN_POINT('Ctrl Pts',(-0.117808253179095,-0.000100611602195775,
-0.235086711473615));
#39498=CARTESIAN_POINT('Ctrl Pts',(-0.117879338460233,-0.00801262199676357,
-0.234551572995552));
#39499=CARTESIAN_POINT('Ctrl Pts',(-0.113566221109939,-0.0546711547288069,
-0.231390555851028));
#39500=CARTESIAN_POINT('Ctrl Pts',(-0.0513876737847133,-0.128987138809037,
-0.225603660040042));
#39501=CARTESIAN_POINT('Ctrl Pts',(0.0796330755882605,-0.113740706298137,
-0.217726024040658));
#39502=CARTESIAN_POINT('Ctrl Pts',(0.138784325562075,0.004157640156581,
-0.209848388041274));
#39503=CARTESIAN_POINT('Ctrl Pts',(0.0726815912474743,0.118303682479431,
-0.20197075204189));
#39504=CARTESIAN_POINT('Ctrl Pts',(-0.0590168712602702,0.125679687743678,
-0.194093116042506));
#39505=CARTESIAN_POINT('Ctrl Pts',(-0.11505331136728,0.0499137972881179,
-0.188465102519748));
#39506=CARTESIAN_POINT('Ctrl Pts',(-0.117919870183388,0.00563896275122834,
-0.185462967663451));
#39507=CARTESIAN_POINT('Ctrl Pts',(-0.117874828748926,8.41669106047436E-5,
-0.185086711473615));
#39508=CARTESIAN_POINT('Ctrl Pts',(-0.117874288948281,8.4369087091269E-5,
-0.225213288526384));
#39509=CARTESIAN_POINT('Ctrl Pts',(-0.11760470306281,-0.0331077028297975,
-0.222965037678917));
#39510=CARTESIAN_POINT('Ctrl Pts',(-0.0857304791730737,-0.105520590514,
-0.218090908164989));
#39511=CARTESIAN_POINT('Ctrl Pts',(0.0365939199639361,-0.133937518903554,
-0.210590899984599));
#39512=CARTESIAN_POINT('Ctrl Pts',(0.132051080927517,-0.0429055468321947,
-0.202713263985216));
#39513=CARTESIAN_POINT('Ctrl Pts',(0.108331065856659,0.0868490305592283,
-0.194835627985831));
#39514=CARTESIAN_POINT('Ctrl Pts',(-0.0131586188681242,0.138221650789034,
-0.186957991986448));
#39515=CARTESIAN_POINT('Ctrl Pts',(-0.104170762439501,0.0772997942322291,
-0.180417212166632));
#39516=CARTESIAN_POINT('Ctrl Pts',(-0.117596797687883,0.0191542801885525,
-0.176502311013277));
#39517=CARTESIAN_POINT('Ctrl Pts',(-0.117588491764479,5.64203395314773E-6,
-0.175213288526384));
#39518=CARTESIAN_POINT('Origin',(0.,0.,-0.860086711473615));
#39519=CARTESIAN_POINT('',(-0.117596201538205,3.10584990424738E-5,-0.285086711473616));
#39520=CARTESIAN_POINT('',(-0.117808848495488,-0.000100531858621397,-0.275213288526384));
#39521=CARTESIAN_POINT('',(-0.117775,-1.1488940921122E-14,-0.860086711473615));
#39522=CARTESIAN_POINT('Ctrl Pts',(-0.117596201538205,3.10584990424884E-5,
-0.285086711473616));
#39523=CARTESIAN_POINT('Ctrl Pts',(-0.117544694036852,-0.0214539032491567,
-0.283640178327653));
#39524=CARTESIAN_POINT('Ctrl Pts',(-0.10167468688571,-0.082011168264245,
-0.27956776651523));
#39525=CARTESIAN_POINT('Ctrl Pts',(-0.00493263138706642,-0.138758942569485,
-0.272869476036346));
#39526=CARTESIAN_POINT('Ctrl Pts',(0.113294213096355,-0.0802670310546098,
-0.264991840036961));
#39527=CARTESIAN_POINT('Ctrl Pts',(0.129272107399731,0.0506665298182005,
-0.257114204037578));
#39528=CARTESIAN_POINT('Ctrl Pts',(0.0285808717640413,0.1358731348154,-0.249236568038194));
#39529=CARTESIAN_POINT('Ctrl Pts',(-0.0893124882611786,0.100995120524423,
-0.241894070516873));
#39530=CARTESIAN_POINT('Ctrl Pts',(-0.117530529075574,0.0308109351862458,
-0.237177451662014));
#39531=CARTESIAN_POINT('Ctrl Pts',(-0.117808253179095,-0.000100611602195775,
-0.235086711473615));
#39532=CARTESIAN_POINT('Ctrl Pts',(-0.117808848495488,-0.000100531858621394,
-0.275213288526384));
#39533=CARTESIAN_POINT('Ctrl Pts',(-0.11787973499181,-0.00799215919477956,
-0.274679521677479));
#39534=CARTESIAN_POINT('Ctrl Pts',(-0.113579744177213,-0.0546300439782162,
-0.271519876162114));
#39535=CARTESIAN_POINT('Ctrl Pts',(-0.0514543637190464,-0.128960545878442,
-0.265734351980287));
#39536=CARTESIAN_POINT('Ctrl Pts',(0.0795742483504507,-0.113781865596983,
-0.257856715980903));
#39537=CARTESIAN_POINT('Ctrl Pts',(0.138786453094293,0.00408587522045665,
-0.249979079981519));
#39538=CARTESIAN_POINT('Ctrl Pts',(0.0727427534113967,0.118266080365061,
-0.242101443982136));
#39539=CARTESIAN_POINT('Ctrl Pts',(-0.0589518737717736,0.125710184628324,
-0.234223807982751));
#39540=CARTESIAN_POINT('Ctrl Pts',(-0.115041149280448,0.0499548242228102,
-0.228594422830834));
#39541=CARTESIAN_POINT('Ctrl Pts',(-0.117919569985349,0.00565948084119541,
-0.225590916345378));
#39542=CARTESIAN_POINT('Ctrl Pts',(-0.117874288948281,8.4369087091269E-5,
-0.225213288526384));
#39543=CARTESIAN_POINT('Origin',(0.,0.,-0.860086711473615));
#39544=CARTESIAN_POINT('',(-0.117913678466366,6.52086126365611E-5,-0.335086711473616));
#39545=CARTESIAN_POINT('',(-0.117596036550741,3.07491073512287E-5,-0.325213288526384));
#39546=CARTESIAN_POINT('',(-0.117775,-1.1488940921122E-14,-0.860086711473615));
#39547=CARTESIAN_POINT('Ctrl Pts',(-0.117913678466366,6.52086126365584E-5,
-0.335086711473616));
#39548=CARTESIAN_POINT('Ctrl Pts',(-0.117680645599752,-0.0347155948899763,
-0.332728783659755));
#39549=CARTESIAN_POINT('Ctrl Pts',(-0.0830999363091226,-0.10863285629369,
-0.327744977179433));
#39550=CARTESIAN_POINT('Ctrl Pts',(0.0420990144004436,-0.132310422801546,
-0.320135292032649));
#39551=CARTESIAN_POINT('Ctrl Pts',(0.133711744422676,-0.0374104851459921,
-0.312257656033266));
#39552=CARTESIAN_POINT('Ctrl Pts',(0.104648535928131,0.0912527200882886,
-0.304380020033881));
#39553=CARTESIAN_POINT('Ctrl Pts',(-0.0188608286767674,0.137559602125903,
-0.296502384034497));
#39554=CARTESIAN_POINT('Ctrl Pts',(-0.105794378680474,0.0740115415589361,
-0.290071281181076));
#39555=CARTESIAN_POINT('Ctrl Pts',(-0.11763819514282,0.0175475554189854,
-0.286266056994115));
#39556=CARTESIAN_POINT('Ctrl Pts',(-0.117596201538205,3.10584990424884E-5,
-0.285086711473616));
#39557=CARTESIAN_POINT('Ctrl Pts',(-0.117596036550741,3.07491073512287E-5,
-0.325213288526384));
#39558=CARTESIAN_POINT('Ctrl Pts',(-0.117545094609287,-0.0214339135322908,
-0.323768127009581));
#39559=CARTESIAN_POINT('Ctrl Pts',(-0.101697273673151,-0.0819702105434217,
-0.319697086826317));
#39560=CARTESIAN_POINT('Ctrl Pts',(-0.00500438172789432,-0.138756369592802,
-0.31300016797659));
#39561=CARTESIAN_POINT('Ctrl Pts',(0.113252689408266,-0.0803256016526085,
-0.305122531977208));
#39562=CARTESIAN_POINT('Ctrl Pts',(0.12929828583138,0.0505996760870913,
-0.297244895977823));
#39563=CARTESIAN_POINT('Ctrl Pts',(0.0286511260671305,0.135858333988494,
-0.289367259978439));
#39564=CARTESIAN_POINT('Ctrl Pts',(-0.0892822767652217,0.101034782961183,
-0.28202339082796));
#39565=CARTESIAN_POINT('Ctrl Pts',(-0.117531007192745,0.0308308885614153,
-0.277305400343941));
#39566=CARTESIAN_POINT('Ctrl Pts',(-0.117808848495488,-0.000100531858621394,
-0.275213288526384));
#39567=CARTESIAN_POINT('Origin',(0.,0.,-0.860086711473615));
#39568=CARTESIAN_POINT('',(-0.117760958805986,-0.000103413802380578,-0.385086711473616));
#39569=CARTESIAN_POINT('',(-0.117913234095501,6.54834407544293E-5,-0.375213288526384));
#39570=CARTESIAN_POINT('',(-0.117775,-1.1488940921122E-14,-0.860086711473615));
#39571=CARTESIAN_POINT('Ctrl Pts',(-0.117760958805986,-0.000103413802380574,
-0.385086711473616));
#39572=CARTESIAN_POINT('Ctrl Pts',(-0.11784536193606,-0.00962652777585667,
-0.384443267658318));
#39573=CARTESIAN_POINT('Ctrl Pts',(-0.112459473549584,-0.0579190182986298,
-0.381173945176558));
#39574=CARTESIAN_POINT('Ctrl Pts',(-0.0460797444479301,-0.130977219954565,
-0.375278744028337));
#39575=CARTESIAN_POINT('Ctrl Pts',(0.0842094664898252,-0.110395383730082,
-0.367401108028953));
#39576=CARTESIAN_POINT('Ctrl Pts',(0.138498947975746,0.0098191855581053,
-0.359523472029569));
#39577=CARTESIAN_POINT('Ctrl Pts',(0.0677920007431425,0.121171859895995,
-0.351645836030185));
#39578=CARTESIAN_POINT('Ctrl Pts',(-0.0640977793732191,0.123165943648539,
-0.343768200030801));
#39579=CARTESIAN_POINT('Ctrl Pts',(-0.115976893950903,0.0466766976138206,
-0.338248491845278));
#39580=CARTESIAN_POINT('Ctrl Pts',(-0.117940159919669,0.00401763917385966,
-0.335354662326216));
#39581=CARTESIAN_POINT('Ctrl Pts',(-0.117913678466366,6.52086126365584E-5,
-0.335086711473616));
#39582=CARTESIAN_POINT('Ctrl Pts',(-0.117913234095501,6.54834407544259E-5,
-0.375213288526384));
#39583=CARTESIAN_POINT('Ctrl Pts',(-0.117679560835611,-0.034695429594265,
-0.372856732341682));
#39584=CARTESIAN_POINT('Ctrl Pts',(-0.0831335314732004,-0.108594147982193,
-0.36787429749052));
#39585=CARTESIAN_POINT('Ctrl Pts',(0.042030590961085,-0.132332170550159,
-0.360265983972894));
#39586=CARTESIAN_POINT('Ctrl Pts',(0.133692378221512,-0.0374796203893622,
-0.352388347973512));
#39587=CARTESIAN_POINT('Ctrl Pts',(0.104695705119469,0.0911985924704521,
-0.344510711974126));
#39588=CARTESIAN_POINT('Ctrl Pts',(-0.0187896946723457,0.137569332749615,
-0.336633075974744));
#39589=CARTESIAN_POINT('Ctrl Pts',(-0.105774639104889,0.0740526910848505,
-0.330200601492162));
#39590=CARTESIAN_POINT('Ctrl Pts',(-0.117637656828621,0.0175676783679118,
-0.326394005676042));
#39591=CARTESIAN_POINT('Ctrl Pts',(-0.117596036550741,3.07491073512287E-5,
-0.325213288526384));
#39592=CARTESIAN_POINT('Origin',(0.,0.,-0.860086711473615));
#39593=CARTESIAN_POINT('',(-0.117614005739933,5.43156211771659E-5,-0.435086711473616));
#39594=CARTESIAN_POINT('',(-0.117761548966307,-0.000103421267928797,-0.425213288526384));
#39595=CARTESIAN_POINT('',(-0.117775,-1.1488940921122E-14,-0.860086711473615));
#39596=CARTESIAN_POINT('Ctrl Pts',(-0.117614005739933,5.43156211771697E-5,
-0.435086711473616));
#39597=CARTESIAN_POINT('Ctrl Pts',(-0.11751630423813,-0.023030516556304,
-0.433531872990419));
#39598=CARTESIAN_POINT('Ctrl Pts',(-0.0998427317906378,-0.085240110976336,
-0.429351155840761));
#39599=CARTESIAN_POINT('Ctrl Pts',(0.000735454065993374,-0.138844640165656,
-0.42254456002464));
#39600=CARTESIAN_POINT('Ctrl Pts',(0.116476194166392,-0.0755755991569081,
-0.414666924025258));
#39601=CARTESIAN_POINT('Ctrl Pts',(0.127096220251881,0.0559010357068483,
-0.406789288025873));
#39602=CARTESIAN_POINT('Ctrl Pts',(0.0230108722727937,0.136926530492298,
-0.39891165202649));
#39603=CARTESIAN_POINT('Ctrl Pts',(-0.0916440184411212,0.0978503402769418,
-0.391677459842403));
#39604=CARTESIAN_POINT('Ctrl Pts',(-0.117500914801167,0.0292370702985872,
-0.387069146324779));
#39605=CARTESIAN_POINT('Ctrl Pts',(-0.117760958805986,-0.000103413802380574,
-0.385086711473616));
#39606=CARTESIAN_POINT('Ctrl Pts',(-0.117761548966307,-0.000103421267928784,
-0.425213288526384));
#39607=CARTESIAN_POINT('Ctrl Pts',(-0.117845816925276,-0.00960611208181708,
-0.424571216340245));
#39608=CARTESIAN_POINT('Ctrl Pts',(-0.112473969195758,-0.0578778634222503,
-0.421303265487644));
#39609=CARTESIAN_POINT('Ctrl Pts',(-0.0461474642941204,-0.130953371389504,
-0.415409435968583));
#39610=CARTESIAN_POINT('Ctrl Pts',(0.0841523683577151,-0.110438909985756,
-0.407531799969199));
#39611=CARTESIAN_POINT('Ctrl Pts',(0.13850400308705,0.00974756728199353,
-0.399654163969815));
#39612=CARTESIAN_POINT('Ctrl Pts',(0.0678546468187308,0.121136785677018,
-0.391776527970431));
#39613=CARTESIAN_POINT('Ctrl Pts',(-0.0640340809268605,0.123199068255027,
-0.383898891971047));
#39614=CARTESIAN_POINT('Ctrl Pts',(-0.115965640736743,0.0467176601612722,
-0.378377812156364));
#39615=CARTESIAN_POINT('Ctrl Pts',(-0.117939939786918,0.00403818539778824,
-0.375482611008143));
#39616=CARTESIAN_POINT('Ctrl Pts',(-0.117913234095501,6.54834407544259E-5,
-0.375213288526384));
#39617=CARTESIAN_POINT('Origin',(0.,0.,-0.860086711473615));
#39618=CARTESIAN_POINT('',(-0.117943154879689,4.11508268803651E-5,-0.485086711473616));
#39619=CARTESIAN_POINT('',(-0.117613716614051,5.40385033010807E-5,-0.475213288526384));
#39620=CARTESIAN_POINT('',(-0.117775,-1.1488940921122E-14,-0.860086711473615));
#39621=CARTESIAN_POINT('Ctrl Pts',(-0.117943154879689,4.11508268803695E-5,
-0.485086711473616));
#39622=CARTESIAN_POINT('Ctrl Pts',(-0.117777131663363,-0.036313138524991,
-0.48262047832252));
#39623=CARTESIAN_POINT('Ctrl Pts',(-0.0803905871069344,-0.111670381593164,
-0.477528366504963));
#39624=CARTESIAN_POINT('Ctrl Pts',(0.0474646811631436,-0.130481719169871,
-0.469810376020945));
#39625=CARTESIAN_POINT('Ctrl Pts',(0.135127355757309,-0.0319213521242443,
-0.461932740021561));
#39626=CARTESIAN_POINT('Ctrl Pts',(0.10083649107415,0.0954482952349766,
-0.454055104022177));
#39627=CARTESIAN_POINT('Ctrl Pts',(-0.024460128186944,0.136675078651873,
-0.446177468022793));
#39628=CARTESIAN_POINT('Ctrl Pts',(-0.107308137190071,0.0707605300904387,
-0.439854670506606));
#39629=CARTESIAN_POINT('Ctrl Pts',(-0.117681306771859,0.0159561492541893,
-0.43615775165688));
#39630=CARTESIAN_POINT('Ctrl Pts',(-0.117614005739933,5.43156211771697E-5,
-0.435086711473616));
#39631=CARTESIAN_POINT('Ctrl Pts',(-0.117613716614051,5.40385033010841E-5,
-0.475213288526384));
#39632=CARTESIAN_POINT('Ctrl Pts',(-0.117516613707476,-0.0230105689760668,
-0.473659821672346));
#39633=CARTESIAN_POINT('Ctrl Pts',(-0.0998665302895594,-0.0851992819494425,
-0.469480476151846));
#39634=CARTESIAN_POINT('Ctrl Pts',(0.000663658498523691,-0.138844998096641,
-0.462675251964888));
#39635=CARTESIAN_POINT('Ctrl Pts',(0.11643709586757,-0.0756358158875735,
-0.454797615965502));
#39636=CARTESIAN_POINT('Ctrl Pts',(0.127125105754884,0.0558353062664104,
-0.446919979966119));
#39637=CARTESIAN_POINT('Ctrl Pts',(0.0230816721758652,0.136914609697508,
-0.439042343966735));
#39638=CARTESIAN_POINT('Ctrl Pts',(-0.0916151488647261,0.09789031515504,
-0.43180678015349));
#39639=CARTESIAN_POINT('Ctrl Pts',(-0.117501186772313,0.0292569840323692,
-0.427197095006706));
#39640=CARTESIAN_POINT('Ctrl Pts',(-0.117761548966307,-0.000103421267928784,
-0.425213288526384));
#39641=CARTESIAN_POINT('Origin',(0.,0.,-0.860086711473615));
#39642=CARTESIAN_POINT('',(-0.117715464068169,-9.94428558149901E-5,-0.535086711473616));
#39643=CARTESIAN_POINT('',(-0.117942852310966,4.1481206443531E-5,-0.525213288526384));
#39644=CARTESIAN_POINT('',(-0.117775,-1.1488940921122E-14,-0.860086711473615));
#39645=CARTESIAN_POINT('Ctrl Pts',(-0.117715464068169,-9.94428558149935E-5,
-0.535086711473616));
#39646=CARTESIAN_POINT('Ctrl Pts',(-0.117807243319497,-0.0112364652973298,
-0.534334962321083));
#39647=CARTESIAN_POINT('Ctrl Pts',(-0.111274845462934,-0.0611698966227711,
-0.530957334502088));
#39648=CARTESIAN_POINT('Ctrl Pts',(-0.0406950061935692,-0.13274897914597,
-0.524953828016632));
#39649=CARTESIAN_POINT('Ctrl Pts',(0.0886454911998817,-0.106866046463675,
-0.51707619201725));
#39650=CARTESIAN_POINT('Ctrl Pts',(0.137982710697811,0.0154643636671598,
-0.509198556017864));
#39651=CARTESIAN_POINT('Ctrl Pts',(0.0627894098300584,0.12383805961159,
-0.501320920018481));
#39652=CARTESIAN_POINT('Ctrl Pts',(-0.0690718448751183,0.120446898013915,
-0.493443284019097));
#39653=CARTESIAN_POINT('Ctrl Pts',(-0.116829683066834,0.0434448969256025,
-0.488031881170809));
#39654=CARTESIAN_POINT('Ctrl Pts',(-0.117953901982784,0.00239445601084412,
-0.485246356988981));
#39655=CARTESIAN_POINT('Ctrl Pts',(-0.117943154879689,4.11508268803695E-5,
-0.485086711473616));
#39656=CARTESIAN_POINT('Ctrl Pts',(-0.117942852310966,4.14812064435314E-5,
-0.525213288526384));
#39657=CARTESIAN_POINT('Ctrl Pts',(-0.117775766365834,-0.0362928338941266,
-0.522748427004448));
#39658=CARTESIAN_POINT('Ctrl Pts',(-0.0804255975098662,-0.111632149146056,
-0.517657686816049));
#39659=CARTESIAN_POINT('Ctrl Pts',(0.0473972024675744,-0.130506241756924,
-0.509941067961191));
#39660=CARTESIAN_POINT('Ctrl Pts',(0.135110827714643,-0.0319912202527791,
-0.502063431961806));
#39661=CARTESIAN_POINT('Ctrl Pts',(0.100885830377846,0.0953961381189002,
-0.494185795962423));
#39662=CARTESIAN_POINT('Ctrl Pts',(-0.0243894506605435,0.136687704770994,
-0.486308159963038));
#39663=CARTESIAN_POINT('Ctrl Pts',(-0.107289510134903,0.070801717063382,
-0.479983990817693));
#39664=CARTESIAN_POINT('Ctrl Pts',(-0.11768075010354,0.0159763334949808,
-0.476285700338808));
#39665=CARTESIAN_POINT('Ctrl Pts',(-0.117613716614051,5.40385033010841E-5,
-0.475213288526384));
#39666=CARTESIAN_POINT('Origin',(0.,0.,-0.860086711473615));
#39667=CARTESIAN_POINT('',(-0.117641121075241,7.43322482763471E-5,-0.585086711473616));
#39668=CARTESIAN_POINT('',(-0.117716014989814,-9.95338970442156E-5,-0.575213288526384));
#39669=CARTESIAN_POINT('',(-0.117775,-1.1488940921122E-14,-0.860086711473615));
#39670=CARTESIAN_POINT('Ctrl Pts',(-0.117641121075241,7.43322482763594E-5,
-0.585086711473616));
#39671=CARTESIAN_POINT('Ctrl Pts',(-0.11749601672539,-0.0246042219688241,
-0.583423567653184));
#39672=CARTESIAN_POINT('Ctrl Pts',(-0.0979139840066323,-0.0884576215721144,
-0.579134545166291));
#39673=CARTESIAN_POINT('Ctrl Pts',(0.00640231340113165,-0.138698901431908,
-0.572219644012936));
#39674=CARTESIAN_POINT('Ctrl Pts',(0.119464024723476,-0.0707581928149885,
-0.564342008013553));
#39675=CARTESIAN_POINT('Ctrl Pts',(0.124708480222252,0.0610423619770983,
-0.556464372014168));
#39676=CARTESIAN_POINT('Ctrl Pts',(0.0174025166897942,0.137751687439221,
-0.548586736014785));
#39677=CARTESIAN_POINT('Ctrl Pts',(-0.0938705497883859,0.0946825900337148,
-0.541460849167934));
#39678=CARTESIAN_POINT('Ctrl Pts',(-0.117486656090001,0.0276654337451075,
-0.536960840987544));
#39679=CARTESIAN_POINT('Ctrl Pts',(-0.117715464068169,-9.94428558149935E-5,
-0.535086711473616));
#39680=CARTESIAN_POINT('Ctrl Pts',(-0.117716014989814,-9.95338970442277E-5,
-0.575213288526384));
#39681=CARTESIAN_POINT('Ctrl Pts',(-0.117807744610619,-0.0112161026403652,
-0.574462911003011));
#39682=CARTESIAN_POINT('Ctrl Pts',(-0.111290340970323,-0.061128709613193,
-0.571086654813175));
#39683=CARTESIAN_POINT('Ctrl Pts',(-0.0407636430850622,-0.132727914643187,
-0.565084519956878));
#39684=CARTESIAN_POINT('Ctrl Pts',(0.0885902173532643,-0.10691186715079,
-0.557206883957495));
#39685=CARTESIAN_POINT('Ctrl Pts',(0.137990684964291,0.0153930114396808,
-0.54932924795811));
#39686=CARTESIAN_POINT('Ctrl Pts',(0.0628534353842331,0.123805571754376,
-0.541451611958728));
#39687=CARTESIAN_POINT('Ctrl Pts',(-0.0690095516253471,0.120482595112153,
-0.533573975959342));
#39688=CARTESIAN_POINT('Ctrl Pts',(-0.116819314516747,0.043485790171169,
-0.528161201481895));
#39689=CARTESIAN_POINT('Ctrl Pts',(-0.117953767204779,0.00241502130745575,
-0.525374305670909));
#39690=CARTESIAN_POINT('Ctrl Pts',(-0.117942852310966,4.14812064435314E-5,
-0.525213288526384));
#39691=CARTESIAN_POINT('Origin',(0.,0.,-0.860086711473615));
#39692=CARTESIAN_POINT('',(-0.117959517728684,1.36525406724091E-5,-0.635086711473616));
#39693=CARTESIAN_POINT('',(-0.117640721763206,7.41070646922068E-5,-0.625213288526384));
#39694=CARTESIAN_POINT('',(-0.117775,-1.1488940921122E-14,-0.860086711473615));
#39695=CARTESIAN_POINT('Ctrl Pts',(-0.117959517728684,1.36525406724122E-5,
-0.635086711473616));
#39696=CARTESIAN_POINT('Ctrl Pts',(-0.11789655159411,-0.0379230490610994,
-0.632512172985285));
#39697=CARTESIAN_POINT('Ctrl Pts',(-0.0775687689381847,-0.11466827637256,
-0.627311755830493));
#39698=CARTESIAN_POINT('Ctrl Pts',(0.0527512205227371,-0.128435499614995,
-0.619485460009241));
#39699=CARTESIAN_POINT('Ctrl Pts',(0.136317732660755,-0.0263790208529794,
-0.611607824009857));
#39700=CARTESIAN_POINT('Ctrl Pts',(0.0968563621793423,0.099484776038326,
-0.603730188010473));
#39701=CARTESIAN_POINT('Ctrl Pts',(-0.030018654400187,0.135562732744109,
-0.595852552011088));
#39702=CARTESIAN_POINT('Ctrl Pts',(-0.108735202118669,0.0675074251532259,
-0.589638059832136));
#39703=CARTESIAN_POINT('Ctrl Pts',(-0.117725116826057,0.0143598701569989,
-0.586049446319646));
#39704=CARTESIAN_POINT('Ctrl Pts',(-0.117641121075241,7.43322482763594E-5,
-0.585086711473616));
#39705=CARTESIAN_POINT('Ctrl Pts',(-0.117640721763206,7.41070646922016E-5,
-0.625213288526384));
#39706=CARTESIAN_POINT('Ctrl Pts',(-0.117496212726526,-0.0245843038632945,
-0.623551516335112));
#39707=CARTESIAN_POINT('Ctrl Pts',(-0.0979390209757794,-0.0884169574269978,
-0.619263865477377));
#39708=CARTESIAN_POINT('Ctrl Pts',(0.00633059155599267,-0.138702186982091,
-0.612350335953182));
#39709=CARTESIAN_POINT('Ctrl Pts',(0.119427417367179,-0.0708199567217074,
-0.604472699953798));
#39710=CARTESIAN_POINT('Ctrl Pts',(0.124740024447541,0.0609778671354031,
-0.596595063954414));
#39711=CARTESIAN_POINT('Ctrl Pts',(0.0174737442840939,0.137742666154633,
-0.588717427955029));
#39712=CARTESIAN_POINT('Ctrl Pts',(-0.0938429978234783,0.0947228355430488,
-0.581590169479021));
#39713=CARTESIAN_POINT('Ctrl Pts',(-0.117486745051261,0.0276853300359315,
-0.577088789669472));
#39714=CARTESIAN_POINT('Ctrl Pts',(-0.117716014989814,-9.95338970442277E-5,
-0.575213288526384));
#39715=CARTESIAN_POINT('Origin',(0.,0.,-0.860086711473615));
#39716=CARTESIAN_POINT('',(-0.117674062045845,-8.95928838821694E-5,-0.685086711473616));
#39717=CARTESIAN_POINT('',(-0.117959439303798,1.41398256485216E-5,-0.675213288526384));
#39718=CARTESIAN_POINT('',(-0.117775,-1.1488940921122E-14,-0.860086711473615));
#39719=CARTESIAN_POINT('Ctrl Pts',(-0.117674062045845,-8.959288388217E-5,
-0.685086711473616));
#39720=CARTESIAN_POINT('Ctrl Pts',(-0.117766071086712,-0.0128419083078311,
-0.684226656983848));
#39721=CARTESIAN_POINT('Ctrl Pts',(-0.110011270651638,-0.0644205347554902,
-0.680740723827619));
#39722=CARTESIAN_POINT('Ctrl Pts',(-0.0352415432127178,-0.134301243779432,
-0.674628912004927));
#39723=CARTESIAN_POINT('Ctrl Pts',(0.0929332862694289,-0.103157640277856,
-0.666751276005546));
#39724=CARTESIAN_POINT('Ctrl Pts',(0.137236721157382,0.0210832714786364,
-0.65887364000616));
#39725=CARTESIAN_POINT('Ctrl Pts',(0.0576820272073694,0.126298097011918,
-0.650996004006777));
#39726=CARTESIAN_POINT('Ctrl Pts',(-0.0739307082268856,0.11752694649454,
-0.643118368007392));
#39727=CARTESIAN_POINT('Ctrl Pts',(-0.117613549182942,0.0402187154116586,
-0.637815270496339));
#39728=CARTESIAN_POINT('Ctrl Pts',(-0.117960773368318,0.000770167553659683,
-0.635138051651747));
#39729=CARTESIAN_POINT('Ctrl Pts',(-0.117959517728684,1.36525406724122E-5,
-0.635086711473616));
#39730=CARTESIAN_POINT('Ctrl Pts',(-0.117959439303798,1.41398256485209E-5,
-0.675213288526384));
#39731=CARTESIAN_POINT('Ctrl Pts',(-0.117894944776542,-0.037902354392603,
-0.672640121667213));
#39732=CARTESIAN_POINT('Ctrl Pts',(-0.0776051478672742,-0.114630810377079,
-0.66744107614158));
#39733=CARTESIAN_POINT('Ctrl Pts',(0.052684764963274,-0.128462629580122,
-0.659616151949486));
#39734=CARTESIAN_POINT('Ctrl Pts',(0.136304088268209,-0.0264495720340304,
-0.651738515950102));
#39735=CARTESIAN_POINT('Ctrl Pts',(0.0969077799094599,0.0994347114333518,
-0.643860879950719));
#39736=CARTESIAN_POINT('Ctrl Pts',(-0.0299485461911899,0.135578214853137,
-0.635983243951333));
#39737=CARTESIAN_POINT('Ctrl Pts',(-0.108717659726821,0.0675486323374574,
-0.629767380143224));
#39738=CARTESIAN_POINT('Ctrl Pts',(-0.117724561232128,0.0143801195063431,
-0.626177395001573));
#39739=CARTESIAN_POINT('Ctrl Pts',(-0.117640721763206,7.41070646922016E-5,
-0.625213288526384));
#39740=CARTESIAN_POINT('Origin',(0.,0.,-0.860086711473615));
#39741=CARTESIAN_POINT('',(-0.11756447877375,-3.1000136807011E-5,-0.735086711473616));
#39742=CARTESIAN_POINT('',(-0.117673801045155,-9.24777646016256E-5,-0.725213288526384));
#39743=CARTESIAN_POINT('',(-0.117775,-1.1488940921122E-14,-0.860086711473615));
#39744=CARTESIAN_POINT('Ctrl Pts',(-0.11756447877375,-3.10001368070065E-5,
-0.735086711473616));
#39745=CARTESIAN_POINT('Ctrl Pts',(-0.117424235421919,-0.0262843339558975,
-0.733315262315949));
#39746=CARTESIAN_POINT('Ctrl Pts',(-0.0959617948024944,-0.0915157796904448,
-0.728917934491822));
#39747=CARTESIAN_POINT('Ctrl Pts',(0.0121016636501963,-0.138407426356883,
-0.721894728001232));
#39748=CARTESIAN_POINT('Ctrl Pts',(0.122230504106716,-0.0657785464558806,
-0.714017092001848));
#39749=CARTESIAN_POINT('Ctrl Pts',(0.122124503576362,0.0660587059756678,
-0.706139456002464));
#39750=CARTESIAN_POINT('Ctrl Pts',(0.0117590361697431,0.138359448122069,
-0.69826182000308));
#39751=CARTESIAN_POINT('Ctrl Pts',(-0.0959918518471737,0.0914906904383485,
-0.691244238493464));
#39752=CARTESIAN_POINT('Ctrl Pts',(-0.117485153330444,0.0260928724742271,
-0.68685253565031));
#39753=CARTESIAN_POINT('Ctrl Pts',(-0.117674062045845,-8.959288388217E-5,
-0.685086711473616));
#39754=CARTESIAN_POINT('Ctrl Pts',(-0.117673801045155,-9.24777646016256E-5,
-0.725213288526384));
#39755=CARTESIAN_POINT('Ctrl Pts',(-0.117766777010352,-0.0128209253377562,
-0.724354605665775));
#39756=CARTESIAN_POINT('Ctrl Pts',(-0.110031606923338,-0.0643651828756224,
-0.720870044138706));
#39757=CARTESIAN_POINT('Ctrl Pts',(-0.035307936335489,-0.134294310470789,
-0.714759603945173));
#39758=CARTESIAN_POINT('Ctrl Pts',(0.0928783259292375,-0.103199726094761,
-0.70688196794579));
#39759=CARTESIAN_POINT('Ctrl Pts',(0.137248444930391,0.0210091710227868,
-0.699004331946405));
#39760=CARTESIAN_POINT('Ctrl Pts',(0.0577468814636623,0.126269898836241,
-0.691126695947023));
#39761=CARTESIAN_POINT('Ctrl Pts',(-0.0738696902757825,0.117564288535968,
-0.683249059947637));
#39762=CARTESIAN_POINT('Ctrl Pts',(-0.117604048723001,0.040259560390861,
-0.677944590807425));
#39763=CARTESIAN_POINT('Ctrl Pts',(-0.117960760486325,0.000790866344265062,
-0.675266000333674));
#39764=CARTESIAN_POINT('Ctrl Pts',(-0.117959439303798,1.41398256485209E-5,
-0.675213288526384));
#39765=CARTESIAN_POINT('Origin',(3.28582941601228E-18,0.,-0.01365));
#39766=CARTESIAN_POINT('',(-0.00798678478682301,0.146131905375825,-0.0136500000000001));
#39767=CARTESIAN_POINT('Ctrl Pts',(0.106341965058147,-0.0510185301167581,
-0.01365));
#39768=CARTESIAN_POINT('Ctrl Pts',(0.108342566854854,-0.0479029045944487,
-0.01365));
#39769=CARTESIAN_POINT('Ctrl Pts',(0.110183088349928,-0.044695819810311,
-0.0136499999999998));
#39770=CARTESIAN_POINT('Ctrl Pts',(0.111853496790312,-0.0414060369465285,
-0.0136499999999998));
#39771=CARTESIAN_POINT('Ctrl Pts',(0.114271585472934,-0.0366437365899957,
-0.0136499999999998));
#39772=CARTESIAN_POINT('Ctrl Pts',(0.116333554267275,-0.0317083325327904,
-0.01365));
#39773=CARTESIAN_POINT('Ctrl Pts',(0.118049888741346,-0.026638969815401,
-0.01365));
#39774=CARTESIAN_POINT('Ctrl Pts',(0.11924838271765,-0.0230990999518747,
-0.01365));
#39775=CARTESIAN_POINT('Ctrl Pts',(0.120278297505165,-0.0194918553238869,
-0.0136499999999997));
#39776=CARTESIAN_POINT('Ctrl Pts',(0.121138443618246,-0.0158468448199564,
-0.0136499999999997));
#39777=CARTESIAN_POINT('Ctrl Pts',(0.122741275996562,-0.00905457921978598,
-0.0136499999999998));
#39778=CARTESIAN_POINT('Ctrl Pts',(0.123760167768593,-0.00212023278417033,
-0.0136499999999998));
#39779=CARTESIAN_POINT('Ctrl Pts',(0.124213451674144,0.00487494639068494,
-0.0136499999999998));
#39780=CARTESIAN_POINT('Ctrl Pts',(0.124483209002123,0.00903790214498723,
-0.0136499999999997));
#39781=CARTESIAN_POINT('Ctrl Pts',(0.124551731397662,0.0132256840072574,
-0.0136499999999997));
#39782=CARTESIAN_POINT('Ctrl Pts',(0.124422405850686,0.0173967602373136,
-0.0136499999999997));
#39783=CARTESIAN_POINT('Ctrl Pts',(0.124128401004826,0.0268791606815134,
-0.0136499999999999));
#39784=CARTESIAN_POINT('Ctrl Pts',(0.122818528710923,0.0362997013229908,
-0.0136500000000001));
#39785=CARTESIAN_POINT('Ctrl Pts',(0.120525658053403,0.045471105234349,
-0.0136500000000001));
#39786=CARTESIAN_POINT('Ctrl Pts',(0.119627364156967,0.0490642499799099,
-0.0136500000000002));
#39787=CARTESIAN_POINT('Ctrl Pts',(0.118577639382974,0.0526192976583267,
-0.0136499999999998));
#39788=CARTESIAN_POINT('Ctrl Pts',(0.117376297305641,0.0561250923148867,
-0.0136499999999998));
#39789=CARTESIAN_POINT('Ctrl Pts',(0.116377302902627,0.0590403895529535,
-0.0136499999999998));
#39790=CARTESIAN_POINT('Ctrl Pts',(0.115273111640123,0.0619215009930825,
-0.0136500000000001));
#39791=CARTESIAN_POINT('Ctrl Pts',(0.114069691815438,0.0647487244549216,
-0.0136500000000001));
#39792=CARTESIAN_POINT('Ctrl Pts',(0.111990795593586,0.0696327259085989,
-0.0136500000000001));
#39793=CARTESIAN_POINT('Ctrl Pts',(0.109612823724072,0.0743660871426123,
-0.0136499999999997));
#39794=CARTESIAN_POINT('Ctrl Pts',(0.106940366893081,0.0789174960988524,
-0.0136499999999998));
#39795=CARTESIAN_POINT('Ctrl Pts',(0.10367803111746,0.0844735163477981,
-0.0136499999999999));
#39796=CARTESIAN_POINT('Ctrl Pts',(0.0999772058860202,0.0897587318249706,
-0.01365));
#39797=CARTESIAN_POINT('Ctrl Pts',(0.0958886739670196,0.0947554852369029,
-0.01365));
#39798=CARTESIAN_POINT('Ctrl Pts',(0.0939519614645511,0.0971224166920954,
-0.01365));
#39799=CARTESIAN_POINT('Ctrl Pts',(0.0919280942758348,0.0994245574006695,
-0.0136499999999999));
#39800=CARTESIAN_POINT('Ctrl Pts',(0.0898217035368732,0.101659607670364,
-0.0136499999999999));
#39801=CARTESIAN_POINT('Ctrl Pts',(0.0875898148282813,0.104027821396241,
-0.0136499999999999));
#39802=CARTESIAN_POINT('Ctrl Pts',(0.0852708873134785,0.106314590966667,
-0.01365));
#39803=CARTESIAN_POINT('Ctrl Pts',(0.0828754001610831,0.108514666841639,
-0.01365));
#39804=CARTESIAN_POINT('Ctrl Pts',(0.0767368610952631,0.114152456087464,
-0.0136500000000001));
#39805=CARTESIAN_POINT('Ctrl Pts',(0.0700902785826064,0.119229332008775,
-0.0136500000000001));
#39806=CARTESIAN_POINT('Ctrl Pts',(0.0630385493739984,0.123708097010451,
-0.0136500000000001));
#39807=CARTESIAN_POINT('Ctrl Pts',(0.0583362796780647,0.126694649715408,
-0.0136500000000002));
#39808=CARTESIAN_POINT('Ctrl Pts',(0.0534533030596454,0.129415029588119,
-0.0136500000000001));
#39809=CARTESIAN_POINT('Ctrl Pts',(0.0484154076414554,0.13185404772708,
-0.0136500000000001));
#39810=CARTESIAN_POINT('Ctrl Pts',(0.0455727092826764,0.133230295601465,
-0.0136500000000002));
#39811=CARTESIAN_POINT('Ctrl Pts',(0.0426811633551951,0.134516309136496,
-0.0136500000000002));
#39812=CARTESIAN_POINT('Ctrl Pts',(0.0397579206933862,0.135704614292114,
-0.0136500000000002));
#39813=CARTESIAN_POINT('Ctrl Pts',(0.0301875705441006,0.139594984589468,
-0.0136500000000001));
#39814=CARTESIAN_POINT('Ctrl Pts',(0.0202471683700578,0.142457694671499,
-0.0136499999999998));
#39815=CARTESIAN_POINT('Ctrl Pts',(0.0101045343131722,0.144212130069045,
-0.0136499999999998));
#39816=CARTESIAN_POINT('Ctrl Pts',(0.00413458586419398,0.145244789713637,
-0.0136499999999998));
#39817=CARTESIAN_POINT('Ctrl Pts',(-0.00190612190526973,0.145892796544534,
-0.0136499999999999));
#39818=CARTESIAN_POINT('Ctrl Pts',(-0.00798678478682509,0.146131905375825,
-0.0136499999999999));
#39819=CARTESIAN_POINT('',(-0.14635,-1.79227059055215E-17,-0.01365));
#39820=CARTESIAN_POINT('Origin',(0.,0.,-0.01365));
#39821=CARTESIAN_POINT('',(-0.119316161853458,0.0851151957093249,-0.0136499999999998));
#39822=CARTESIAN_POINT('Origin',(0.,0.,-0.01365));
#39823=CARTESIAN_POINT('Ctrl Pts',(-0.119316161853456,0.0851151957093283,
-0.01365));
#39824=CARTESIAN_POINT('Ctrl Pts',(-0.121618076638167,0.0812021306583877,
-0.01365));
#39825=CARTESIAN_POINT('Ctrl Pts',(-0.123722085229027,0.0771843356216899,
-0.0136499999999999));
#39826=CARTESIAN_POINT('Ctrl Pts',(-0.1256140695707,0.0730688966137306,
-0.0136499999999999));
#39827=CARTESIAN_POINT('Ctrl Pts',(-0.128792092093133,0.0661560709793384,
-0.0136499999999999));
#39828=CARTESIAN_POINT('Ctrl Pts',(-0.131372690800445,0.0589676394657173,
-0.0136499999999999));
#39829=CARTESIAN_POINT('Ctrl Pts',(-0.133357756374321,0.0515830681614563,
-0.0136499999999998));
#39830=CARTESIAN_POINT('Ctrl Pts',(-0.134263694945998,0.0482129185463161,
-0.0136499999999998));
#39831=CARTESIAN_POINT('Ctrl Pts',(-0.13504450061239,0.0448044325552989,
-0.01365));
#39832=CARTESIAN_POINT('Ctrl Pts',(-0.135698940481304,0.0413736537756237,
-0.01365));
#39833=CARTESIAN_POINT('Ctrl Pts',(-0.136955087895919,0.0347885355716289,
-0.0136499999999998));
#39834=CARTESIAN_POINT('Ctrl Pts',(-0.137748728715298,0.0281123211991962,
-0.0136499999999999));
#39835=CARTESIAN_POINT('Ctrl Pts',(-0.138080117385458,0.0214001920011799,
-0.0136499999999999));
#39836=CARTESIAN_POINT('Ctrl Pts',(-0.138253918763604,0.017879922873254,
-0.0136499999999999));
#39837=CARTESIAN_POINT('Ctrl Pts',(-0.138300356470715,0.0143477408926489,
-0.0136500000000001));
#39838=CARTESIAN_POINT('Ctrl Pts',(-0.138218634317284,0.0108185068260204,
-0.0136500000000001));
#39839=CARTESIAN_POINT('Ctrl Pts',(-0.137988104065489,0.000862880550021112,
-0.0136500000000001));
#39840=CARTESIAN_POINT('Ctrl Pts',(-0.136743935784425,-0.00901554091696978,
-0.0136500000000002));
#39841=CARTESIAN_POINT('Ctrl Pts',(-0.134486996926361,-0.0186350354119432,
-0.0136500000000003));
#39842=CARTESIAN_POINT('Ctrl Pts',(-0.132955925535783,-0.0251607473338499,
-0.0136500000000003));
#39843=CARTESIAN_POINT('Ctrl Pts',(-0.130957707016009,-0.0315672393290349,
-0.0136500000000003));
#39844=CARTESIAN_POINT('Ctrl Pts',(-0.128480470731525,-0.0377902656536371,
-0.0136500000000003));
#39845=CARTESIAN_POINT('Ctrl Pts',(-0.127462904475702,-0.0403464778473128,
-0.0136500000000002));
#39846=CARTESIAN_POINT('Ctrl Pts',(-0.126364970507356,-0.0428696996823228,
-0.0136500000000001));
#39847=CARTESIAN_POINT('Ctrl Pts',(-0.125189987366655,-0.0453475440721538,
-0.0136500000000001));
#39848=CARTESIAN_POINT('Ctrl Pts',(-0.122981386926095,-0.0500051157610184,
-0.0136500000000001));
#39849=CARTESIAN_POINT('Ctrl Pts',(-0.120497522574337,-0.0545110076612892,
-0.0136500000000001));
#39850=CARTESIAN_POINT('Ctrl Pts',(-0.117735701698672,-0.0588371322340339,
-0.0136500000000001));
#39851=CARTESIAN_POINT('Ctrl Pts',(-0.114499346202997,-0.0639065692707884,
-0.0136500000000001));
#39852=CARTESIAN_POINT('Ctrl Pts',(-0.11088126561812,-0.0687293688896335,
-0.0136500000000003));
#39853=CARTESIAN_POINT('Ctrl Pts',(-0.106920330946986,-0.0732809440582911,
-0.0136500000000003));
#39854=CARTESIAN_POINT('Ctrl Pts',(-0.104866691559283,-0.0756408148510523,
-0.0136500000000003));
#39855=CARTESIAN_POINT('Ctrl Pts',(-0.102720811300817,-0.0779276639257738,
-0.01365));
#39856=CARTESIAN_POINT('Ctrl Pts',(-0.100487766234768,-0.0801372691093224,
-0.01365));
#39857=CARTESIAN_POINT('Ctrl Pts',(-0.0983185592222529,-0.0822837063361919,
-0.0136499999999999));
#39858=CARTESIAN_POINT('Ctrl Pts',(-0.096070846136074,-0.0843533002970022,
-0.01365));
#39859=CARTESIAN_POINT('Ctrl Pts',(-0.0937558409539707,-0.0863381453211609,
-0.01365));
#39860=CARTESIAN_POINT('Ctrl Pts',(-0.0882265183286274,-0.0910788900005786,
-0.01365));
#39861=CARTESIAN_POINT('Ctrl Pts',(-0.0823041470487266,-0.0953470446859006,
-0.0136500000000001));
#39862=CARTESIAN_POINT('Ctrl Pts',(-0.0760595239664612,-0.0990980605043351,
-0.01365));
#39863=CARTESIAN_POINT('Ctrl Pts',(-0.0711801715289065,-0.102028986508334,
-0.01365));
#39864=CARTESIAN_POINT('Ctrl Pts',(-0.0661037637394787,-0.104643891124205,
-0.01365));
#39865=CARTESIAN_POINT('Ctrl Pts',(-0.0608627395111615,-0.106913236962818,
-0.01365));
#39866=CARTESIAN_POINT('Ctrl Pts',(-0.0584349443975771,-0.107964464069964,
-0.01365));
#39867=CARTESIAN_POINT('Ctrl Pts',(-0.0559735570906737,-0.108940481663004,
-0.0136499999999999));
#39868=CARTESIAN_POINT('Ctrl Pts',(-0.0534903959610244,-0.109835670325941,
-0.0136499999999999));
#39869=CARTESIAN_POINT('Ctrl Pts',(-0.0452610837496131,-0.112802367455442,
-0.0136499999999998));
#39870=CARTESIAN_POINT('Ctrl Pts',(-0.0367667177655714,-0.114896564272088,
-0.0136500000000001));
#39871=CARTESIAN_POINT('Ctrl Pts',(-0.0281307376421152,-0.116018109833104,
-0.01365));
#39872=CARTESIAN_POINT('Ctrl Pts',(-0.0233995953608321,-0.116632538253301,
-0.01365));
#39873=CARTESIAN_POINT('Ctrl Pts',(-0.0186259220515163,-0.116954205068862,
-0.0136500000000001));
#39874=CARTESIAN_POINT('Ctrl Pts',(-0.0138313775859342,-0.116960008631478,
-0.0136500000000001));
#39875=CARTESIAN_POINT('Ctrl Pts',(0.103670563470625,-0.0558870726973871,
-0.754147783942094));
#39876=CARTESIAN_POINT('Ctrl Pts',(0.122112048111452,-0.0216781042960277,
-0.751521905275632));
#39877=CARTESIAN_POINT('Ctrl Pts',(0.122205985182819,0.0658325307641024,
-0.746270147942709));
#39878=CARTESIAN_POINT('Ctrl Pts',(0.0118087845259011,0.138432738517456,
-0.738392511943327));
#39879=CARTESIAN_POINT('Ctrl Pts',(-0.10914203235335,0.0857620083606503,
-0.730514875943941));
#39880=CARTESIAN_POINT('Ctrl Pts',(-0.13164238341053,-0.0441410325559887,
-0.722637239944559));
#39881=CARTESIAN_POINT('Ctrl Pts',(-0.035307936335489,-0.134294310470789,
-0.714759603945173));
#39882=CARTESIAN_POINT('Ctrl Pts',(0.0928783259292375,-0.103199726094761,
-0.70688196794579));
#39883=CARTESIAN_POINT('Ctrl Pts',(0.137248444930391,0.0210091710227868,
-0.699004331946405));
#39884=CARTESIAN_POINT('Ctrl Pts',(0.0577468814636623,0.126269898836241,
-0.691126695947023));
#39885=CARTESIAN_POINT('Ctrl Pts',(-0.0738696902757825,0.117564288535968,
-0.683249059947637));
#39886=CARTESIAN_POINT('Ctrl Pts',(-0.138819329421003,0.00275949030613511,
-0.675371423948254));
#39887=CARTESIAN_POINT('Ctrl Pts',(-0.0784828326356314,-0.114537633731478,
-0.66749378794887));
#39888=CARTESIAN_POINT('Ctrl Pts',(0.052684764963274,-0.128462629580122,
-0.659616151949486));
#39889=CARTESIAN_POINT('Ctrl Pts',(0.136304088268209,-0.0264495720340304,
-0.651738515950102));
#39890=CARTESIAN_POINT('Ctrl Pts',(0.0969077799094599,0.0994347114333518,
-0.643860879950719));
#39891=CARTESIAN_POINT('Ctrl Pts',(-0.0299485461911899,0.135578214853137,
-0.635983243951333));
#39892=CARTESIAN_POINT('Ctrl Pts',(-0.129776088039535,0.0493613502639795,
-0.628105607951951));
#39893=CARTESIAN_POINT('Ctrl Pts',(-0.112479641400627,-0.0814045746418012,
-0.620227971952565));
#39894=CARTESIAN_POINT('Ctrl Pts',(0.00633059155599267,-0.138702186982091,
-0.612350335953182));
#39895=CARTESIAN_POINT('Ctrl Pts',(0.119427417367179,-0.0708199567217074,
-0.604472699953798));
#39896=CARTESIAN_POINT('Ctrl Pts',(0.124740024447541,0.0609778671354031,
-0.596595063954414));
#39897=CARTESIAN_POINT('Ctrl Pts',(0.0174737442840939,0.137742666154633,
-0.588717427955029));
#39898=CARTESIAN_POINT('Ctrl Pts',(-0.105562732912909,0.0901935885599426,
-0.580839791955647));
#39899=CARTESIAN_POINT('Ctrl Pts',(-0.133327983520661,-0.0387559382421815,
-0.572962155956263));
#39900=CARTESIAN_POINT('Ctrl Pts',(-0.0407636430850622,-0.132727914643187,
-0.565084519956878));
#39901=CARTESIAN_POINT('Ctrl Pts',(0.0885902173532643,-0.10691186715079,
-0.557206883957495));
#39902=CARTESIAN_POINT('Ctrl Pts',(0.137990684964291,0.0153930114396808,
-0.54932924795811));
#39903=CARTESIAN_POINT('Ctrl Pts',(0.0628534353842331,0.123805571754376,
-0.541451611958728));
#39904=CARTESIAN_POINT('Ctrl Pts',(-0.0690095516253471,0.120482595112153,
-0.533573975959342));
#39905=CARTESIAN_POINT('Ctrl Pts',(-0.138590856156792,0.00842309494862901,
-0.525696339959959));
#39906=CARTESIAN_POINT('Ctrl Pts',(-0.0830927840904983,-0.11123831700858,
-0.517818703960574));
#39907=CARTESIAN_POINT('Ctrl Pts',(0.0473972024675744,-0.130506241756924,
-0.509941067961191));
#39908=CARTESIAN_POINT('Ctrl Pts',(0.135110827714643,-0.0319912202527791,
-0.502063431961806));
#39909=CARTESIAN_POINT('Ctrl Pts',(0.100885830377846,0.0953961381189002,
-0.494185795962423));
#39910=CARTESIAN_POINT('Ctrl Pts',(-0.0243894506605435,0.136687704770994,
-0.486308159963038));
#39911=CARTESIAN_POINT('Ctrl Pts',(-0.127653053808612,0.0546175044503093,
-0.478430523963655));
#39912=CARTESIAN_POINT('Ctrl Pts',(-0.115708736071418,-0.0767454385342013,
-0.470552887964269));
#39913=CARTESIAN_POINT('Ctrl Pts',(0.000663658498523691,-0.138844998096641,
-0.462675251964888));
#39914=CARTESIAN_POINT('Ctrl Pts',(0.11643709586757,-0.0756358158875735,
-0.454797615965502));
#39915=CARTESIAN_POINT('Ctrl Pts',(0.127125105754884,0.0558353062664104,
-0.446919979966119));
#39916=CARTESIAN_POINT('Ctrl Pts',(0.0230816721758652,0.136914609697508,
-0.439042343966735));
#39917=CARTESIAN_POINT('Ctrl Pts',(-0.101793158558169,0.094427362611722,
-0.431164707967351));
#39918=CARTESIAN_POINT('Ctrl Pts',(-0.134798834517268,-0.033281348407788,
-0.423287071967966));
#39919=CARTESIAN_POINT('Ctrl Pts',(-0.0461474642941204,-0.130953371389504,
-0.415409435968583));
#39920=CARTESIAN_POINT('Ctrl Pts',(0.0841523683577151,-0.110438909985756,
-0.407531799969199));
#39921=CARTESIAN_POINT('Ctrl Pts',(0.13850400308705,0.00974756728199353,
-0.399654163969815));
#39922=CARTESIAN_POINT('Ctrl Pts',(0.0678546468187308,0.121136785677018,
-0.391776527970431));
#39923=CARTESIAN_POINT('Ctrl Pts',(-0.0640340809268605,0.123199068255027,
-0.383898891971047));
#39924=CARTESIAN_POINT('Ctrl Pts',(-0.138131529033763,0.0140731881906393,
-0.376021255971662));
#39925=CARTESIAN_POINT('Ctrl Pts',(-0.0875641470101639,-0.107753858851722,
-0.368143619972279));
#39926=CARTESIAN_POINT('Ctrl Pts',(0.042030590961085,-0.132332170550159,
-0.360265983972894));
#39927=CARTESIAN_POINT('Ctrl Pts',(0.133692378221512,-0.0374796203893622,
-0.352388347973512));
#39928=CARTESIAN_POINT('Ctrl Pts',(0.104695705119469,0.0911985924704521,
-0.344510711974126));
#39929=CARTESIAN_POINT('Ctrl Pts',(-0.0187896946723457,0.137569332749615,
-0.336633075974744));
#39930=CARTESIAN_POINT('Ctrl Pts',(-0.125317241967218,0.0597826296242031,
-0.328755439975358));
#39931=CARTESIAN_POINT('Ctrl Pts',(-0.118744957590436,-0.0719583837082228,
-0.320877803975976));
#39932=CARTESIAN_POINT('Ctrl Pts',(-0.00500438172789432,-0.138756369592802,
-0.31300016797659));
#39933=CARTESIAN_POINT('Ctrl Pts',(0.113252689408266,-0.0803256016526085,
-0.305122531977208));
#39934=CARTESIAN_POINT('Ctrl Pts',(0.12929828583138,0.0505996760870913,
-0.297244895977823));
#39935=CARTESIAN_POINT('Ctrl Pts',(0.0286511260671305,0.135858333988494,
-0.289367259978439));
#39936=CARTESIAN_POINT('Ctrl Pts',(-0.0978539083562148,0.0985037388046721,
-0.281489623979056));
#39937=CARTESIAN_POINT('Ctrl Pts',(-0.136044993399579,-0.0277512830322524,
-0.273611987979671));
#39938=CARTESIAN_POINT('Ctrl Pts',(-0.0514543637190464,-0.128960545878442,
-0.265734351980287));
#39939=CARTESIAN_POINT('Ctrl Pts',(0.0795742483504507,-0.113781865596983,
-0.257856715980903));
#39940=CARTESIAN_POINT('Ctrl Pts',(0.138786453094293,0.00408587522045665,
-0.249979079981519));
#39941=CARTESIAN_POINT('Ctrl Pts',(0.0727427534113967,0.118266080365061,
-0.242101443982136));
#39942=CARTESIAN_POINT('Ctrl Pts',(-0.0589518737717736,0.125710184628324,
-0.234223807982751));
#39943=CARTESIAN_POINT('Ctrl Pts',(-0.137441954660273,0.0196998232527949,
-0.226346171983368));
#39944=CARTESIAN_POINT('Ctrl Pts',(-0.0918895519293831,-0.104089789049232,
-0.218468535983983));
#39945=CARTESIAN_POINT('Ctrl Pts',(0.0365939199639361,-0.133937518903554,
-0.210590899984599));
#39946=CARTESIAN_POINT('Ctrl Pts',(0.132051080927517,-0.0429055468321947,
-0.202713263985216));
#39947=CARTESIAN_POINT('Ctrl Pts',(0.108331065856659,0.0868490305592283,
-0.194835627985831));
#39948=CARTESIAN_POINT('Ctrl Pts',(-0.0131586188681242,0.138221650789034,
-0.186957991986448));
#39949=CARTESIAN_POINT('Ctrl Pts',(-0.122772542334386,0.0648481045786531,
-0.179080355987064));
#39950=CARTESIAN_POINT('Ctrl Pts',(-0.121583247309369,-0.0670513829332748,
-0.17120271998768));
#39951=CARTESIAN_POINT('Ctrl Pts',(-0.0106640792440769,-0.138436453663531,
-0.163325083988296));
#39952=CARTESIAN_POINT('Ctrl Pts',(0.10987950347526,-0.0848814925592979,
-0.155447447988912));
#39953=CARTESIAN_POINT('Ctrl Pts',(0.13125594634982,0.04527969798971,-0.147569811989528));
#39954=CARTESIAN_POINT('Ctrl Pts',(0.0341728150085339,0.134575609384171,
-0.139692175990144));
#39955=CARTESIAN_POINT('Ctrl Pts',(-0.0937515346592391,0.102415904579156,
-0.13181453999076));
#39956=CARTESIAN_POINT('Ctrl Pts',(-0.137064409224776,-0.0221749265765932,
-0.123936903991376));
#39957=CARTESIAN_POINT('Ctrl Pts',(-0.0566754456467214,-0.126752823243337,
-0.116059267991992));
#39958=CARTESIAN_POINT('Ctrl Pts',(0.0748633938659991,-0.116935041440705,
-0.108181631992608));
#39959=CARTESIAN_POINT('Ctrl Pts',(0.138837743882996,-0.00158285589939853,
-0.100303995993224));
#39960=CARTESIAN_POINT('Ctrl Pts',(0.077509265915822,0.115198674926568,
-0.0924263599938399));
#39961=CARTESIAN_POINT('Ctrl Pts',(-0.0537707528995959,0.128010933958857,
-0.0845487239944558));
#39962=CARTESIAN_POINT('Ctrl Pts',(-0.136524514803491,0.0252951878539005,
-0.0766710879950718));
#39963=CARTESIAN_POINT('Ctrl Pts',(-0.0960594476464373,-0.1002551914902,
-0.068793451995688));
#39964=CARTESIAN_POINT('Ctrl Pts',(0.0310918033177442,-0.135313955894808,
-0.0609158159963039));
#39965=CARTESIAN_POINT('Ctrl Pts',(0.13019812432102,-0.0482707014283373,
-0.0530381799969201));
#39966=CARTESIAN_POINT('Ctrl Pts',(0.111769783231296,0.0823751383704014,
-0.045160543997536));
#39967=CARTESIAN_POINT('Ctrl Pts',(-0.00747498868383688,0.138604580907157,
-0.037282907998152));
#39968=CARTESIAN_POINT('Ctrl Pts',(-0.120082141870022,0.0698809680050969,
-0.0294052719987681));
#39969=CARTESIAN_POINT('Ctrl Pts',(-0.12410032159439,-0.0621879015683824,
-0.0215276359993841));
#39970=CARTESIAN_POINT('Ctrl Pts',(-0.0524255658063026,-0.112395963227031,
-0.0162758786664614));
#39971=CARTESIAN_POINT('Ctrl Pts',(-0.0138313775859342,-0.116960008631478,
-0.0136500000000001));
#39972=CARTESIAN_POINT('Ctrl Pts',(0.112054873528428,-0.0604069144926977,
-0.748648522628062));
#39973=CARTESIAN_POINT('Ctrl Pts',(0.131987804921145,-0.0234313112025849,
-0.746022643961601));
#39974=CARTESIAN_POINT('Ctrl Pts',(0.132089339110787,0.0711567069944395,
-0.740770886628678));
#39975=CARTESIAN_POINT('Ctrl Pts',(0.0127638146478229,0.149628423801929,
-0.732893250629295));
#39976=CARTESIAN_POINT('Ctrl Pts',(-0.117968844989016,0.0926979721019815,
-0.72501561462991));
#39977=CARTESIAN_POINT('Ctrl Pts',(-0.142288901788669,-0.0477109186531712,
-0.717137978630527));
#39978=CARTESIAN_POINT('Ctrl Pts',(-0.0381634497602026,-0.145155302253716,
-0.709260342631142));
#39979=CARTESIAN_POINT('Ctrl Pts',(0.100389818643955,-0.111545957392173,
-0.701382706631759));
#39980=CARTESIAN_POINT('Ctrl Pts',(0.148348351005212,0.0227082782526056,
-0.693505070632373));
#39981=CARTESIAN_POINT('Ctrl Pts',(0.062417134454038,0.136481919947811,
-0.685627434632992));
#39982=CARTESIAN_POINT('Ctrl Pts',(-0.0798438681562896,0.127072247341361,
-0.677749798633605));
#39983=CARTESIAN_POINT('Ctrl Pts',(-0.15004628007042,0.00298266283991623,
-0.669872162634224));
#39984=CARTESIAN_POINT('Ctrl Pts',(-0.0848300963236339,-0.123800813194796,
-0.661994526634838));
#39985=CARTESIAN_POINT('Ctrl Pts',(0.0569456215650577,-0.138851986801525,
-0.654116890635456));
#39986=CARTESIAN_POINT('Ctrl Pts',(0.147327619923948,-0.0285886692416235,
-0.64623925463607));
#39987=CARTESIAN_POINT('Ctrl Pts',(0.104745152897256,0.107476448868313,
-0.638361618636687));
#39988=CARTESIAN_POINT('Ctrl Pts',(-0.032370621355452,0.146543041823854,
-0.630483982637303));
#39989=CARTESIAN_POINT('Ctrl Pts',(-0.140271670621378,0.0533534272010589,
-0.622606346637919));
#39990=CARTESIAN_POINT('Ctrl Pts',(-0.121576381662491,-0.0879881328966351,
-0.614728710638534));
#39991=CARTESIAN_POINT('Ctrl Pts',(0.0068425752925302,-0.149919663789601,
-0.606851074639151));
#39992=CARTESIAN_POINT('Ctrl Pts',(0.12908605587639,-0.0765474887766799,
-0.598973438639767));
#39993=CARTESIAN_POINT('Ctrl Pts',(0.134828317658009,0.0659094246345719,
-0.591095802640382));
#39994=CARTESIAN_POINT('Ctrl Pts',(0.0188869254711551,0.148882542148034,
-0.583218166641));
#39995=CARTESIAN_POINT('Ctrl Pts',(-0.114100071320851,0.0974879543509301,
-0.575340530641614));
#39996=CARTESIAN_POINT('Ctrl Pts',(-0.14411082404738,-0.0418903072657999,
-0.567462894642231));
#39997=CARTESIAN_POINT('Ctrl Pts',(-0.0440603843322313,-0.143462224870114,
-0.559585258642847));
#39998=CARTESIAN_POINT('Ctrl Pts',(0.0957549112211459,-0.115558316181665,
-0.551707622643463));
#39999=CARTESIAN_POINT('Ctrl Pts',(0.14915061936705,0.016637914296508,-0.543829986644079));
#40000=CARTESIAN_POINT('Ctrl Pts',(0.0679366786195117,0.133818291524789,
-0.535952350644695));
#40001=CARTESIAN_POINT('Ctrl Pts',(-0.0745906679847724,0.130226570645529,
-0.528074714645311));
#40002=CARTESIAN_POINT('Ctrl Pts',(-0.149799329134024,0.00910430895317851,
-0.520197078645927));
#40003=CARTESIAN_POINT('Ctrl Pts',(-0.0898128755229932,-0.120234665720163,
-0.512319442646543));
#40004=CARTESIAN_POINT('Ctrl Pts',(0.0512304298375893,-0.14106087519131,
-0.504441806647159));
#40005=CARTESIAN_POINT('Ctrl Pts',(0.146037854961359,-0.0345784957603811,
-0.496564170647776));
#40006=CARTESIAN_POINT('Ctrl Pts',(0.109044926402886,0.103111257758742,
-0.488686534648391));
#40007=CARTESIAN_POINT('Ctrl Pts',(-0.0263619364813165,0.147742261238358,
-0.480808898649007));
#40008=CARTESIAN_POINT('Ctrl Pts',(-0.13797693695467,0.0590346704863042,
-0.472931262649624));
#40009=CARTESIAN_POINT('Ctrl Pts',(-0.125066627908228,-0.0829521912579385,
-0.465053626650239));
#40010=CARTESIAN_POINT('Ctrl Pts',(0.000717331580232957,-0.150074024688621,
-0.457175990650856));
#40011=CARTESIAN_POINT('Ctrl Pts',(0.12585389347435,-0.0817528283802863,
-0.449298354651471));
#40012=CARTESIAN_POINT('Ctrl Pts',(0.13740629134024,0.0603509614749642,
-0.441420718652087));
#40013=CARTESIAN_POINT('Ctrl Pts',(0.0249483920015943,0.147987516998452,
-0.433543082652704));
#40014=CARTESIAN_POINT('Ctrl Pts',(-0.110025634340521,0.10206413296941,
-0.42566544665332));
#40015=CARTESIAN_POINT('Ctrl Pts',(-0.145700629454878,-0.0359729624479837,
-0.417787810653936));
#40016=CARTESIAN_POINT('Ctrl Pts',(-0.0498796196530811,-0.141544166231236,
-0.409910174654552));
#40017=CARTESIAN_POINT('Ctrl Pts',(0.0909581531898705,-0.119370607014959,
-0.402032538655167));
#40018=CARTESIAN_POINT('Ctrl Pts',(0.149705451861443,0.0105358973890694,
-0.394154902655784));
#40019=CARTESIAN_POINT('Ctrl Pts',(0.0733423607728681,0.130933668577239,
-0.386277266656399));
#40020=CARTESIAN_POINT('Ctrl Pts',(-0.0692128083378411,0.133162737328507,
-0.378399630657016));
#40021=CARTESIAN_POINT('Ctrl Pts',(-0.149302854137109,0.0152113509375375,
-0.370521994657631));
#40022=CARTESIAN_POINT('Ctrl Pts',(-0.0946458579018804,-0.11646840358161,
-0.362644358658248));
#40023=CARTESIAN_POINT('Ctrl Pts',(0.0454297960462407,-0.143034475152072,
-0.354766722658863));
#40024=CARTESIAN_POINT('Ctrl Pts',(0.144504689005293,-0.040510767782347,
-0.34688908665948));
#40025=CARTESIAN_POINT('Ctrl Pts',(0.11316292304571,0.0985742374993713,
-0.339011450660095));
#40026=CARTESIAN_POINT('Ctrl Pts',(-0.0203093027534662,0.148695190482071,
-0.331133814660713));
#40027=CARTESIAN_POINT('Ctrl Pts',(-0.135452217384223,0.0646175228287937,
-0.323256178661327));
#40028=CARTESIAN_POINT('Ctrl Pts',(-0.128348402473042,-0.0777779855322154,
-0.315378542661945));
#40029=CARTESIAN_POINT('Ctrl Pts',(-0.00540910884280258,-0.149978228394512,
-0.30750090666256));
#40030=CARTESIAN_POINT('Ctrl Pts',(0.122411949579047,-0.0868218984536377,
-0.299623270663176));
#40031=CARTESIAN_POINT('Ctrl Pts',(0.139755226375163,0.0546919020665389,
-0.291745634663792));
#40032=CARTESIAN_POINT('Ctrl Pts',(0.0309682729640912,0.146845815467929,
-0.283867998664408));
#40033=CARTESIAN_POINT('Ctrl Pts',(-0.105767799055369,0.106470184248226,
-0.275990362665024));
#40034=CARTESIAN_POINT('Ctrl Pts',(-0.147047570874689,-0.0299956555296591,
-0.26811272666564));
#40035=CARTESIAN_POINT('Ctrl Pts',(-0.0556157121752046,-0.139390171855875,
-0.260235090666256));
#40036=CARTESIAN_POINT('Ctrl Pts',(0.0860097797920805,-0.12298392265333,
-0.252357454666872));
#40037=CARTESIAN_POINT('Ctrl Pts',(0.150010744885616,0.00441631853588612,
-0.244479818667488));
#40038=CARTESIAN_POINT('Ctrl Pts',(0.0786257907813281,0.127830796268072,
-0.236602182668104));
#40039=CARTESIAN_POINT('Ctrl Pts',(-0.0637195799715275,0.135876939105801,
-0.22872454666872));
#40040=CARTESIAN_POINT('Ctrl Pts',(-0.148557510747211,0.0212930375723279,
-0.220846910669336));
#40041=CARTESIAN_POINT('Ctrl Pts',(-0.0993210779928724,-0.112508003786603,
-0.212969274669952));
#40042=CARTESIAN_POINT('Ctrl Pts',(0.0395534367345272,-0.14476965532942,
-0.205091638670569));
#40043=CARTESIAN_POINT('Ctrl Pts',(0.14273065253299,-0.0463755135787604,
-0.197214002671184));
#40044=CARTESIAN_POINT('Ctrl Pts',(0.11709229194271,0.0938729067305426,
-0.189336366671801));
#40045=CARTESIAN_POINT('Ctrl Pts',(-0.0142228162335986,0.149400264448687,
-0.181458730672416));
#40046=CARTESIAN_POINT('Ctrl Pts',(-0.132701716316428,0.070092665785291,
-0.173581094673032));
#40047=CARTESIAN_POINT('Ctrl Pts',(-0.131416237592721,-0.0724741332830037,
-0.165703458673648));
#40048=CARTESIAN_POINT('Ctrl Pts',(-0.0115265318426756,-0.149632439408767,
-0.157825822674264));
#40049=CARTESIAN_POINT('Ctrl Pts',(0.118765958755258,-0.0917462449823706,
-0.14994818667488));
#40050=CARTESIAN_POINT('Ctrl Pts',(0.141871211804985,0.0489416731402246,
-0.142070550675496));
#40051=CARTESIAN_POINT('Ctrl Pts',(0.0369365260079516,0.145459351089831,
-0.134192914676113));
#40052=CARTESIAN_POINT('Ctrl Pts',(-0.101333647736116,0.110698744665053,
-0.126315278676728));
#40053=CARTESIAN_POINT('Ctrl Pts',(-0.148149431494919,-0.0239683137609865,
-0.118437642677345));
#40054=CARTESIAN_POINT('Ctrl Pts',(-0.0612590467486968,-0.137003900648497,
-0.110560006677961));
#40055=CARTESIAN_POINT('Ctrl Pts',(0.0809179370761331,-0.126392110171104,
-0.102682370678577));
#40056=CARTESIAN_POINT('Ctrl Pts',(0.15006618379372,-0.00171086865628145,
-0.0948047346791928));
#40057=CARTESIAN_POINT('Ctrl Pts',(0.0837777928345086,0.124515315798361,
-0.0869270986798086));
#40058=CARTESIAN_POINT('Ctrl Pts',(-0.0581194382858709,0.138363760500637,
-0.0790494626804247));
#40059=CARTESIAN_POINT('Ctrl Pts',(-0.147565873355843,0.0273409247616357,
-0.0711718266810408));
#40060=CARTESIAN_POINT('Ctrl Pts',(-0.10382821214512,-0.108363284879664,
-0.0632941906816567));
#40061=CARTESIAN_POINT('Ctrl Pts',(0.033606338886425,-0.14625741104147,
-0.0554165546822729));
#40062=CARTESIAN_POINT('Ctrl Pts',(0.14072783889676,-0.0521745726327952,
-0.0475389186828887));
#40063=CARTESIAN_POINT('Ctrl Pts',(0.120809114033913,0.0890371905289917,
-0.0396612826835049));
#40064=CARTESIAN_POINT('Ctrl Pts',(-0.00807952502188328,0.149814163867383,
-0.0317836466841208));
#40065=CARTESIAN_POINT('Ctrl Pts',(-0.129793730928073,0.075532559771165,
-0.0239060106847369));
#40066=CARTESIAN_POINT('Ctrl Pts',(-0.134136879125162,-0.0672173200565058,
-0.0160283746853529));
#40067=CARTESIAN_POINT('Ctrl Pts',(-0.0566654597931856,-0.121485936054349,
-0.0107766173524302));
#40068=CARTESIAN_POINT('Ctrl Pts',(-0.014949984009251,-0.126419096572168,
-0.00815073868596886));
#40069=CARTESIAN_POINT('Ctrl Pts',(0.12043918358623,-0.0649267562880083,
-0.743149261314031));
#40070=CARTESIAN_POINT('Ctrl Pts',(0.141863561730838,-0.0251845181091421,
-0.74052338264757));
#40071=CARTESIAN_POINT('Ctrl Pts',(0.141972693038755,0.0764808832247766,
-0.735271625314647));
#40072=CARTESIAN_POINT('Ctrl Pts',(0.0137188447697446,0.160824109086401,
-0.727393989315264));
#40073=CARTESIAN_POINT('Ctrl Pts',(-0.126795657624682,0.0996339358433128,
-0.719516353315879));
#40074=CARTESIAN_POINT('Ctrl Pts',(-0.152935420166808,-0.0512808047503536,
-0.711638717316496));
#40075=CARTESIAN_POINT('Ctrl Pts',(-0.0410189631849163,-0.156016294036643,
-0.703761081317111));
#40076=CARTESIAN_POINT('Ctrl Pts',(0.107901311358673,-0.119892188689585,
-0.695883445317728));
#40077=CARTESIAN_POINT('Ctrl Pts',(0.159448257080032,0.0244073854824245,
-0.688005809318343));
#40078=CARTESIAN_POINT('Ctrl Pts',(0.0670873874444137,0.146693941059381,
-0.68012817331896));
#40079=CARTESIAN_POINT('Ctrl Pts',(-0.0858180460367966,0.136580206146754,
-0.672250537319575));
#40080=CARTESIAN_POINT('Ctrl Pts',(-0.161273230719836,0.00320583537369734,
-0.664372901320192));
#40081=CARTESIAN_POINT('Ctrl Pts',(-0.0911773600116365,-0.133063992658113,
-0.656495265320807));
#40082=CARTESIAN_POINT('Ctrl Pts',(0.0612064781668413,-0.149241344022927,
-0.648617629321424));
#40083=CARTESIAN_POINT('Ctrl Pts',(0.158351151579687,-0.0307277664492165,
-0.640739993322038));
#40084=CARTESIAN_POINT('Ctrl Pts',(0.112582525885052,0.115518186303275,
-0.632862357322657));
#40085=CARTESIAN_POINT('Ctrl Pts',(-0.0347926965197141,0.157507868794571,
-0.624984721323271));
#40086=CARTESIAN_POINT('Ctrl Pts',(-0.15076725320322,0.0573455041381383,
-0.617107085323888));
#40087=CARTESIAN_POINT('Ctrl Pts',(-0.130673121924355,-0.0945716911514688,
-0.609229449324504));
#40088=CARTESIAN_POINT('Ctrl Pts',(0.00735455902906769,-0.16113714059711,
-0.60135181332512));
#40089=CARTESIAN_POINT('Ctrl Pts',(0.138744694385601,-0.0822750208316521,
-0.593474177325735));
#40090=CARTESIAN_POINT('Ctrl Pts',(0.144916610868477,0.0708409821337405,
-0.585596541326352));
#40091=CARTESIAN_POINT('Ctrl Pts',(0.0203001066582162,0.160022418141436,
-0.577718905326968));
#40092=CARTESIAN_POINT('Ctrl Pts',(-0.122637409728793,0.104782320141917,
-0.569841269327584));
#40093=CARTESIAN_POINT('Ctrl Pts',(-0.154893664574099,-0.0450246762894181,
-0.5619636333282));
#40094=CARTESIAN_POINT('Ctrl Pts',(-0.0473571255794006,-0.154196535097041,
-0.554085997328815));
#40095=CARTESIAN_POINT('Ctrl Pts',(0.102919605089028,-0.12420476521254,
-0.546208361329432));
#40096=CARTESIAN_POINT('Ctrl Pts',(0.160310553769808,0.0178828171533352,
-0.538330725330049));
#40097=CARTESIAN_POINT('Ctrl Pts',(0.0730199218547905,0.143831011295202,
-0.530453089330663));
#40098=CARTESIAN_POINT('Ctrl Pts',(-0.0801717843441979,0.139970546178904,
-0.52257545333128));
#40099=CARTESIAN_POINT('Ctrl Pts',(-0.161007802111255,0.00978552295772822,
-0.514697817331896));
#40100=CARTESIAN_POINT('Ctrl Pts',(-0.0965329669554883,-0.129231014431746,
-0.506820181332512));
#40101=CARTESIAN_POINT('Ctrl Pts',(0.0550636572076045,-0.151615508625695,
-0.498942545333128));
#40102=CARTESIAN_POINT('Ctrl Pts',(0.156964882208075,-0.0371657712679834,
-0.491064909333744));
#40103=CARTESIAN_POINT('Ctrl Pts',(0.117204022427926,0.110826377398585,
-0.48318727333436));
#40104=CARTESIAN_POINT('Ctrl Pts',(-0.0283344223020895,0.158796817705721,
-0.475309637334976));
#40105=CARTESIAN_POINT('Ctrl Pts',(-0.148300820100728,0.0634518365222992,
-0.467432001335592));
#40106=CARTESIAN_POINT('Ctrl Pts',(-0.134424519745038,-0.0891589439816757,
-0.459554365336208));
#40107=CARTESIAN_POINT('Ctrl Pts',(0.000771004661942072,-0.161303051280602,
-0.451676729336824));
#40108=CARTESIAN_POINT('Ctrl Pts',(0.13527069108113,-0.087869840872999,
-0.44379909333744));
#40109=CARTESIAN_POINT('Ctrl Pts',(0.147687476925596,0.0648666166835182,
-0.435921457338057));
#40110=CARTESIAN_POINT('Ctrl Pts',(0.0268151118273235,0.159060424299397,
-0.428043821338672));
#40111=CARTESIAN_POINT('Ctrl Pts',(-0.118258110122872,0.109700903327099,
-0.420166185339288));
#40112=CARTESIAN_POINT('Ctrl Pts',(-0.156602424392488,-0.0386645764881796,
-0.412288549339904));
#40113=CARTESIAN_POINT('Ctrl Pts',(-0.0536117750120421,-0.152134961072968,
-0.404410913340521));
#40114=CARTESIAN_POINT('Ctrl Pts',(0.0977639380220263,-0.128302304044162,
-0.396533277341136));
#40115=CARTESIAN_POINT('Ctrl Pts',(0.160906900635836,0.0113242274961454,
-0.388655641341753));
#40116=CARTESIAN_POINT('Ctrl Pts',(0.0788300747270055,0.14073055147746,
-0.380778005342368));
#40117=CARTESIAN_POINT('Ctrl Pts',(-0.0743915357488216,0.143126406401988,
-0.372900369342985));
#40118=CARTESIAN_POINT('Ctrl Pts',(-0.160474179240455,0.0163495136844361,
-0.3650227333436));
#40119=CARTESIAN_POINT('Ctrl Pts',(-0.101727568793597,-0.125182948311499,
-0.357145097344217));
#40120=CARTESIAN_POINT('Ctrl Pts',(0.0488290011313963,-0.153736779753985,
-0.349267461344832));
#40121=CARTESIAN_POINT('Ctrl Pts',(0.155316999789075,-0.043541915175332,
-0.341389825345449));
#40122=CARTESIAN_POINT('Ctrl Pts',(0.121630140971951,0.105949882528291,
-0.333512189346064));
#40123=CARTESIAN_POINT('Ctrl Pts',(-0.0218289108345867,0.159821048214528,
-0.325634553346681));
#40124=CARTESIAN_POINT('Ctrl Pts',(-0.145587192801227,0.0694524160333842,
-0.317756917347296));
#40125=CARTESIAN_POINT('Ctrl Pts',(-0.137951847355649,-0.0835975873562079,
-0.309879281347913));
#40126=CARTESIAN_POINT('Ctrl Pts',(-0.00581383595771093,-0.161200087196222,
-0.302001645348528));
#40127=CARTESIAN_POINT('Ctrl Pts',(0.131571209749827,-0.0933181952546669,
-0.294124009349145));
#40128=CARTESIAN_POINT('Ctrl Pts',(0.150212166918945,0.0587841280459866,
-0.28624637334976));
#40129=CARTESIAN_POINT('Ctrl Pts',(0.033285419861052,0.157833296947363,
-0.278368737350377));
#40130=CARTESIAN_POINT('Ctrl Pts',(-0.113681689754523,0.114436629691781,
-0.270491101350993));
#40131=CARTESIAN_POINT('Ctrl Pts',(-0.158050148349798,-0.0322400280270659,
-0.262613465351609));
#40132=CARTESIAN_POINT('Ctrl Pts',(-0.059777060631363,-0.149819797833307,
-0.254735829352225));
#40133=CARTESIAN_POINT('Ctrl Pts',(0.0924453112337102,-0.132185979709678,
-0.246858193352841));
#40134=CARTESIAN_POINT('Ctrl Pts',(0.16123503667694,0.00474676185131575,
-0.238980557353457));
#40135=CARTESIAN_POINT('Ctrl Pts',(0.0845088281512594,0.137395512171083,
-0.231102921354073));
#40136=CARTESIAN_POINT('Ctrl Pts',(-0.0684872861712815,0.146043693583278,
-0.223225285354689));
#40137=CARTESIAN_POINT('Ctrl Pts',(-0.159673066834149,0.022886251891861,
-0.215347649355305));
#40138=CARTESIAN_POINT('Ctrl Pts',(-0.106752604056362,-0.120926218523974,
-0.207470013355921));
#40139=CARTESIAN_POINT('Ctrl Pts',(0.0425129535051184,-0.155601791755286,
-0.199592377356537));
#40140=CARTESIAN_POINT('Ctrl Pts',(0.153410224138463,-0.0498454803253261,
-0.191714741357153));
#40141=CARTESIAN_POINT('Ctrl Pts',(0.125853518028762,0.100896782901857,
-0.183837105357769));
#40142=CARTESIAN_POINT('Ctrl Pts',(-0.0152870135990733,0.160578878108339,
-0.175959469358385));
#40143=CARTESIAN_POINT('Ctrl Pts',(-0.14263089029847,0.075337226991929,
-0.168081833359001));
#40144=CARTESIAN_POINT('Ctrl Pts',(-0.141249227876074,-0.0778968836327328,
-0.160204197359617));
#40145=CARTESIAN_POINT('Ctrl Pts',(-0.0123889844412741,-0.160828425154002,
-0.152326561360233));
#40146=CARTESIAN_POINT('Ctrl Pts',(0.127652414035256,-0.0986109974054438,
-0.144448925360849));
#40147=CARTESIAN_POINT('Ctrl Pts',(0.15248647726015,0.0526036482907394,
-0.136571289361465));
#40148=CARTESIAN_POINT('Ctrl Pts',(0.0397002370073691,0.156343092795492,
-0.128693653362081));
#40149=CARTESIAN_POINT('Ctrl Pts',(-0.108915760812993,0.118981584750951,
-0.120816017362697));
#40150=CARTESIAN_POINT('Ctrl Pts',(-0.159234453765061,-0.0257617009453798,
-0.112938381363313));
#40151=CARTESIAN_POINT('Ctrl Pts',(-0.065842647850672,-0.147254978053657,
-0.105060745363929));
#40152=CARTESIAN_POINT('Ctrl Pts',(0.0869724802862671,-0.135849178901503,
-0.0971831093645453));
#40153=CARTESIAN_POINT('Ctrl Pts',(0.161294623704445,-0.00183888141316458,
-0.0893054733651615));
#40154=CARTESIAN_POINT('Ctrl Pts',(0.090046319753195,0.133831956670155,
-0.0814278373657774));
#40155=CARTESIAN_POINT('Ctrl Pts',(-0.0624681236721457,0.148716587042417,
-0.0735502013663936));
#40156=CARTESIAN_POINT('Ctrl Pts',(-0.158607231908194,0.029386661669371,
-0.0656725653670094));
#40157=CARTESIAN_POINT('Ctrl Pts',(-0.111596976643804,-0.116471378269128,
-0.0577949293676256));
#40158=CARTESIAN_POINT('Ctrl Pts',(0.0361208744551059,-0.157200866188131,
-0.0499172933682415));
#40159=CARTESIAN_POINT('Ctrl Pts',(0.151257553472499,-0.0560784438372532,
-0.0420396573688577));
#40160=CARTESIAN_POINT('Ctrl Pts',(0.129848444836529,0.0956992426875821,
-0.0341620213694736));
#40161=CARTESIAN_POINT('Ctrl Pts',(-0.00868406135992968,0.161023746827609,
-0.0262843853700897));
#40162=CARTESIAN_POINT('Ctrl Pts',(-0.139505319986123,0.081184151537233,
-0.0184067493707057));
#40163=CARTESIAN_POINT('Ctrl Pts',(-0.144173436655933,-0.0722467385446291,
-0.0105291133713217));
#40164=CARTESIAN_POINT('Ctrl Pts',(-0.0609053537800685,-0.130575908881668,
-0.00527735603839902));
#40165=CARTESIAN_POINT('Ctrl Pts',(-0.0160685904325677,-0.135878184512858,
-0.00265147737193768));
#40166=CARTESIAN_POINT('Ctrl Pts',(0.128823493644032,-0.0694465980833189,
-0.73765));
#40167=CARTESIAN_POINT('Ctrl Pts',(0.15173931854053,-0.0269377250156994,
-0.735024121333539));
#40168=CARTESIAN_POINT('Ctrl Pts',(0.151856046966723,0.0818050594551139,
-0.729772364000616));
#40169=CARTESIAN_POINT('Ctrl Pts',(0.0146738748916663,0.172019794370874,
-0.721894728001232));
#40170=CARTESIAN_POINT('Ctrl Pts',(-0.135622470260348,0.106569899584644,
-0.714017092001848));
#40171=CARTESIAN_POINT('Ctrl Pts',(-0.163581938544947,-0.0548506908475362,
-0.706139456002465));
#40172=CARTESIAN_POINT('Ctrl Pts',(-0.04387447660963,-0.16687728581957,
-0.698261820003079));
#40173=CARTESIAN_POINT('Ctrl Pts',(0.115412804073391,-0.128238419986997,
-0.690384184003697));
#40174=CARTESIAN_POINT('Ctrl Pts',(0.170548163154853,0.0261064927122433,
-0.682506548004312));
#40175=CARTESIAN_POINT('Ctrl Pts',(0.0717576404347894,0.156905962170951,
-0.674628912004929));
#40176=CARTESIAN_POINT('Ctrl Pts',(-0.0917922239173038,0.146088164952146,
-0.666751276005544));
#40177=CARTESIAN_POINT('Ctrl Pts',(-0.172500181369253,0.00342900790747846,
-0.65887364000616));
#40178=CARTESIAN_POINT('Ctrl Pts',(-0.0975246236996389,-0.142327172121431,
-0.650996004006776));
#40179=CARTESIAN_POINT('Ctrl Pts',(0.0654673347686249,-0.15963070124433,
-0.643118368007393));
#40180=CARTESIAN_POINT('Ctrl Pts',(0.169374683235426,-0.0328668636568096,
-0.635240732008008));
#40181=CARTESIAN_POINT('Ctrl Pts',(0.120419898872848,0.123559923738236,
-0.627363096008626));
#40182=CARTESIAN_POINT('Ctrl Pts',(-0.037214771683976,0.168472695765287,
-0.619485460009239));
#40183=CARTESIAN_POINT('Ctrl Pts',(-0.161262835785063,0.0613375810752176,
-0.611607824009858));
#40184=CARTESIAN_POINT('Ctrl Pts',(-0.139769862186219,-0.101155249406303,
-0.603730188010472));
#40185=CARTESIAN_POINT('Ctrl Pts',(0.00786654276560517,-0.17235461740462,
-0.595852552011089));
#40186=CARTESIAN_POINT('Ctrl Pts',(0.148403332894812,-0.0880025528866245,
-0.587974916011704));
#40187=CARTESIAN_POINT('Ctrl Pts',(0.155004904078945,0.0757725396329093,
-0.580097280012322));
#40188=CARTESIAN_POINT('Ctrl Pts',(0.0217132878452772,0.171162294134837,
-0.572219644012935));
#40189=CARTESIAN_POINT('Ctrl Pts',(-0.131174748136735,0.112076685932905,
-0.564342008013554));
#40190=CARTESIAN_POINT('Ctrl Pts',(-0.165676505100818,-0.0481590453130367,
-0.556464372014167));
#40191=CARTESIAN_POINT('Ctrl Pts',(-0.0506538668265696,-0.164930845323967,
-0.548586736014785));
#40192=CARTESIAN_POINT('Ctrl Pts',(0.110084298956909,-0.132851214243416,
-0.5407091000154));
#40193=CARTESIAN_POINT('Ctrl Pts',(0.171470488172567,0.0191277200101626,
-0.532831464016017));
#40194=CARTESIAN_POINT('Ctrl Pts',(0.0781031650900689,0.153843731065615,
-0.524953828016632));
#40195=CARTESIAN_POINT('Ctrl Pts',(-0.0857529007036231,0.14971452171228,
-0.51707619201725));
#40196=CARTESIAN_POINT('Ctrl Pts',(-0.172216275088487,0.0104667369622776,
-0.509198556017864));
#40197=CARTESIAN_POINT('Ctrl Pts',(-0.103253058387983,-0.138227363143328,
-0.501320920018481));
#40198=CARTESIAN_POINT('Ctrl Pts',(0.0588968845776194,-0.162170142060081,
-0.493443284019097));
#40199=CARTESIAN_POINT('Ctrl Pts',(0.16789190945479,-0.0397530467755856,
-0.485565648019713));
#40200=CARTESIAN_POINT('Ctrl Pts',(0.125363118452966,0.118541497038427,
-0.477688012020329));
#40201=CARTESIAN_POINT('Ctrl Pts',(-0.0303069081228627,0.169851374173085,
-0.469810376020944));
#40202=CARTESIAN_POINT('Ctrl Pts',(-0.158624703246786,0.0678690025582943,
-0.461932740021561));
#40203=CARTESIAN_POINT('Ctrl Pts',(-0.143782411581849,-0.095365696705413,
-0.454055104022176));
#40204=CARTESIAN_POINT('Ctrl Pts',(0.000824677743651456,-0.172532077872582,
-0.446177468022794));
#40205=CARTESIAN_POINT('Ctrl Pts',(0.14468748868791,-0.0939868533657117,
-0.438299832023408));
#40206=CARTESIAN_POINT('Ctrl Pts',(0.157968662510953,0.0693822718920721,
-0.430422196024026));
#40207=CARTESIAN_POINT('Ctrl Pts',(0.0286818316530525,0.170133331600341,
-0.42254456002464));
#40208=CARTESIAN_POINT('Ctrl Pts',(-0.126490585905224,0.117337673684787,
-0.414666924025258));
#40209=CARTESIAN_POINT('Ctrl Pts',(-0.167504219330098,-0.0413561905283752,
-0.406789288025872));
#40210=CARTESIAN_POINT('Ctrl Pts',(-0.057343930371003,-0.1627257559147,
-0.39891165202649));
#40211=CARTESIAN_POINT('Ctrl Pts',(0.104569722854182,-0.137234001073365,
-0.391034016027105));
#40212=CARTESIAN_POINT('Ctrl Pts',(0.172108349410229,0.0121125576032212,
-0.383156380027722));
#40213=CARTESIAN_POINT('Ctrl Pts',(0.0843177886811427,0.150527434377681,
-0.375278744028337));
#40214=CARTESIAN_POINT('Ctrl Pts',(-0.079570263159802,0.153090075475469,
-0.367401108028953));
#40215=CARTESIAN_POINT('Ctrl Pts',(-0.171645504343801,0.0174876764313346,
-0.359523472029569));
#40216=CARTESIAN_POINT('Ctrl Pts',(-0.108809279685313,-0.133897493041387,
-0.351645836030186));
#40217=CARTESIAN_POINT('Ctrl Pts',(0.0522282062165519,-0.164439084355898,
-0.343768200030801));
#40218=CARTESIAN_POINT('Ctrl Pts',(0.166129310572857,-0.046573062568317,
-0.335890564031418));
#40219=CARTESIAN_POINT('Ctrl Pts',(0.130097358898192,0.11332552755721,-0.328012928032033));
#40220=CARTESIAN_POINT('Ctrl Pts',(-0.0233485189157071,0.170946905946985,
-0.32013529203265));
#40221=CARTESIAN_POINT('Ctrl Pts',(-0.155722168218232,0.0742873092379748,
-0.312257656033265));
#40222=CARTESIAN_POINT('Ctrl Pts',(-0.147555292238255,-0.0894171891802003,
-0.304380020033882));
#40223=CARTESIAN_POINT('Ctrl Pts',(-0.00621856307261924,-0.172421945997932,
-0.296502384034497));
#40224=CARTESIAN_POINT('Ctrl Pts',(0.140730469920608,-0.0998144920556959,
-0.288624748035114));
#40225=CARTESIAN_POINT('Ctrl Pts',(0.160669107462727,0.0628763540254339,
-0.280747112035729));
#40226=CARTESIAN_POINT('Ctrl Pts',(0.0356025667580126,0.168820778426797,
-0.272869476036346));
#40227=CARTESIAN_POINT('Ctrl Pts',(-0.121595580453677,0.122403075135335,
-0.264991840036961));
#40228=CARTESIAN_POINT('Ctrl Pts',(-0.169052725824908,-0.0344844005244726,
-0.257114204037578));
#40229=CARTESIAN_POINT('Ctrl Pts',(-0.0639384090875212,-0.16024942381074,
-0.249236568038193));
#40230=CARTESIAN_POINT('Ctrl Pts',(0.0988808426753398,-0.141388036766026,
-0.24135893203881));
#40231=CARTESIAN_POINT('Ctrl Pts',(0.172459328468264,0.00507720516674541,
-0.233481296039426));
#40232=CARTESIAN_POINT('Ctrl Pts',(0.0903918655211907,0.146960228074094,
-0.225603660040042));
#40233=CARTESIAN_POINT('Ctrl Pts',(-0.0732549923710354,0.156210448060755,
-0.217726024040658));
#40234=CARTESIAN_POINT('Ctrl Pts',(-0.170788622921086,0.0244794662113939,
-0.209848388041274));
#40235=CARTESIAN_POINT('Ctrl Pts',(-0.114184130119851,-0.129344433261344,
-0.20197075204189));
#40236=CARTESIAN_POINT('Ctrl Pts',(0.0454724702757093,-0.166433928181152,
-0.194093116042506));
#40237=CARTESIAN_POINT('Ctrl Pts',(0.164089795743936,-0.0533154470718918,
-0.186215480043122));
#40238=CARTESIAN_POINT('Ctrl Pts',(0.134614744114814,0.107920659073171,
-0.178337844043738));
#40239=CARTESIAN_POINT('Ctrl Pts',(-0.0163512109645475,0.171757491767992,
-0.170460208044354));
#40240=CARTESIAN_POINT('Ctrl Pts',(-0.152560064280512,0.0805817881985668,
-0.16258257204497));
#40241=CARTESIAN_POINT('Ctrl Pts',(-0.151082218159426,-0.0833196339824615,
-0.154704936045586));
#40242=CARTESIAN_POINT('Ctrl Pts',(-0.013251437039873,-0.172024410899238,
-0.146827300046202));
#40243=CARTESIAN_POINT('Ctrl Pts',(0.136538869315254,-0.105475749828517,
-0.138949664046818));
#40244=CARTESIAN_POINT('Ctrl Pts',(0.163101742715315,0.056265623441254,
-0.131072028047434));
#40245=CARTESIAN_POINT('Ctrl Pts',(0.0424639480067868,0.167226834501153,
-0.12319439204805));
#40246=CARTESIAN_POINT('Ctrl Pts',(-0.116497873889869,0.127264424836848,
-0.115316756048666));
#40247=CARTESIAN_POINT('Ctrl Pts',(-0.170319476035203,-0.0275550881297732,
-0.107439120049282));
#40248=CARTESIAN_POINT('Ctrl Pts',(-0.0704262489526473,-0.157506055458817,
-0.0995614840498983));
#40249=CARTESIAN_POINT('Ctrl Pts',(0.0930270234964012,-0.145306247631903,
-0.0916838480505141));
#40250=CARTESIAN_POINT('Ctrl Pts',(0.172523063615169,-0.00196689417004758,
-0.0838062120511303));
#40251=CARTESIAN_POINT('Ctrl Pts',(0.0963148466718817,0.143148597541948,
-0.0759285760517462));
#40252=CARTESIAN_POINT('Ctrl Pts',(-0.0668168090584207,0.159069413584198,
-0.0680509400523624));
#40253=CARTESIAN_POINT('Ctrl Pts',(-0.169648590460546,0.0314323985771063,
-0.0601733040529782));
#40254=CARTESIAN_POINT('Ctrl Pts',(-0.119365741142487,-0.124579471658591,
-0.0522956680535945));
#40255=CARTESIAN_POINT('Ctrl Pts',(0.0386354100237868,-0.168144321334793,
-0.0444180320542104));
#40256=CARTESIAN_POINT('Ctrl Pts',(0.161787268048238,-0.059982315041711,
-0.0365403960548265));
#40257=CARTESIAN_POINT('Ctrl Pts',(0.138887775639146,0.102361294846172,
-0.0286627600554425));
#40258=CARTESIAN_POINT('Ctrl Pts',(-0.00928859769797627,0.172233329787836,
-0.0207851240560585));
#40259=CARTESIAN_POINT('Ctrl Pts',(-0.149216909044174,0.0868357433033009,
-0.0129074880566745));
#40260=CARTESIAN_POINT('Ctrl Pts',(-0.154209994186705,-0.0772761570327524,
-0.00502985205729055));
#40261=CARTESIAN_POINT('Ctrl Pts',(-0.0651452477669514,-0.139665881708986,
0.000221905275632163));
#40262=CARTESIAN_POINT('Ctrl Pts',(-0.0171871968558845,-0.145337272453549,
0.00284778394209351));
#40263=CARTESIAN_POINT('Ctrl Pts',(-0.146417921947427,0.000120753153388515,
-0.0587155045842908));
#40264=CARTESIAN_POINT('Ctrl Pts',(-0.146069418978064,-0.0391769882200356,
-0.0565755590740587));
#40265=CARTESIAN_POINT('Ctrl Pts',(-0.129702676035881,-0.0787309748396744,
-0.0544356135638267));
#40266=CARTESIAN_POINT('Ctrl Pts',(-0.101412690834453,-0.10583830156534,
-0.0522956680535946));
#40267=CARTESIAN_POINT('Ctrl Pts',(-0.0666986907537308,-0.139101088217324,
-0.0496697893871332));
#40268=CARTESIAN_POINT('Ctrl Pts',(-0.0140316403649711,-0.153622704776059,
-0.0470439107206718));
#40269=CARTESIAN_POINT('Ctrl Pts',(0.0328271945001503,-0.142856512006579,
-0.0444180320542104));
#40270=CARTESIAN_POINT('Ctrl Pts',(0.0796860293652709,-0.132090319237099,
-0.0417921533877491));
#40271=CARTESIAN_POINT('Ctrl Pts',(0.120736648706754,-0.0960363171394056,
-0.0391662747212878));
#40272=CARTESIAN_POINT('Ctrl Pts',(0.137445376309314,-0.0509520477759113,
-0.0365403960548265));
#40273=CARTESIAN_POINT('Ctrl Pts',(0.154154103911874,-0.00586777841241708,
-0.0339145173883652));
#40274=CARTESIAN_POINT('Ctrl Pts',(0.14652093977551,0.0482467582168783,
-0.0312886387219038));
#40275=CARTESIAN_POINT('Ctrl Pts',(0.118008295484474,0.0869493656884694,
-0.0286627600554425));
#40276=CARTESIAN_POINT('Ctrl Pts',(0.0894956511934385,0.12565197316006,
-0.0260368813889812));
#40277=CARTESIAN_POINT('Ctrl Pts',(0.0401035267477311,0.148942651473948,
-0.0234110027225198));
#40278=CARTESIAN_POINT('Ctrl Pts',(-0.00791392069948822,0.146355059550136,
-0.0207851240560585));
#40279=CARTESIAN_POINT('Ctrl Pts',(-0.0514054509527252,0.144011362864443,
-0.0184067493707056));
#40280=CARTESIAN_POINT('Ctrl Pts',(-0.0937692336261515,0.120437837890111,
-0.0160283746853528));
#40281=CARTESIAN_POINT('Ctrl Pts',(-0.119316161853458,0.0851151957093249,
-0.0136499999999998));
#40282=CARTESIAN_POINT('',(-0.000884750838570857,0.117943724677159,-0.73765));
#40283=CARTESIAN_POINT('Ctrl Pts',(-0.000884750838570857,0.117943724677159,
-0.73765));
#40284=CARTESIAN_POINT('Ctrl Pts',(0.00278616629908432,0.118427354462138,
-0.73765));
#40285=CARTESIAN_POINT('Ctrl Pts',(0.00647167956003039,0.118727197682349,
-0.73765));
#40286=CARTESIAN_POINT('Ctrl Pts',(0.0101595898828385,0.118837906739275,
-0.73765));
#40287=CARTESIAN_POINT('Ctrl Pts',(0.0154982204910781,0.118998169519057,
-0.73765));
#40288=CARTESIAN_POINT('Ctrl Pts',(0.0208418519924889,0.118762501178767,
-0.73765));
#40289=CARTESIAN_POINT('Ctrl Pts',(0.026159529311872,0.118157056568905,
-0.73765));
#40290=CARTESIAN_POINT('Ctrl Pts',(0.0298727943515444,0.117734282457535,
-0.73765));
#40291=CARTESIAN_POINT('Ctrl Pts',(0.0335752445366655,0.117130286443933,
-0.73765));
#40292=CARTESIAN_POINT('Ctrl Pts',(0.0372395824352719,0.116356599132226,
-0.73765));
#40293=CARTESIAN_POINT('Ctrl Pts',(0.0440678843012388,0.114914873325166,
-0.73765));
#40294=CARTESIAN_POINT('Ctrl Pts',(0.0507761145954882,0.112884283325685,
-0.73765));
#40295=CARTESIAN_POINT('Ctrl Pts',(0.0572985626748901,0.110316011463869,
-0.73765));
#40296=CARTESIAN_POINT('Ctrl Pts',(0.0611801597768471,0.108787598129718,
-0.73765));
#40297=CARTESIAN_POINT('Ctrl Pts',(0.0649985389765126,0.107066533179972,
-0.73765));
#40298=CARTESIAN_POINT('Ctrl Pts',(0.0687175636740839,0.105173564435539,
-0.73765));
#40299=CARTESIAN_POINT('Ctrl Pts',(0.0771723185211559,0.100870127924939,
-0.73765));
#40300=CARTESIAN_POINT('Ctrl Pts',(0.0851385654920254,0.095673845814644,
-0.73765));
#40301=CARTESIAN_POINT('Ctrl Pts',(0.092460845720161,0.0896941979495885,
-0.73765));
#40302=CARTESIAN_POINT('Ctrl Pts',(0.0953295505232922,0.087351506326615,
-0.73765));
#40303=CARTESIAN_POINT('Ctrl Pts',(0.0980993075401888,0.0848880166213253,
-0.73765));
#40304=CARTESIAN_POINT('Ctrl Pts',(0.100759943103025,0.082308310166907,
-0.73765));
#40305=CARTESIAN_POINT('Ctrl Pts',(0.102972427973208,0.0801631229117881,
-0.73765));
#40306=CARTESIAN_POINT('Ctrl Pts',(0.105109190100999,0.0779373067134747,
-0.73765));
#40307=CARTESIAN_POINT('Ctrl Pts',(0.107154943682283,0.0756446505534301,
-0.73765));
#40308=CARTESIAN_POINT('Ctrl Pts',(0.110688967967185,0.0716841038773035,
-0.73765));
#40309=CARTESIAN_POINT('Ctrl Pts',(0.113959348635532,0.0675170854532638,
-0.73765));
#40310=CARTESIAN_POINT('Ctrl Pts',(0.116939708255812,0.0631610811162178,
-0.73765));
#40311=CARTESIAN_POINT('Ctrl Pts',(0.12057791194668,0.0578435915929273,
-0.73765));
#40312=CARTESIAN_POINT('Ctrl Pts',(0.123784383512494,0.0522446483168349,
-0.73765));
#40313=CARTESIAN_POINT('Ctrl Pts',(0.126564768603565,0.0464177189336189,
-0.73765));
#40314=CARTESIAN_POINT('Ctrl Pts',(0.127881821320869,0.0436575353884167,
-0.73765));
#40315=CARTESIAN_POINT('Ctrl Pts',(0.129103140600637,0.0408460784277879,
-0.73765));
#40316=CARTESIAN_POINT('Ctrl Pts',(0.130228617479411,0.0379885175969106,
-0.73765));
#40317=CARTESIAN_POINT('Ctrl Pts',(0.131421146659668,0.0349607124598609,
-0.73765));
#40318=CARTESIAN_POINT('Ctrl Pts',(0.132502923828134,0.0318888297538296,
-0.73765));
#40319=CARTESIAN_POINT('Ctrl Pts',(0.133473660931759,0.0287845863114225,
-0.73765));
#40320=CARTESIAN_POINT('Ctrl Pts',(0.13596121999,0.0208298178521682,-0.73765));
#40321=CARTESIAN_POINT('Ctrl Pts',(0.137724934662181,0.0126541835654583,
-0.73765));
#40322=CARTESIAN_POINT('Ctrl Pts',(0.138774959248534,0.00436662491368386,
-0.73765));
#40323=CARTESIAN_POINT('Ctrl Pts',(0.139475142462338,-0.00115973087531884,
-0.73765));
#40324=CARTESIAN_POINT('Ctrl Pts',(0.139857543532154,-0.00673626433291896,
-0.73765));
#40325=CARTESIAN_POINT('Ctrl Pts',(0.139919399280779,-0.0123331745591834,
-0.73765));
#40326=CARTESIAN_POINT('Ctrl Pts',(0.139954302158222,-0.0154913009423901,
-0.73765));
#40327=CARTESIAN_POINT('Ctrl Pts',(0.139886760375099,-0.0186552059838679,
-0.73765));
#40328=CARTESIAN_POINT('Ctrl Pts',(0.139717313713924,-0.0218061889195747,
-0.73765));
#40329=CARTESIAN_POINT('Ctrl Pts',(0.139162565153442,-0.0321221387031601,
-0.73765));
#40330=CARTESIAN_POINT('Ctrl Pts',(0.137520401557198,-0.0423353653549661,
-0.73765));
#40331=CARTESIAN_POINT('Ctrl Pts',(0.134789335766029,-0.0522596970838267,
-0.73765));
#40332=CARTESIAN_POINT('Ctrl Pts',(0.1331818334651,-0.0581011477515141,
-0.73765));
#40333=CARTESIAN_POINT('Ctrl Pts',(0.131196160006388,-0.0638428465505078,
-0.73765));
#40334=CARTESIAN_POINT('Ctrl Pts',(0.128823493644032,-0.0694465980833189,
-0.73765));
#40335=CARTESIAN_POINT('Ctrl Pts',(-0.00088475083857086,0.117943724677159,
-0.73765));
#40336=CARTESIAN_POINT('Ctrl Pts',(-0.0359625809725899,0.117451794425203,
-0.735271625314648));
#40337=CARTESIAN_POINT('Ctrl Pts',(-0.0971707523342012,0.0878186355611941,
-0.731126054823441));
#40338=CARTESIAN_POINT('Ctrl Pts',(-0.117482453641731,0.0261030598409213,
-0.726980484332236));
#40339=CARTESIAN_POINT('Ctrl Pts',(-0.117673801045155,-9.24777646016256E-5,
-0.725213288526384));
#40340=CARTESIAN_POINT('Origin',(-3.28582941601228E-18,0.,-0.73765));
#40341=CARTESIAN_POINT('',(-0.111717694016328,0.0372841450039317,-0.73765));
#40342=CARTESIAN_POINT('Ctrl Pts',(0.0262121662178384,-0.144200775921424,
-0.73765));
#40343=CARTESIAN_POINT('Ctrl Pts',(0.0216914116314411,-0.144617508648269,
-0.73765));
#40344=CARTESIAN_POINT('Ctrl Pts',(0.017160159126439,-0.144810578739906,
-0.73765));
#40345=CARTESIAN_POINT('Ctrl Pts',(0.012630831538952,-0.144770228896137,
-0.73765));
#40346=CARTESIAN_POINT('Ctrl Pts',(0.00502278391791575,-0.144702452051349,
-0.73765));
#40347=CARTESIAN_POINT('Ctrl Pts',(-0.00258026785134787,-0.143976762872906,
-0.73765));
#40348=CARTESIAN_POINT('Ctrl Pts',(-0.0101072259685224,-0.142628707009231,
-0.73765));
#40349=CARTESIAN_POINT('Ctrl Pts',(-0.0135423586684204,-0.142013484935917,
-0.73765));
#40350=CARTESIAN_POINT('Ctrl Pts',(-0.0169589000212732,-0.141268716329859,
-0.73765));
#40351=CARTESIAN_POINT('Ctrl Pts',(-0.0203418084420799,-0.140400116655759,
-0.73765));
#40352=CARTESIAN_POINT('Ctrl Pts',(-0.0268350469323433,-0.138732904856054,
-0.73765));
#40353=CARTESIAN_POINT('Ctrl Pts',(-0.0332137854254147,-0.136608416932435,
-0.73765));
#40354=CARTESIAN_POINT('Ctrl Pts',(-0.0394282027288326,-0.134050378168974,
-0.73765));
#40355=CARTESIAN_POINT('Ctrl Pts',(-0.0426874420061282,-0.13270877846563,
-0.73765));
#40356=CARTESIAN_POINT('Ctrl Pts',(-0.0459032314063151,-0.131246864018571,
-0.73765));
#40357=CARTESIAN_POINT('Ctrl Pts',(-0.0490617852831597,-0.129670241929581,
-0.73765));
#40358=CARTESIAN_POINT('Ctrl Pts',(-0.0579717447200327,-0.125222751271541,
-0.73765));
#40359=CARTESIAN_POINT('Ctrl Pts',(-0.0663802608480417,-0.119890965737638,
-0.73765));
#40360=CARTESIAN_POINT('Ctrl Pts',(-0.074123276457021,-0.113753043432987,
-0.73765));
#40361=CARTESIAN_POINT('Ctrl Pts',(-0.0793760400744385,-0.109589154762658,
-0.73765));
#40362=CARTESIAN_POINT('Ctrl Pts',(-0.0843220259407665,-0.105053336421179,
-0.73765));
#40363=CARTESIAN_POINT('Ctrl Pts',(-0.0888980477470807,-0.100162202168974,
-0.73765));
#40364=CARTESIAN_POINT('Ctrl Pts',(-0.0907777300028143,-0.0981530818777209,
-0.73765));
#40365=CARTESIAN_POINT('Ctrl Pts',(-0.092593341574421,-0.0960852887450699,
-0.73765));
#40366=CARTESIAN_POINT('Ctrl Pts',(-0.0943350874707246,-0.0939670993988704,
-0.73765));
#40367=CARTESIAN_POINT('Ctrl Pts',(-0.0976089573306515,-0.0899856482165493,
-0.73765));
#40368=CARTESIAN_POINT('Ctrl Pts',(-0.100628388290881,-0.0858197177372537,
-0.73765));
#40369=CARTESIAN_POINT('Ctrl Pts',(-0.10336682064894,-0.081478830271231,
-0.73765));
#40370=CARTESIAN_POINT('Ctrl Pts',(-0.106575782904835,-0.0763920717852811,
-0.73765));
#40371=CARTESIAN_POINT('Ctrl Pts',(-0.109399057782675,-0.0710649351750326,
-0.73765));
#40372=CARTESIAN_POINT('Ctrl Pts',(-0.111830948744127,-0.0655430594973256,
-0.73765));
#40373=CARTESIAN_POINT('Ctrl Pts',(-0.113091811307504,-0.0626801324862042,
-0.73765));
#40374=CARTESIAN_POINT('Ctrl Pts',(-0.114247330990164,-0.0597648360251877,
-0.73765));
#40375=CARTESIAN_POINT('Ctrl Pts',(-0.115295848804168,-0.0568035605001958,
-0.73765));
#40376=CARTESIAN_POINT('Ctrl Pts',(-0.116314386310609,-0.0539269568327871,
-0.73765));
#40377=CARTESIAN_POINT('Ctrl Pts',(-0.117229972470728,-0.0510120371908431,
-0.73765));
#40378=CARTESIAN_POINT('Ctrl Pts',(-0.118040228185711,-0.0480723152749109,
-0.73765));
#40379=CARTESIAN_POINT('Ctrl Pts',(-0.119975551423544,-0.0410506898405367,
-0.73765));
#40380=CARTESIAN_POINT('Ctrl Pts',(-0.121315904182743,-0.0338746385959458,
-0.73765));
#40381=CARTESIAN_POINT('Ctrl Pts',(-0.122051121145503,-0.0266271899647891,
-0.73765));
#40382=CARTESIAN_POINT('Ctrl Pts',(-0.122625570639283,-0.0209645170284367,
-0.73765));
#40383=CARTESIAN_POINT('Ctrl Pts',(-0.122830202791461,-0.0152581010368553,
-0.73765));
#40384=CARTESIAN_POINT('Ctrl Pts',(-0.122652104845954,-0.00954986495031056,
-0.73765));
#40385=CARTESIAN_POINT('Ctrl Pts',(-0.122569605793161,-0.00690567908438269,
-0.73765));
#40386=CARTESIAN_POINT('Ctrl Pts',(-0.122404760993965,-0.00426311687457716,
-0.73765));
#40387=CARTESIAN_POINT('Ctrl Pts',(-0.122157517869817,-0.00163526686520094,
-0.73765));
#40388=CARTESIAN_POINT('Ctrl Pts',(-0.121338098277213,0.00707402198368037,
-0.73765));
#40389=CARTESIAN_POINT('Ctrl Pts',(-0.119616360728985,0.0156516535710813,
-0.73765));
#40390=CARTESIAN_POINT('Ctrl Pts',(-0.116954245640549,0.0239432946408254,
-0.73765));
#40391=CARTESIAN_POINT('Ctrl Pts',(-0.115495686406583,0.028486242351667,
-0.73765));
#40392=CARTESIAN_POINT('Ctrl Pts',(-0.113754063897855,0.0329430069155385,
-0.73765));
#40393=CARTESIAN_POINT('Ctrl Pts',(-0.111717694016328,0.0372841450039292,
-0.73765));
#40394=CARTESIAN_POINT('Origin',(0.,0.,-0.73765));
#40395=CARTESIAN_POINT('Origin',(0.,0.,-0.860086711473615));
#40396=CARTESIAN_POINT('Ctrl Pts',(-0.111717694016328,0.037284145003932,
-0.73765));
#40397=CARTESIAN_POINT('Ctrl Pts',(-0.115720921699071,0.0252889292013099,
-0.736795570491205));
#40398=CARTESIAN_POINT('Ctrl Pts',(-0.117632122859214,0.0126318657558966,
-0.735941140982411));
#40399=CARTESIAN_POINT('Ctrl Pts',(-0.11756447877375,-3.10001368070065E-5,
-0.735086711473616));
#40400=CARTESIAN_POINT('Ctrl Pts',(-0.138823048348881,0.0463301602320166,
-0.754147783942094));
#40401=CARTESIAN_POINT('Ctrl Pts',(-0.154110965519853,0.000521657650733254,
-0.751521905275632));
#40402=CARTESIAN_POINT('Ctrl Pts',(-0.135580905218918,-0.106630820062224,
-0.746270147942711));
#40403=CARTESIAN_POINT('Ctrl Pts',(0.0150378134171585,-0.171988340881595,
-0.738392511943325));
#40404=CARTESIAN_POINT('Ctrl Pts',(0.151886514761348,-0.081737977277168,
-0.730514875943943));
#40405=CARTESIAN_POINT('Ctrl Pts',(0.151754795995761,0.0820861101213215,
-0.722637239944558));
#40406=CARTESIAN_POINT('Ctrl Pts',(0.0146120564079159,0.171928721992484,
-0.714759603945174));
#40407=CARTESIAN_POINT('Ctrl Pts',(-0.13569138198474,0.106550741701972,
-0.70688196794579));
#40408=CARTESIAN_POINT('Ctrl Pts',(-0.16354633841588,-0.05496199688411,
-0.699004331946406));
#40409=CARTESIAN_POINT('Ctrl Pts',(-0.0437919749452907,-0.16688590131284,
-0.691126695947022));
#40410=CARTESIAN_POINT('Ctrl Pts',(0.115481099091748,-0.128186123155717,
-0.683249059947638));
#40411=CARTESIAN_POINT('Ctrl Pts',(0.170533594917282,0.0261985716909196,
-0.675371423948254));
#40412=CARTESIAN_POINT('Ctrl Pts',(0.0716770510023252,0.156941001890843,
-0.667493787948871));
#40413=CARTESIAN_POINT('Ctrl Pts',(-0.0918680462662227,0.14604176284845,
-0.659616151949486));
#40414=CARTESIAN_POINT('Ctrl Pts',(-0.17250178293021,0.00333924143125606,
-0.651738515950102));
#40415=CARTESIAN_POINT('Ctrl Pts',(-0.0974510977380058,-0.14237728741126,
-0.643860879950718));
#40416=CARTESIAN_POINT('Ctrl Pts',(0.0655499140182738,-0.159596988908127,
-0.635983243951334));
#40417=CARTESIAN_POINT('Ctrl Pts',(0.16939163808025,-0.0327791950909268,
-0.628105607951951));
#40418=CARTESIAN_POINT('Ctrl Pts',(0.12035600598554,0.123622135200244,-0.620227971952565));
#40419=CARTESIAN_POINT('Ctrl Pts',(-0.0373018898023092,0.168453457330507,
-0.612350335953183));
#40420=CARTESIAN_POINT('Ctrl Pts',(-0.161294532557813,0.0612541747614786,
-0.604472699953798));
#40421=CARTESIAN_POINT('Ctrl Pts',(-0.139717542474164,-0.10122750617809,
-0.596595063954415));
#40422=CARTESIAN_POINT('Ctrl Pts',(0.00795566602636565,-0.172350534702269,
-0.58871742795503));
#40423=CARTESIAN_POINT('Ctrl Pts',(0.148448822061392,-0.0879258035956179,
-0.580839791955647));
#40424=CARTESIAN_POINT('Ctrl Pts',(0.154965706478682,0.0758526824482954,
-0.572962155956262));
#40425=CARTESIAN_POINT('Ctrl Pts',(0.0216247787522968,0.171173504196391,
-0.565084519956878));
#40426=CARTESIAN_POINT('Ctrl Pts',(-0.131232688082165,0.112008844349949,
-0.557206883957495));
#40427=CARTESIAN_POINT('Ctrl Pts',(-0.165651584869631,-0.0482447100545612,
-0.549329247958111));
#40428=CARTESIAN_POINT('Ctrl Pts',(-0.0505685770021586,-0.164957020573233,
-0.541451611958726));
#40429=CARTESIAN_POINT('Ctrl Pts',(0.110152983545764,-0.132794276374095,
-0.533573975959343));
#40430=CARTESIAN_POINT('Ctrl Pts',(0.171460579160472,0.0192163839752785,
-0.525696339959958));
#40431=CARTESIAN_POINT('Ctrl Pts',(0.0780236054224529,0.153884101245222,
-0.517818703960575));
#40432=CARTESIAN_POINT('Ctrl Pts',(-0.0858303077688239,0.149670163653888,
-0.50994106796119));
#40433=CARTESIAN_POINT('Ctrl Pts',(-0.172221669049576,0.010377684194152,
-0.502063431961807));
#40434=CARTESIAN_POINT('Ctrl Pts',(-0.103181571148412,-0.138280739782684,
-0.494185795962423));
#40435=CARTESIAN_POINT('Ctrl Pts',(0.0589807352003881,-0.162139669713528,
-0.486308159963038));
#40436=CARTESIAN_POINT('Ctrl Pts',(0.167912447591442,-0.0396662269869119,
-0.478430523963655));
#40437=CARTESIAN_POINT('Ctrl Pts',(0.125301808267477,0.118606308704212,
-0.470552887964271));
#40438=CARTESIAN_POINT('Ctrl Pts',(-0.0303947336884643,0.169835684658897,
-0.462675251964886));
#40439=CARTESIAN_POINT('Ctrl Pts',(-0.158659780904255,0.0677869717788998,
-0.454797615965503));
#40440=CARTESIAN_POINT('Ctrl Pts',(-0.14373308345953,-0.0954400353036286,
-0.446919979966119));
#40441=CARTESIAN_POINT('Ctrl Pts',(0.000913892613523542,-0.172531633099076,
-0.439042343966734));
#40442=CARTESIAN_POINT('Ctrl Pts',(0.144736073158576,-0.0939120266322549,
-0.431164707967351));
#40443=CARTESIAN_POINT('Ctrl Pts',(0.157932768701871,0.0694639488490502,
-0.423287071967967));
#40444=CARTESIAN_POINT('Ctrl Pts',(0.0285938540193059,0.170148144661836,
-0.415409435968583));
#40445=CARTESIAN_POINT('Ctrl Pts',(-0.126551246832543,0.117272253942145,
-0.407531799969199));
#40446=CARTESIAN_POINT('Ctrl Pts',(-0.167482816569958,-0.0414428012245345,
-0.399654163969815));
#40447=CARTESIAN_POINT('Ctrl Pts',(-0.0572597800887704,-0.162755390705586,
-0.391776527970431));
#40448=CARTESIAN_POINT('Ctrl Pts',(0.104640674343329,-0.137179914318808,
-0.383898891971047));
#40449=CARTESIAN_POINT('Ctrl Pts',(0.172102067809386,0.0122015521666594,
-0.376021255971662));
#40450=CARTESIAN_POINT('Ctrl Pts',(0.0842399431862384,0.150571018431575,
-0.368143619972279));
#40451=CARTESIAN_POINT('Ctrl Pts',(-0.0796494163555106,0.153048914056156,
-0.360265983972895));
#40452=CARTESIAN_POINT('Ctrl Pts',(-0.17165452883643,0.0173989180550344,
-0.352388347973511));
#40453=CARTESIAN_POINT('Ctrl Pts',(-0.108740030796753,-0.133953743217066,
-0.344510711974127));
#40454=CARTESIAN_POINT('Ctrl Pts',(0.0523132308002934,-0.164412060089207,
-0.336633075974743));
#40455=CARTESIAN_POINT('Ctrl Pts',(0.166153375472371,-0.0464871534800791,
-0.328755439975359));
#40456=CARTESIAN_POINT('Ctrl Pts',(0.130038745345635,0.113392787815077,
-0.320877803975975));
#40457=CARTESIAN_POINT('Ctrl Pts',(-0.023436911711692,0.170934814443863,
-0.313000167976591));
#40458=CARTESIAN_POINT('Ctrl Pts',(-0.155760565039272,0.0742067786539452,
-0.305122531977207));
#40459=CARTESIAN_POINT('Ctrl Pts',(-0.147509039640546,-0.0894934793371125,
-0.297244895977823));
#40460=CARTESIAN_POINT('Ctrl Pts',(-0.00612940440244159,-0.172425143239602,
-0.289367259978439));
#40461=CARTESIAN_POINT('Ctrl Pts',(0.140782068237328,-0.0997417108456163,
-0.281489623979055));
#40462=CARTESIAN_POINT('Ctrl Pts',(0.160636577524524,0.0629594280525857,
-0.273611987979671));
#40463=CARTESIAN_POINT('Ctrl Pts',(0.0355152670997055,0.168839170284302,
-0.265734351980287));
#40464=CARTESIAN_POINT('Ctrl Pts',(-0.121658861180512,0.122340186022964,
-0.257856715980903));
#40465=CARTESIAN_POINT('Ctrl Pts',(-0.169034876246628,-0.0345718126723981,
-0.249979079981519));
#40466=CARTESIAN_POINT('Ctrl Pts',(-0.0638555385981163,-0.160282468815134,
-0.242101443982135));
#40467=CARTESIAN_POINT('Ctrl Pts',(0.0989539427921171,-0.141336891247995,
-0.234223807982751));
#40468=CARTESIAN_POINT('Ctrl Pts',(0.172456684746421,0.00516638197338353,
-0.226346171983367));
#40469=CARTESIAN_POINT('Ctrl Pts',(0.0903158639700122,0.14700695335058,
-0.218468535983983));
#40470=CARTESIAN_POINT('Ctrl Pts',(-0.0733357597872231,0.15617255191074,
-0.210590899984599));
#40471=CARTESIAN_POINT('Ctrl Pts',(-0.170801262847335,0.0243911501310009,
-0.202713263985215));
#40472=CARTESIAN_POINT('Ctrl Pts',(-0.114117235117242,-0.129403463123037,
-0.194835627985831));
#40473=CARTESIAN_POINT('Ctrl Pts',(0.04555852729765,-0.166410397210689,
-0.186957991986448));
#40474=CARTESIAN_POINT('Ctrl Pts',(0.164117346908928,-0.0532305915583867,
-0.179080355987063));
#40475=CARTESIAN_POINT('Ctrl Pts',(0.134558925626773,0.10799025519103,-0.17120271998768));
#40476=CARTESIAN_POINT('Ctrl Pts',(-0.0164400250396412,0.171749019605496,
-0.163325083988295));
#40477=CARTESIAN_POINT('Ctrl Pts',(-0.152601713625263,0.0805028898118418,
-0.155447447988912));
#40478=CARTESIAN_POINT('Ctrl Pts',(-0.151039123194672,-0.0833977442910985,
-0.147569811989528));
#40479=CARTESIAN_POINT('Ctrl Pts',(-0.0131624736632622,-0.172031252885583,
-0.139692175990144));
#40480=CARTESIAN_POINT('Ctrl Pts',(0.13659337737755,-0.10540512014574,-0.13181453999076));
#40481=CARTESIAN_POINT('Ctrl Pts',(0.163072665249414,0.0563499269687501,
-0.123936903991376));
#40482=CARTESIAN_POINT('Ctrl Pts',(0.042377406518749,0.167248829784194,
-0.116059267991992));
#40483=CARTESIAN_POINT('Ctrl Pts',(-0.116563544816227,0.127204066132066,
-0.108181631992608));
#40484=CARTESIAN_POINT('Ctrl Pts',(-0.170305445231403,-0.0276429564161484,
-0.100303995993224));
#40485=CARTESIAN_POINT('Ctrl Pts',(-0.0703443482700645,-0.157542834875204,
-0.0924263599938398));
#40486=CARTESIAN_POINT('Ctrl Pts',(0.0931012989163088,-0.145257407925471,
-0.0845487239944556));
#40487=CARTESIAN_POINT('Ctrl Pts',(0.172525680076593,-0.00187905314371138,
-0.0766710879950718));
#40488=CARTESIAN_POINT('Ctrl Pts',(0.096237741546027,0.143200988169951,
-0.0687934519956877));
#40489=CARTESIAN_POINT('Ctrl Pts',(-0.0668932145228675,0.159029901442989,
-0.0609158159963038));
#40490=CARTESIAN_POINT('Ctrl Pts',(-0.169675926294121,0.0313540695073055,
-0.0530381799969198));
#40491=CARTESIAN_POINT('Ctrl Pts',(-0.119280200416385,-0.124659060525867,
-0.0451605439975358));
#40492=CARTESIAN_POINT('Ctrl Pts',(0.03868209760446,-0.168090171100606,
-0.0372829079981519));
#40493=CARTESIAN_POINT('Ctrl Pts',(0.161895992042455,-0.0599650981168399,
-0.0294052719987679));
#40494=CARTESIAN_POINT('Ctrl Pts',(0.1386766030792,0.102572478792013,-0.0215276359993839));
#40495=CARTESIAN_POINT('Ctrl Pts',(0.040233477224662,0.148767365811789,
-0.0162758786664613));
#40496=CARTESIAN_POINT('Ctrl Pts',(-0.00798678478682508,0.146131905375825,
-0.0136499999999999));
#40497=CARTESIAN_POINT('Ctrl Pts',(-0.12978793023803,0.0433148218226551,
-0.748648522628063));
#40498=CARTESIAN_POINT('Ctrl Pts',(-0.144080853141469,0.000487706238889336,
-0.746022643961601));
#40499=CARTESIAN_POINT('Ctrl Pts',(-0.126756797790082,-0.0996908913905975,
-0.740770886628678));
#40500=CARTESIAN_POINT('Ctrl Pts',(0.0140590968281712,-0.16079470270669,
-0.732893250629295));
#40501=CARTESIAN_POINT('Ctrl Pts',(0.14200117787647,-0.0764181670034058,
-0.72501561462991));
#40502=CARTESIAN_POINT('Ctrl Pts',(0.141878031855961,0.0767436420727705,
-0.717137978630528));
#40503=CARTESIAN_POINT('Ctrl Pts',(0.0136610496618582,0.160738964035679,
-0.709260342631142));
#40504=CARTESIAN_POINT('Ctrl Pts',(-0.12686008431884,0.0996160248265959,
-0.701382706631759));
#40505=CARTESIAN_POINT('Ctrl Pts',(-0.152902137025984,-0.051384866577851,
-0.693505070632375));
#40506=CARTESIAN_POINT('Ctrl Pts',(-0.0409418310344329,-0.156024348801704,
-0.68562743463299));
#40507=CARTESIAN_POINT('Ctrl Pts',(0.107965161484308,-0.119843295529764,
-0.677749798633607));
#40508=CARTESIAN_POINT('Ctrl Pts',(0.159434636997316,0.0244934716201587,
-0.669872162634223));
#40509=CARTESIAN_POINT('Ctrl Pts',(0.0670120430706731,0.146726700264534,
-0.661994526634839));
#40510=CARTESIAN_POINT('Ctrl Pts',(-0.0858889335864435,0.136536824063813,
-0.654116890635455));
#40511=CARTESIAN_POINT('Ctrl Pts',(-0.161274728045275,0.00312191123219325,
-0.64623925463607));
#40512=CARTESIAN_POINT('Ctrl Pts',(-0.0911086193918861,-0.133110846259281,
-0.638361618636687));
#40513=CARTESIAN_POINT('Ctrl Pts',(0.0612836828530949,-0.149209825810416,
-0.630483982637303));
#40514=CARTESIAN_POINT('Ctrl Pts',(0.158367002940418,-0.0306458036782776,
-0.62260634663792));
#40515=CARTESIAN_POINT('Ctrl Pts',(0.112522791383474,0.115576348812938,
-0.614728710638535));
#40516=CARTESIAN_POINT('Ctrl Pts',(-0.0348741446682685,0.157489882468374,
-0.606851074639151));
#40517=CARTESIAN_POINT('Ctrl Pts',(-0.150796887032612,0.0572675262161885,
-0.598973438639767));
#40518=CARTESIAN_POINT('Ctrl Pts',(-0.130624207372924,-0.0946392451849487,
-0.591095802640384));
#40519=CARTESIAN_POINT('Ctrl Pts',(0.0074378818179544,-0.161133323612149,
-0.583218166640998));
#40520=CARTESIAN_POINT('Ctrl Pts',(0.138787222948753,-0.0822032666687414,
-0.575340530641615));
#40521=CARTESIAN_POINT('Ctrl Pts',(0.144879964393206,0.0709159089578964,
-0.567462894642231));
#40522=CARTESIAN_POINT('Ctrl Pts',(0.0202173580647961,0.160032898610667,
-0.559585258642847));
#40523=CARTESIAN_POINT('Ctrl Pts',(-0.122691578727996,0.104718893940429,
-0.551707622643464));
#40524=CARTESIAN_POINT('Ctrl Pts',(-0.154870366243849,-0.0451047656523092,
-0.543829986644079));
#40525=CARTESIAN_POINT('Ctrl Pts',(-0.0472773867326288,-0.154221006764145,
-0.535952350644695));
#40526=CARTESIAN_POINT('Ctrl Pts',(0.10298381943047,-0.124151533070622,
-0.528074714645311));
#40527=CARTESIAN_POINT('Ctrl Pts',(0.160301289672918,0.0179657105392391,
-0.520197078645928));
#40528=CARTESIAN_POINT('Ctrl Pts',(0.0729455402249881,0.143868754034011,
-0.512319442646543));
#40529=CARTESIAN_POINT('Ctrl Pts',(-0.0802441534709221,0.13992907510723,
-0.50444180664716));
#40530=CARTESIAN_POINT('Ctrl Pts',(-0.16101284501338,0.00970226607355439,
-0.496564170647775));
#40531=CARTESIAN_POINT('Ctrl Pts',(-0.0964661323702182,-0.129280917121734,
-0.488686534648391));
#40532=CARTESIAN_POINT('Ctrl Pts',(0.0551420505213066,-0.151587019532309,
-0.480808898649007));
#40533=CARTESIAN_POINT('Ctrl Pts',(0.156984083646731,-0.0370846020326892,
-0.472931262649624));
#40534=CARTESIAN_POINT('Ctrl Pts',(0.117146702536368,0.110886970881133,
-0.465053626650239));
#40535=CARTESIAN_POINT('Ctrl Pts',(-0.0284165318546242,0.158782149323222,
-0.457175990650856));
#40536=CARTESIAN_POINT('Ctrl Pts',(-0.14833361477434,0.0633751446098248,
-0.449298354651471));
#40537=CARTESIAN_POINT('Ctrl Pts',(-0.134378402079605,-0.0892284443486102,
-0.441420718652087));
#40538=CARTESIAN_POINT('Ctrl Pts',(0.000854413097680245,-0.161302635454603,
-0.433543082652704));
#40539=CARTESIAN_POINT('Ctrl Pts',(0.135316113494514,-0.0877998841404727,
-0.42566544665332));
#40540=CARTESIAN_POINT('Ctrl Pts',(0.147653919218541,0.0649429778016496,
-0.417787810653936));
#40541=CARTESIAN_POINT('Ctrl Pts',(0.0267328601038017,0.15907427327199,
-0.409910174654551));
#40542=CARTESIAN_POINT('Ctrl Pts',(-0.118314823012387,0.109639741343586,
-0.402032538655168));
#40543=CARTESIAN_POINT('Ctrl Pts',(-0.156582414603242,-0.0387455502394743,
-0.394154902655784));
#40544=CARTESIAN_POINT('Ctrl Pts',(-0.0535331015418237,-0.152162667121912,
-0.386277266656399));
#40545=CARTESIAN_POINT('Ctrl Pts',(0.0978302717254945,-0.128251737455899,
-0.378399630657016));
#40546=CARTESIAN_POINT('Ctrl Pts',(0.16090102786484,0.0114074299638081,
-0.370521994657631));
#40547=CARTESIAN_POINT('Ctrl Pts',(0.0787572957052066,0.140771298919715,
-0.362644358658248));
#40548=CARTESIAN_POINT('Ctrl Pts',(-0.0744655373614135,0.143087923920284,
-0.354766722658863));
#40549=CARTESIAN_POINT('Ctrl Pts',(-0.160482616385682,0.0162665320319777,
-0.34688908665948));
#40550=CARTESIAN_POINT('Ctrl Pts',(-0.101662826879164,-0.125235537517425,
-0.339011450660095));
#40551=CARTESIAN_POINT('Ctrl Pts',(0.0489084920003435,-0.153711514326653,
-0.331133814660712));
#40552=CARTESIAN_POINT('Ctrl Pts',(0.155339498455806,-0.0434615973687168,
-0.323256178661328));
#40553=CARTESIAN_POINT('Ctrl Pts',(0.121575342206467,0.106012765239481,
-0.315378542661944));
#40554=CARTESIAN_POINT('Ctrl Pts',(-0.0219115507000505,0.15980974367121,
-0.30750090666256));
#40555=CARTESIAN_POINT('Ctrl Pts',(-0.145623090614954,0.0693771266780044,
-0.299623270663176));
#40556=CARTESIAN_POINT('Ctrl Pts',(-0.137908605048293,-0.0836689122671714,
-0.291745634663792));
#40557=CARTESIAN_POINT('Ctrl Pts',(-0.00573048006398319,-0.161203076349563,
-0.283867998664408));
#40558=CARTESIAN_POINT('Ctrl Pts',(0.131619449857004,-0.0932501509152808,
-0.275990362665024));
#40559=CARTESIAN_POINT('Ctrl Pts',(0.150181754149593,0.0588617953077906,
-0.26811272666564));
#40560=CARTESIAN_POINT('Ctrl Pts',(0.0332038019878175,0.157850491794668,
-0.260235090666256));
#40561=CARTESIAN_POINT('Ctrl Pts',(-0.113740851937299,0.11437783363575,
-0.252357454666872));
#40562=CARTESIAN_POINT('Ctrl Pts',(-0.158033460488178,-0.0323217510686777,
-0.244479818667488));
#40563=CARTESIAN_POINT('Ctrl Pts',(-0.0596995836603153,-0.149850692146435,
-0.236602182668104));
#40564=CARTESIAN_POINT('Ctrl Pts',(0.0925136537241649,-0.132138162931375,
-0.22872454666872));
#40565=CARTESIAN_POINT('Ctrl Pts',(0.161232565018306,0.00483013470111595,
-0.220846910669336));
#40566=CARTESIAN_POINT('Ctrl Pts',(0.0844377730624996,0.13743919639353,
-0.212969274669952));
#40567=CARTESIAN_POINT('Ctrl Pts',(-0.0685627969449054,0.146008263855052,
-0.205091638670568));
#40568=CARTESIAN_POINT('Ctrl Pts',(-0.159684884107186,0.0228036837490541,
-0.197214002671184));
#40569=CARTESIAN_POINT('Ctrl Pts',(-0.106690062828264,-0.120981406503653,
-0.1893363666718));
#40570=CARTESIAN_POINT('Ctrl Pts',(0.042593409617363,-0.155579792267527,
-0.181458730672416));
#40571=CARTESIAN_POINT('Ctrl Pts',(0.153435982171603,-0.0497661475228981,
-0.173581094673032));
#40572=CARTESIAN_POINT('Ctrl Pts',(0.125801332414644,0.10096184944662,-0.165703458673648));
#40573=CARTESIAN_POINT('Ctrl Pts',(-0.0153700473252411,0.160570957345555,
-0.157825822674264));
#40574=CARTESIAN_POINT('Ctrl Pts',(-0.142669828949619,0.0752634636044082,
-0.14994818667488));
#40575=CARTESIAN_POINT('Ctrl Pts',(-0.141208937691226,-0.0779699102332057,
-0.142070550675496));
#40576=CARTESIAN_POINT('Ctrl Pts',(-0.0123058111306849,-0.160834821838537,
-0.134192914676112));
#40577=CARTESIAN_POINT('Ctrl Pts',(0.12770337451099,-0.0985449645639955,
-0.126315278676728));
#40578=CARTESIAN_POINT('Ctrl Pts',(0.152459292263417,0.0526824650324521,
-0.118437642677344));
#40579=CARTESIAN_POINT('Ctrl Pts',(0.039619327959875,0.156363656544054,
-0.110560006677961));
#40580=CARTESIAN_POINT('Ctrl Pts',(-0.108977157632254,0.118925154414212,
-0.102682370678576));
#40581=CARTESIAN_POINT('Ctrl Pts',(-0.159221336137934,-0.025843850438262,
-0.0948047346791926));
#40582=CARTESIAN_POINT('Ctrl Pts',(-0.0657660775678267,-0.147289363729415,
-0.0869270986798085));
#40583=CARTESIAN_POINT('Ctrl Pts',(0.0870419215867718,-0.135803517864042,
-0.0790494626804245));
#40584=CARTESIAN_POINT('Ctrl Pts',(0.16129706987687,-0.00175675740613725,
-0.0711718266810406));
#40585=CARTESIAN_POINT('Ctrl Pts',(0.089974232914486,0.133880937522061,
-0.0632941906816565));
#40586=CARTESIAN_POINT('Ctrl Pts',(-0.0625395563860025,0.14867964649769,
-0.0554165546822727));
#40587=CARTESIAN_POINT('Ctrl Pts',(-0.158632788624483,0.0293134305455207,
-0.0475389186828885));
#40588=CARTESIAN_POINT('Ctrl Pts',(-0.111517003224952,-0.116545787198168,
-0.0396612826835047));
#40589=CARTESIAN_POINT('Ctrl Pts',(0.0361645234351237,-0.157150240251728,
-0.0317836466841206));
#40590=CARTESIAN_POINT('Ctrl Pts',(0.151359201306518,-0.0560623474536147,
-0.0239060106847367));
#40591=CARTESIAN_POINT('Ctrl Pts',(0.129651016168851,0.0958966820001181,
-0.0160283746853527));
#40592=CARTESIAN_POINT('Ctrl Pts',(0.0376149335241836,0.139085034692163,
-0.0107766173524301));
#40593=CARTESIAN_POINT('Ctrl Pts',(-0.00746697525423609,0.136621099781669,
-0.00815073868596875));
#40594=CARTESIAN_POINT('Ctrl Pts',(-0.120752812127179,0.0402994834132936,
-0.743149261314032));
#40595=CARTESIAN_POINT('Ctrl Pts',(-0.134050740763084,0.000453754827045585,
-0.74052338264757));
#40596=CARTESIAN_POINT('Ctrl Pts',(-0.117932690361245,-0.0927509627189708,
-0.735271625314648));
#40597=CARTESIAN_POINT('Ctrl Pts',(0.0130803802391836,-0.149601064531786,
-0.727393989315262));
#40598=CARTESIAN_POINT('Ctrl Pts',(0.132115840991593,-0.0710983567296433,
-0.719516353315881));
#40599=CARTESIAN_POINT('Ctrl Pts',(0.132001267716162,0.0714011740242192,
-0.711638717316495));
#40600=CARTESIAN_POINT('Ctrl Pts',(0.0127100429158007,0.149549206078874,
-0.703761081317112));
#40601=CARTESIAN_POINT('Ctrl Pts',(-0.118028786652939,0.092681307951219,
-0.695883445317726));
#40602=CARTESIAN_POINT('Ctrl Pts',(-0.142257935636087,-0.0478077362715918,
-0.688005809318345));
#40603=CARTESIAN_POINT('Ctrl Pts',(-0.0380916871235754,-0.145162796290568,
-0.680128173318959));
#40604=CARTESIAN_POINT('Ctrl Pts',(0.100449223876869,-0.11150046790381,
-0.672250537319576));
#40605=CARTESIAN_POINT('Ctrl Pts',(0.148335679077349,0.0227883715493975,
-0.664372901320192));
#40606=CARTESIAN_POINT('Ctrl Pts',(0.0623470351390212,0.136512398638226,
-0.656495265320809));
#40607=CARTESIAN_POINT('Ctrl Pts',(-0.0799098209066646,0.127031885279177,
-0.648617629321423));
#40608=CARTESIAN_POINT('Ctrl Pts',(-0.15004767316034,0.00290458103313051,
-0.64073999332204));
#40609=CARTESIAN_POINT('Ctrl Pts',(-0.0847661410457665,-0.123844405107302,
-0.632862357322656));
#40610=CARTESIAN_POINT('Ctrl Pts',(0.0570174516879159,-0.138822662712705,
-0.624984721323272));
#40611=CARTESIAN_POINT('Ctrl Pts',(0.147342367800587,-0.0285124122656285,
-0.617107085323888));
#40612=CARTESIAN_POINT('Ctrl Pts',(0.104689576781408,0.107530562425632,
-0.609229449324504));
#40613=CARTESIAN_POINT('Ctrl Pts',(-0.0324463995342276,0.146526307606242,
-0.60135181332512));
#40614=CARTESIAN_POINT('Ctrl Pts',(-0.140299241507412,0.0532808776708985,
-0.593474177325736));
#40615=CARTESIAN_POINT('Ctrl Pts',(-0.121530872271684,-0.0880509841918077,
-0.585596541326352));
#40616=CARTESIAN_POINT('Ctrl Pts',(0.00692009760954291,-0.149916112522029,
-0.577718905326969));
#40617=CARTESIAN_POINT('Ctrl Pts',(0.129125623836115,-0.076480729741865,
-0.569841269327583));
#40618=CARTESIAN_POINT('Ctrl Pts',(0.134794222307729,0.0659791354674974,
-0.561963633328201));
#40619=CARTESIAN_POINT('Ctrl Pts',(0.0188099373772952,0.148892293024944,
-0.554085997328816));
#40620=CARTESIAN_POINT('Ctrl Pts',(-0.114150469373828,0.097428943530908,
-0.546208361329432));
#40621=CARTESIAN_POINT('Ctrl Pts',(-0.144089147618066,-0.0419648212500574,
-0.538330725330049));
#40622=CARTESIAN_POINT('Ctrl Pts',(-0.043986196463099,-0.143484992955057,
-0.530453089330663));
#40623=CARTESIAN_POINT('Ctrl Pts',(0.0958146553151759,-0.115508789767149,
-0.52257545333128));
#40624=CARTESIAN_POINT('Ctrl Pts',(0.149142000185364,0.0167150371031994,
-0.514697817331896));
#40625=CARTESIAN_POINT('Ctrl Pts',(0.0678674750275233,0.1338534068228,-0.506820181332512));
#40626=CARTESIAN_POINT('Ctrl Pts',(-0.0746579991730203,0.130187986560573,
-0.498942545333128));
#40627=CARTESIAN_POINT('Ctrl Pts',(-0.149804020977185,0.00902684795295702,
-0.491064909333744));
#40628=CARTESIAN_POINT('Ctrl Pts',(-0.089750693592024,-0.120281094460784,
-0.48318727333436));
#40629=CARTESIAN_POINT('Ctrl Pts',(0.0513033658422252,-0.14103436935109,
-0.475309637334976));
#40630=CARTESIAN_POINT('Ctrl Pts',(0.14605571970202,-0.0345029770784666,
-0.467432001335592));
#40631=CARTESIAN_POINT('Ctrl Pts',(0.108991596805259,0.103167633058055,
-0.459554365336209));
#40632=CARTESIAN_POINT('Ctrl Pts',(-0.0264383300207842,0.147728613987548,
-0.451676729336824));
#40633=CARTESIAN_POINT('Ctrl Pts',(-0.138007448644426,0.0589633174407497,
-0.443799093337441));
#40634=CARTESIAN_POINT('Ctrl Pts',(-0.125023720699679,-0.0830168533935917,
-0.435921457338056));
#40635=CARTESIAN_POINT('Ctrl Pts',(0.000794933581836814,-0.150073637810129,
-0.428043821338672));
#40636=CARTESIAN_POINT('Ctrl Pts',(0.125896153830453,-0.0816877416486904,
-0.420166185339288));
#40637=CARTESIAN_POINT('Ctrl Pts',(0.137375069735211,0.0604220067542489,
-0.412288549339905));
#40638=CARTESIAN_POINT('Ctrl Pts',(0.0248718661882977,0.148000401882144,
-0.40441091334052));
#40639=CARTESIAN_POINT('Ctrl Pts',(-0.110078399192231,0.102007228745028,
-0.396533277341137));
#40640=CARTESIAN_POINT('Ctrl Pts',(-0.145682012636526,-0.0360482992544141,
-0.388655641341752));
#40641=CARTESIAN_POINT('Ctrl Pts',(-0.0498064229948769,-0.141569943538238,
-0.380778005342368));
#40642=CARTESIAN_POINT('Ctrl Pts',(0.0910198691076597,-0.11932356059299,
-0.372900369342984));
#40643=CARTESIAN_POINT('Ctrl Pts',(0.149699987920293,0.0106133077609567,
-0.365022733343601));
#40644=CARTESIAN_POINT('Ctrl Pts',(0.0732746482241745,0.130971579407855,
-0.357145097344216));
#40645=CARTESIAN_POINT('Ctrl Pts',(-0.0692816583673163,0.133126933784411,
-0.349267461344833));
#40646=CARTESIAN_POINT('Ctrl Pts',(-0.149310703934934,0.0151341460089211,
-0.341389825345448));
#40647=CARTESIAN_POINT('Ctrl Pts',(-0.0945856229615745,-0.116517331817784,
-0.333512189346065));
#40648=CARTESIAN_POINT('Ctrl Pts',(0.0455037532003936,-0.1430109685641,
-0.32563455334668));
#40649=CARTESIAN_POINT('Ctrl Pts',(0.144525621439241,-0.0404360412573544,
-0.317756917347297));
#40650=CARTESIAN_POINT('Ctrl Pts',(0.113111939067299,0.0986327426638849,
-0.309879281347913));
#40651=CARTESIAN_POINT('Ctrl Pts',(-0.020386189688409,0.148684672898556,
-0.302001645348529));
#40652=CARTESIAN_POINT('Ctrl Pts',(-0.135485616190635,0.0645474747020636,
-0.294124009349145));
#40653=CARTESIAN_POINT('Ctrl Pts',(-0.12830817045604,-0.0778443451972303,
-0.286246373349761));
#40654=CARTESIAN_POINT('Ctrl Pts',(-0.00533155572552474,-0.149981009459524,
-0.278368737350377));
#40655=CARTESIAN_POINT('Ctrl Pts',(0.122456831476679,-0.0867585909849453,
-0.270491101350993));
#40656=CARTESIAN_POINT('Ctrl Pts',(0.139726930774663,0.0547641625629956,
-0.262613465351609));
#40657=CARTESIAN_POINT('Ctrl Pts',(0.0308923368759293,0.146861813305034,
-0.254735829352225));
#40658=CARTESIAN_POINT('Ctrl Pts',(-0.105822842694085,0.106415481248536,
-0.246858193352841));
#40659=CARTESIAN_POINT('Ctrl Pts',(-0.147032044729728,-0.0300716894649577,
-0.238980557353457));
#40660=CARTESIAN_POINT('Ctrl Pts',(-0.0555436287225143,-0.139418915477736,
-0.231102921354073));
#40661=CARTESIAN_POINT('Ctrl Pts',(0.0860733646562128,-0.122939434614756,
-0.223225285354689));
#40662=CARTESIAN_POINT('Ctrl Pts',(0.15000844529019,0.0044938874288485,
-0.215347649355305));
#40663=CARTESIAN_POINT('Ctrl Pts',(0.0785596821549869,0.127871439436481,
-0.207470013355921));
#40664=CARTESIAN_POINT('Ctrl Pts',(-0.0637898341025878,0.135843975799365,
-0.199592377356537));
#40665=CARTESIAN_POINT('Ctrl Pts',(-0.148568505367037,0.0212162173671073,
-0.191714741357153));
#40666=CARTESIAN_POINT('Ctrl Pts',(-0.0992628905392872,-0.112559349884269,
-0.183837105357769));
#40667=CARTESIAN_POINT('Ctrl Pts',(0.039628291937076,-0.144749187324364,
-0.175959469358385));
#40668=CARTESIAN_POINT('Ctrl Pts',(0.142754617434278,-0.0463017034874096,
-0.168081833359001));
#40669=CARTESIAN_POINT('Ctrl Pts',(0.117043739202515,0.0939334437022093,
-0.160204197359617));
#40670=CARTESIAN_POINT('Ctrl Pts',(-0.0143000696108409,0.149392895085614,
-0.152326561360233));
#40671=CARTESIAN_POINT('Ctrl Pts',(-0.132737944273974,0.0700240373969747,
-0.144448925360849));
#40672=CARTESIAN_POINT('Ctrl Pts',(-0.13137875218778,-0.0725420761753132,
-0.136571289361465));
#40673=CARTESIAN_POINT('Ctrl Pts',(-0.0114491485981074,-0.149638390791491,
-0.128693653362081));
#40674=CARTESIAN_POINT('Ctrl Pts',(0.11881337164443,-0.0916848089822516,
-0.120816017362697));
#40675=CARTESIAN_POINT('Ctrl Pts',(0.14184591927742,0.0490150030961542,
-0.112938381363313));
#40676=CARTESIAN_POINT('Ctrl Pts',(0.0368612494010009,0.145478483303915,
-0.105060745363929));
#40677=CARTESIAN_POINT('Ctrl Pts',(-0.101390770448281,0.110646242696357,
-0.0971831093645454));
#40678=CARTESIAN_POINT('Ctrl Pts',(-0.148137227044466,-0.0240447444603757,
-0.0893054733651613));
#40679=CARTESIAN_POINT('Ctrl Pts',(-0.061187806865589,-0.137035892583625,
-0.0814278373657773));
#40680=CARTESIAN_POINT('Ctrl Pts',(0.0809825442572348,-0.126349627802613,
-0.0735502013663932));
#40681=CARTESIAN_POINT('Ctrl Pts',(0.150068459677146,-0.00163446166856293,
-0.0656725653670095));
#40682=CARTESIAN_POINT('Ctrl Pts',(0.0837107242829451,0.124560886874171,
-0.0577949293676252));
#40683=CARTESIAN_POINT('Ctrl Pts',(-0.0581858982491374,0.138329391552391,
-0.0499172933682416));
#40684=CARTESIAN_POINT('Ctrl Pts',(-0.147589650954845,0.0272727915837357,
-0.0420396573688573));
#40685=CARTESIAN_POINT('Ctrl Pts',(-0.103753806033519,-0.108432513870469,
-0.0341620213694735));
#40686=CARTESIAN_POINT('Ctrl Pts',(0.0336469492657874,-0.14621030940285,
-0.0262843853700894));
#40687=CARTESIAN_POINT('Ctrl Pts',(0.140822410570581,-0.0521595967903893,
-0.0184067493707056));
#40688=CARTESIAN_POINT('Ctrl Pts',(0.120625429258503,0.0892208852082231,
-0.0105291133713215));
#40689=CARTESIAN_POINT('Ctrl Pts',(0.0349963898237052,0.129402703572537,
-0.00527735603839891));
#40690=CARTESIAN_POINT('Ctrl Pts',(-0.00694716572164709,0.127110294187512,
-0.00265147737193757));
#40691=CARTESIAN_POINT('Ctrl Pts',(-0.111717694016328,0.037284145003932,
-0.73765));
#40692=CARTESIAN_POINT('Ctrl Pts',(-0.124020628384699,0.000419803415201668,
-0.735024121333539));
#40693=CARTESIAN_POINT('Ctrl Pts',(-0.109108582932408,-0.0858110340473438,
-0.729772364000617));
#40694=CARTESIAN_POINT('Ctrl Pts',(0.0121016636501963,-0.138407426356883,
-0.721894728001232));
#40695=CARTESIAN_POINT('Ctrl Pts',(0.122230504106716,-0.0657785464558806,
-0.714017092001848));
#40696=CARTESIAN_POINT('Ctrl Pts',(0.122124503576362,0.0660587059756678,
-0.706139456002464));
#40697=CARTESIAN_POINT('Ctrl Pts',(0.0117590361697431,0.138359448122069,
-0.69826182000308));
#40698=CARTESIAN_POINT('Ctrl Pts',(-0.109197488987038,0.0857465910758423,
-0.690384184003696));
#40699=CARTESIAN_POINT('Ctrl Pts',(-0.131613734246191,-0.0442306059653326,
-0.682506548004313));
#40700=CARTESIAN_POINT('Ctrl Pts',(-0.0352415432127178,-0.134301243779432,
-0.674628912004927));
#40701=CARTESIAN_POINT('Ctrl Pts',(0.0929332862694289,-0.103157640277856,
-0.666751276005546));
#40702=CARTESIAN_POINT('Ctrl Pts',(0.137236721157382,0.0210832714786364,
-0.65887364000616));
#40703=CARTESIAN_POINT('Ctrl Pts',(0.0576820272073694,0.126298097011918,
-0.650996004006777));
#40704=CARTESIAN_POINT('Ctrl Pts',(-0.0739307082268856,0.11752694649454,
-0.643118368007392));
#40705=CARTESIAN_POINT('Ctrl Pts',(-0.138820618275404,0.0026872508340677,
-0.635240732008009));
#40706=CARTESIAN_POINT('Ctrl Pts',(-0.0784236626996469,-0.114577963955322,
-0.627363096008624));
#40707=CARTESIAN_POINT('Ctrl Pts',(0.0527512205227371,-0.128435499614995,
-0.619485460009241));
#40708=CARTESIAN_POINT('Ctrl Pts',(0.136317732660755,-0.0263790208529794,
-0.611607824009857));
#40709=CARTESIAN_POINT('Ctrl Pts',(0.0968563621793423,0.099484776038326,
-0.603730188010473));
#40710=CARTESIAN_POINT('Ctrl Pts',(-0.030018654400187,0.135562732744109,
-0.595852552011088));
#40711=CARTESIAN_POINT('Ctrl Pts',(-0.129801595982211,0.0492942291256084,
-0.587974916011705));
#40712=CARTESIAN_POINT('Ctrl Pts',(-0.112437537170444,-0.0814627231986667,
-0.580097280012321));
#40713=CARTESIAN_POINT('Ctrl Pts',(0.00640231340113165,-0.138698901431908,
-0.572219644012936));
#40714=CARTESIAN_POINT('Ctrl Pts',(0.119464024723476,-0.0707581928149885,
-0.564342008013553));
#40715=CARTESIAN_POINT('Ctrl Pts',(0.124708480222252,0.0610423619770983,
-0.556464372014168));
#40716=CARTESIAN_POINT('Ctrl Pts',(0.0174025166897942,0.137751687439221,
-0.548586736014785));
#40717=CARTESIAN_POINT('Ctrl Pts',(-0.10560936001966,0.0901389931213871,
-0.540709100015401));
#40718=CARTESIAN_POINT('Ctrl Pts',(-0.133307928992284,-0.0388248768478054,
-0.532831464016017));
#40719=CARTESIAN_POINT('Ctrl Pts',(-0.0406950061935692,-0.13274897914597,
-0.524953828016632));
#40720=CARTESIAN_POINT('Ctrl Pts',(0.0886454911998817,-0.106866046463675,
-0.51707619201725));
#40721=CARTESIAN_POINT('Ctrl Pts',(0.137982710697811,0.0154643636671598,
-0.509198556017864));
#40722=CARTESIAN_POINT('Ctrl Pts',(0.0627894098300584,0.12383805961159,
-0.501320920018481));
#40723=CARTESIAN_POINT('Ctrl Pts',(-0.0690718448751183,0.120446898013915,
-0.493443284019097));
#40724=CARTESIAN_POINT('Ctrl Pts',(-0.13859519694099,0.00835142983235973,
-0.485565648019713));
#40725=CARTESIAN_POINT('Ctrl Pts',(-0.0830352548138296,-0.111281271799835,
-0.477688012020329));
#40726=CARTESIAN_POINT('Ctrl Pts',(0.0474646811631436,-0.130481719169871,
-0.469810376020945));
#40727=CARTESIAN_POINT('Ctrl Pts',(0.135127355757309,-0.0319213521242443,
-0.461932740021561));
#40728=CARTESIAN_POINT('Ctrl Pts',(0.10083649107415,0.0954482952349766,
-0.454055104022177));
#40729=CARTESIAN_POINT('Ctrl Pts',(-0.024460128186944,0.136675078651873,
-0.446177468022793));
#40730=CARTESIAN_POINT('Ctrl Pts',(-0.127681282514511,0.0545514902716746,
-0.438299832023409));
#40731=CARTESIAN_POINT('Ctrl Pts',(-0.115669039319754,-0.0768052624385732,
-0.430422196024025));
#40732=CARTESIAN_POINT('Ctrl Pts',(0.000735454065993374,-0.138844640165656,
-0.42254456002464));
#40733=CARTESIAN_POINT('Ctrl Pts',(0.116476194166392,-0.0755755991569081,
-0.414666924025258));
#40734=CARTESIAN_POINT('Ctrl Pts',(0.127096220251881,0.0559010357068483,
-0.406789288025873));
#40735=CARTESIAN_POINT('Ctrl Pts',(0.0230108722727937,0.136926530492298,
-0.39891165202649));
#40736=CARTESIAN_POINT('Ctrl Pts',(-0.101841975372074,0.0943747161464696,
-0.391034016027105));
#40737=CARTESIAN_POINT('Ctrl Pts',(-0.13478161066981,-0.0333510482693538,
-0.383156380027722));
#40738=CARTESIAN_POINT('Ctrl Pts',(-0.0460797444479301,-0.130977219954565,
-0.375278744028337));
#40739=CARTESIAN_POINT('Ctrl Pts',(0.0842094664898252,-0.110395383730082,
-0.367401108028953));
#40740=CARTESIAN_POINT('Ctrl Pts',(0.138498947975746,0.0098191855581053,
-0.359523472029569));
#40741=CARTESIAN_POINT('Ctrl Pts',(0.0677920007431425,0.121171859895995,
-0.351645836030185));
#40742=CARTESIAN_POINT('Ctrl Pts',(-0.0640977793732191,0.123165943648539,
-0.343768200030801));
#40743=CARTESIAN_POINT('Ctrl Pts',(-0.138138791484186,0.0140017599858645,
-0.335890564031418));
#40744=CARTESIAN_POINT('Ctrl Pts',(-0.0875084190439853,-0.107799126118143,
-0.328012928032034));
#40745=CARTESIAN_POINT('Ctrl Pts',(0.0420990144004436,-0.132310422801546,
-0.320135292032649));
#40746=CARTESIAN_POINT('Ctrl Pts',(0.133711744422676,-0.0374104851459921,
-0.312257656033266));
#40747=CARTESIAN_POINT('Ctrl Pts',(0.104648535928131,0.0912527200882886,
-0.304380020033881));
#40748=CARTESIAN_POINT('Ctrl Pts',(-0.0188608286767674,0.137559602125903,
-0.296502384034497));
#40749=CARTESIAN_POINT('Ctrl Pts',(-0.125348141766317,0.0597178227261228,
-0.288624748035114));
#40750=CARTESIAN_POINT('Ctrl Pts',(-0.118707735863786,-0.0720197781272891,
-0.280747112035729));
#40751=CARTESIAN_POINT('Ctrl Pts',(-0.00493263138706642,-0.138758942569485,
-0.272869476036346));
#40752=CARTESIAN_POINT('Ctrl Pts',(0.113294213096355,-0.0802670310546098,
-0.264991840036961));
#40753=CARTESIAN_POINT('Ctrl Pts',(0.129272107399731,0.0506665298182005,
-0.257114204037578));
#40754=CARTESIAN_POINT('Ctrl Pts',(0.0285808717640413,0.1358731348154,-0.249236568038194));
#40755=CARTESIAN_POINT('Ctrl Pts',(-0.0979048334508719,0.0984531288613211,
-0.24135893203881));
#40756=CARTESIAN_POINT('Ctrl Pts',(-0.136030628971278,-0.0278216278612372,
-0.233481296039426));
#40757=CARTESIAN_POINT('Ctrl Pts',(-0.0513876737847133,-0.128987138809037,
-0.225603660040042));
#40758=CARTESIAN_POINT('Ctrl Pts',(0.0796330755882605,-0.113740706298137,
-0.217726024040658));
#40759=CARTESIAN_POINT('Ctrl Pts',(0.138784325562075,0.004157640156581,
-0.209848388041274));
#40760=CARTESIAN_POINT('Ctrl Pts',(0.0726815912474743,0.118303682479431,
-0.20197075204189));
#40761=CARTESIAN_POINT('Ctrl Pts',(-0.0590168712602702,0.125679687743678,
-0.194093116042506));
#40762=CARTESIAN_POINT('Ctrl Pts',(-0.137452126626887,0.0196287509851605,
-0.186215480043122));
#40763=CARTESIAN_POINT('Ctrl Pts',(-0.0918357182503099,-0.104137293264885,
-0.178337844043738));
#40764=CARTESIAN_POINT('Ctrl Pts',(0.0366631742567891,-0.133918582381201,
-0.170460208044354));
#40765=CARTESIAN_POINT('Ctrl Pts',(0.132073252696953,-0.042837259451921,
-0.16258257204497));
#40766=CARTESIAN_POINT('Ctrl Pts',(0.108286145990386,0.0869050379577989,
-0.154704936045586));
#40767=CARTESIAN_POINT('Ctrl Pts',(-0.0132300918964409,0.138214832825673,
-0.146827300046202));
#40768=CARTESIAN_POINT('Ctrl Pts',(-0.12280605959833,0.0647846111895411,
-0.138949664046818));
#40769=CARTESIAN_POINT('Ctrl Pts',(-0.121548566684335,-0.0671142421174204,
-0.131072028047434));
#40770=CARTESIAN_POINT('Ctrl Pts',(-0.01059248606553,-0.138441959744445,
-0.12319439204805));
#40771=CARTESIAN_POINT('Ctrl Pts',(0.10992336877787,-0.0848246534005071,
-0.115316756048666));
#40772=CARTESIAN_POINT('Ctrl Pts',(0.131232546291422,0.045347541159856,
-0.107439120049282));
#40773=CARTESIAN_POINT('Ctrl Pts',(0.034103170842127,0.134593310063775,
-0.099561484049898));
#40774=CARTESIAN_POINT('Ctrl Pts',(-0.0938043832643078,0.102367330978503,
-0.0916838480505142));
#40775=CARTESIAN_POINT('Ctrl Pts',(-0.137053117950997,-0.022245638482489,
-0.0838062120511301));
#40776=CARTESIAN_POINT('Ctrl Pts',(-0.0566095361633514,-0.126782421437836,
-0.0759285760517461));
#40777=CARTESIAN_POINT('Ctrl Pts',(0.0749231669276979,-0.116895737741183,
-0.0680509400523622));
#40778=CARTESIAN_POINT('Ctrl Pts',(0.138839849477423,-0.00151216593098895,
-0.0601733040529782));
#40779=CARTESIAN_POINT('Ctrl Pts',(0.0774472156514042,0.115240836226281,
-0.0522956680535942));
#40780=CARTESIAN_POINT('Ctrl Pts',(-0.0538322401122725,0.127979136607092,
-0.0444180320542103));
#40781=CARTESIAN_POINT('Ctrl Pts',(-0.136546513285208,0.0252321526219511,
-0.0365403960548262));
#40782=CARTESIAN_POINT('Ctrl Pts',(-0.0959906088420872,-0.10031924054277,
-0.0286627600554423));
#40783=CARTESIAN_POINT('Ctrl Pts',(0.0311293750964514,-0.135270378553972,
-0.0207851240560583));
#40784=CARTESIAN_POINT('Ctrl Pts',(0.130285619834645,-0.0482568461271642,
-0.0129074880566744));
#40785=CARTESIAN_POINT('Ctrl Pts',(0.111599842348155,0.0825450884163283,
-0.0050298520572903));
#40786=CARTESIAN_POINT('Ctrl Pts',(0.0323778461232267,0.119720372452911,
0.000221905275632274));
#40787=CARTESIAN_POINT('Ctrl Pts',(-0.00642735618905809,0.117599488593356,
0.00284778394209362));
#40788=CARTESIAN_POINT('Ctrl Pts',(-0.00798678478682509,0.146131905375825,
-0.0136499999999999));
#40789=CARTESIAN_POINT('Ctrl Pts',(0.0402334772246618,0.148767365811789,
-0.0162758786664613));
#40790=CARTESIAN_POINT('Ctrl Pts',(0.0894550401519313,0.125669922301901,
-0.0189017573329226));
#40791=CARTESIAN_POINT('Ctrl Pts',(0.117935719776108,0.087031604395481,
-0.0215276359993839));
#40792=CARTESIAN_POINT('Ctrl Pts',(0.146416399400285,0.0483932864890619,
-0.0241535146658452));
#40793=CARTESIAN_POINT('Ctrl Pts',(0.154156195721369,-0.00578590581389135,
-0.0267793933323067));
#40794=CARTESIAN_POINT('Ctrl Pts',(0.137490444808912,-0.0508963474626602,
-0.029405271998768));
#40795=CARTESIAN_POINT('Ctrl Pts',(0.120824693896455,-0.0960067891114296,
-0.0320311506652293));
#40796=CARTESIAN_POINT('Ctrl Pts',(0.0797533957504597,-0.132048480106016,
-0.0346570293316905));
#40797=CARTESIAN_POINT('Ctrl Pts',(0.0328906970073198,-0.142830807174188,
-0.0372829079981518));
#40798=CARTESIAN_POINT('Ctrl Pts',(-0.0139720017358201,-0.15361313424236,
-0.0399087866646132));
#40799=CARTESIAN_POINT('Ctrl Pts',(-0.0666261010761026,-0.139136097384114,
-0.0425346653310745));
#40800=CARTESIAN_POINT('Ctrl Pts',(-0.101352438392533,-0.105895390616129,
-0.0451605439975358));
#40801=CARTESIAN_POINT('Ctrl Pts',(-0.129670617078281,-0.0787886944702327,
-0.0473018611369268));
#40802=CARTESIAN_POINT('Ctrl Pts',(-0.146067080217357,-0.0392044155129423,
-0.0494431782763179));
#40803=CARTESIAN_POINT('Ctrl Pts',(-0.146419470807316,0.000121292426834327,
-0.0515844954157089));
#40804=CARTESIAN_POINT('Origin',(0.277715786349443,-0.0489687861020744,
0.04));
#40805=CARTESIAN_POINT('',(0.271097754137541,-0.0461628389679574,0.04));
#40806=CARTESIAN_POINT('',(0.27053717987482,-0.0493420135926708,0.04));
#40807=CARTESIAN_POINT('Origin',(0.,0.,0.04));
#40808=CARTESIAN_POINT('',(0.264913285560284,-0.0467113597924043,0.04));
#40809=CARTESIAN_POINT('',(0.29173382438227,-0.044332558140659,0.04));
#40810=CARTESIAN_POINT('',(0.264913285560284,-0.0467113597924043,0.04));
#40811=CARTESIAN_POINT('Origin',(0.264913285560284,-0.0467113597924043,
0.04));
#40812=CARTESIAN_POINT('',(0.27053717987482,-0.0493420135926708,0.285));
#40813=CARTESIAN_POINT('',(0.27053717987482,-0.0493420135926708,0.1425));
#40814=CARTESIAN_POINT('',(0.264913285560284,-0.0467113597924043,0.291));
#40815=CARTESIAN_POINT('',(0.264913285560284,-0.0467113597924043,0.04));
#40816=CARTESIAN_POINT('Ctrl Pts',(0.27053717987482,-0.0493420135926707,
0.285));
#40817=CARTESIAN_POINT('Ctrl Pts',(0.267694218594527,-0.048012179410566,
0.288035430631103));
#40818=CARTESIAN_POINT('Ctrl Pts',(0.264913285560284,-0.0467113597924043,
0.291));
#40819=CARTESIAN_POINT('Origin',(0.29173382438227,-0.044332558140659,0.04));
#40820=CARTESIAN_POINT('',(0.271097754137541,-0.0461628389679574,0.285));
#40821=CARTESIAN_POINT('',(0.271097754137541,-0.0461628389679574,0.1425));
#40822=CARTESIAN_POINT('Ctrl Pts',(0.264913285560284,-0.0467113597924043,
0.291));
#40823=CARTESIAN_POINT('Ctrl Pts',(0.267971414323715,-0.0464401243111941,
0.288035430631094));
#40824=CARTESIAN_POINT('Ctrl Pts',(0.271097754137541,-0.0461628389679575,
0.285));
#40825=CARTESIAN_POINT('Origin',(0.264993319061626,-0.0964496804178388,
0.04));
#40826=CARTESIAN_POINT('',(0.25896307723613,-0.0925371526922802,0.04));
#40827=CARTESIAN_POINT('',(0.257858961475997,-0.0955706858117092,0.04));
#40828=CARTESIAN_POINT('Origin',(0.,0.,0.04));
#40829=CARTESIAN_POINT('',(0.252777314991409,-0.0920034185546051,0.04));
#40830=CARTESIAN_POINT('',(0.279603464135123,-0.0943180939355711,0.04));
#40831=CARTESIAN_POINT('',(0.252777314991409,-0.0920034185546051,0.04));
#40832=CARTESIAN_POINT('Origin',(0.252777314991409,-0.0920034185546051,
0.04));
#40833=CARTESIAN_POINT('',(0.257858961475997,-0.0955706858117092,0.285));
#40834=CARTESIAN_POINT('',(0.257858961475997,-0.0955706858117092,0.1425));
#40835=CARTESIAN_POINT('',(0.252777314991409,-0.0920034185546051,0.291));
#40836=CARTESIAN_POINT('',(0.252777314991409,-0.0920034185546051,0.04));
#40837=CARTESIAN_POINT('Ctrl Pts',(0.257858961475997,-0.0955706858117092,
0.285));
#40838=CARTESIAN_POINT('Ctrl Pts',(0.255290114447966,-0.0937673797534469,
0.28803543063111));
#40839=CARTESIAN_POINT('Ctrl Pts',(0.252777314991409,-0.0920034185546051,
0.291));
#40840=CARTESIAN_POINT('Origin',(0.279603464135123,-0.0943180939355711,
0.04));
#40841=CARTESIAN_POINT('',(0.25896307723613,-0.0925371526922802,0.285));
#40842=CARTESIAN_POINT('',(0.25896307723613,-0.0925371526922802,0.1425));
#40843=CARTESIAN_POINT('Ctrl Pts',(0.252777314991409,-0.0920034185546051,
0.291));
#40844=CARTESIAN_POINT('Ctrl Pts',(0.255836083454352,-0.0922673422366557,
0.288035430631118));
#40845=CARTESIAN_POINT('Ctrl Pts',(0.25896307723613,-0.0925371526922802,
0.285));
#40846=CARTESIAN_POINT('Origin',(0.244219163867212,-0.141,0.04));
#40847=CARTESIAN_POINT('',(0.238959938274539,-0.136099771858106,0.04));
#40848=CARTESIAN_POINT('',(0.237345829015656,-0.138895491103459,0.04));
#40849=CARTESIAN_POINT('Origin',(0.,0.,0.04));
#40850=CARTESIAN_POINT('',(0.232960833618014,-0.1345,0.04));
#40851=CARTESIAN_POINT('',(0.258977494116409,-0.141437822173509,0.04));
#40852=CARTESIAN_POINT('',(0.232960833618014,-0.1345,0.04));
#40853=CARTESIAN_POINT('Origin',(0.232960833618014,-0.1345,0.04));
#40854=CARTESIAN_POINT('',(0.237345829015656,-0.138895491103459,0.285));
#40855=CARTESIAN_POINT('',(0.237345829015656,-0.138895491103459,0.1425));
#40856=CARTESIAN_POINT('',(0.232960833618014,-0.1345,0.291));
#40857=CARTESIAN_POINT('',(0.232960833618014,-0.1345,0.04));
#40858=CARTESIAN_POINT('Ctrl Pts',(0.237345829015656,-0.138895491103459,
0.285));
#40859=CARTESIAN_POINT('Ctrl Pts',(0.235129149356958,-0.136673505711122,
0.288035430631088));
#40860=CARTESIAN_POINT('Ctrl Pts',(0.232960833618014,-0.1345,0.291));
#40861=CARTESIAN_POINT('Origin',(0.258977494116409,-0.141437822173509,0.04));
#40862=CARTESIAN_POINT('',(0.238959938274539,-0.136099771858106,0.285));
#40863=CARTESIAN_POINT('',(0.238959938274539,-0.136099771858106,0.1425));
#40864=CARTESIAN_POINT('Ctrl Pts',(0.232960833618014,-0.1345,0.291));
#40865=CARTESIAN_POINT('Ctrl Pts',(0.235927302648582,-0.135291063657789,
0.288035430631094));
#40866=CARTESIAN_POINT('Ctrl Pts',(0.238959938274539,-0.136099771858106,
0.285));
#40867=CARTESIAN_POINT('Origin',(0.216024532959552,-0.181266105931604,0.04));
#40868=CARTESIAN_POINT('',(0.211696122508039,-0.175527068325832,0.04));
#40869=CARTESIAN_POINT('',(0.209621063643459,-0.17800002718254,0.04));
#40870=CARTESIAN_POINT('Origin',(0.,0.,0.04));
#40871=CARTESIAN_POINT('',(0.206065955199005,-0.172909867005679,0.04));
#40872=CARTESIAN_POINT('',(0.230482623987904,-0.184260033755696,0.04));
#40873=CARTESIAN_POINT('',(0.206065955199005,-0.172909867005679,0.04));
#40874=CARTESIAN_POINT('Origin',(0.206065955199005,-0.172909867005679,0.04));
#40875=CARTESIAN_POINT('',(0.209621063643459,-0.17800002718254,0.285));
#40876=CARTESIAN_POINT('',(0.209621063643459,-0.17800002718254,0.1425));
#40877=CARTESIAN_POINT('',(0.206065955199005,-0.172909867005679,0.291));
#40878=CARTESIAN_POINT('',(0.206065955199005,-0.172909867005679,0.04));
#40879=CARTESIAN_POINT('Ctrl Pts',(0.209621063643459,-0.17800002718254,
0.285));
#40880=CARTESIAN_POINT('Ctrl Pts',(0.207823904043776,-0.175426876357833,
0.288035430631146));
#40881=CARTESIAN_POINT('Ctrl Pts',(0.206065955199005,-0.172909867005679,
0.291));
#40882=CARTESIAN_POINT('Origin',(0.230482623987904,-0.184260033755696,0.04));
#40883=CARTESIAN_POINT('',(0.211696122508039,-0.175527068325832,0.285));
#40884=CARTESIAN_POINT('',(0.211696122508039,-0.175527068325832,0.1425));
#40885=CARTESIAN_POINT('Ctrl Pts',(0.206065955199005,-0.172909867005679,
0.291));
#40886=CARTESIAN_POINT('Ctrl Pts',(0.208849990136834,-0.174204034570282,
0.288035430631042));
#40887=CARTESIAN_POINT('Ctrl Pts',(0.211696122508039,-0.175527068325832,
0.285));
#40888=CARTESIAN_POINT('Origin',(0.181266105931604,-0.216024532959552,0.04));
#40889=CARTESIAN_POINT('',(0.17800002718254,-0.209621063643459,0.04));
#40890=CARTESIAN_POINT('',(0.175527068325832,-0.211696122508039,0.04));
#40891=CARTESIAN_POINT('Origin',(0.,0.,0.04));
#40892=CARTESIAN_POINT('',(0.172909867005679,-0.206065955199005,0.04));
#40893=CARTESIAN_POINT('',(0.194984655959362,-0.221483597452293,0.04));
#40894=CARTESIAN_POINT('',(0.172909867005679,-0.206065955199005,0.04));
#40895=CARTESIAN_POINT('Origin',(0.172909867005679,-0.206065955199005,0.04));
#40896=CARTESIAN_POINT('',(0.175527068325832,-0.211696122508039,0.285));
#40897=CARTESIAN_POINT('',(0.175527068325832,-0.211696122508039,0.1425));
#40898=CARTESIAN_POINT('',(0.172909867005679,-0.206065955199005,0.291));
#40899=CARTESIAN_POINT('',(0.172909867005679,-0.206065955199005,0.04));
#40900=CARTESIAN_POINT('Ctrl Pts',(0.175527068325832,-0.211696122508039,
0.285));
#40901=CARTESIAN_POINT('Ctrl Pts',(0.174204034570244,-0.208849990136752,
0.288035430631129));
#40902=CARTESIAN_POINT('Ctrl Pts',(0.172909867005679,-0.206065955199005,
0.291));
#40903=CARTESIAN_POINT('Origin',(0.194984655959362,-0.221483597452293,0.04));
#40904=CARTESIAN_POINT('',(0.17800002718254,-0.209621063643459,0.285));
#40905=CARTESIAN_POINT('',(0.17800002718254,-0.209621063643459,0.1425));
#40906=CARTESIAN_POINT('Ctrl Pts',(0.172909867005679,-0.206065955199005,
0.291));
#40907=CARTESIAN_POINT('Ctrl Pts',(0.175426876357872,-0.207823904043804,
0.2880354306311));
#40908=CARTESIAN_POINT('Ctrl Pts',(0.17800002718254,-0.209621063643459,
0.285));
#40909=CARTESIAN_POINT('Origin',(0.141,-0.244219163867212,0.04));
#40910=CARTESIAN_POINT('',(0.138895491103459,-0.237345829015656,0.04));
#40911=CARTESIAN_POINT('',(0.136099771858106,-0.238959938274539,0.04));
#40912=CARTESIAN_POINT('Origin',(0.,0.,0.04));
#40913=CARTESIAN_POINT('',(0.1345,-0.232960833618014,0.04));
#40914=CARTESIAN_POINT('',(0.153562177826491,-0.251977494116409,0.04));
#40915=CARTESIAN_POINT('',(0.1345,-0.232960833618014,0.04));
#40916=CARTESIAN_POINT('Origin',(0.1345,-0.232960833618014,0.04));
#40917=CARTESIAN_POINT('',(0.136099771858106,-0.238959938274539,0.285));
#40918=CARTESIAN_POINT('',(0.136099771858106,-0.238959938274539,0.1425));
#40919=CARTESIAN_POINT('',(0.1345,-0.232960833618014,0.291));
#40920=CARTESIAN_POINT('',(0.1345,-0.232960833618014,0.04));
#40921=CARTESIAN_POINT('Ctrl Pts',(0.136099771858106,-0.238959938274539,
0.285));
#40922=CARTESIAN_POINT('Ctrl Pts',(0.135291063657772,-0.23592730264852,
0.288035430631155));
#40923=CARTESIAN_POINT('Ctrl Pts',(0.1345,-0.232960833618014,0.291));
#40924=CARTESIAN_POINT('Origin',(0.153562177826491,-0.251977494116409,0.04));
#40925=CARTESIAN_POINT('',(0.138895491103459,-0.237345829015656,0.285));
#40926=CARTESIAN_POINT('',(0.138895491103459,-0.237345829015656,0.1425));
#40927=CARTESIAN_POINT('Ctrl Pts',(0.1345,-0.232960833618014,0.291));
#40928=CARTESIAN_POINT('Ctrl Pts',(0.136673505711114,-0.23512914935695,
0.288035430631099));
#40929=CARTESIAN_POINT('Ctrl Pts',(0.138895491103459,-0.237345829015656,
0.285));
#40930=CARTESIAN_POINT('Origin',(0.0964496804178385,-0.264993319061626,
0.04));
#40931=CARTESIAN_POINT('',(0.0955706858117088,-0.257858961475997,0.04));
#40932=CARTESIAN_POINT('',(0.0925371526922799,-0.25896307723613,0.04));
#40933=CARTESIAN_POINT('Origin',(0.,0.,0.04));
#40934=CARTESIAN_POINT('',(0.0920034185546048,-0.252777314991409,0.04));
#40935=CARTESIAN_POINT('',(0.107473790626574,-0.274815182128563,0.04));
#40936=CARTESIAN_POINT('',(0.0920034185546048,-0.252777314991409,0.04));
#40937=CARTESIAN_POINT('Origin',(0.0920034185546048,-0.252777314991409,
0.04));
#40938=CARTESIAN_POINT('',(0.0925371526922799,-0.25896307723613,0.285));
#40939=CARTESIAN_POINT('',(0.0925371526922799,-0.25896307723613,0.1425));
#40940=CARTESIAN_POINT('',(0.0920034185546048,-0.252777314991409,0.291));
#40941=CARTESIAN_POINT('',(0.0920034185546048,-0.252777314991409,0.04));
#40942=CARTESIAN_POINT('Ctrl Pts',(0.0925371526922799,-0.25896307723613,
0.285));
#40943=CARTESIAN_POINT('Ctrl Pts',(0.0922673422366487,-0.255836083454274,
0.288035430631194));
#40944=CARTESIAN_POINT('Ctrl Pts',(0.0920034185546048,-0.252777314991409,
0.291));
#40945=CARTESIAN_POINT('Origin',(0.107473790626574,-0.274815182128563,0.04));
#40946=CARTESIAN_POINT('',(0.0955706858117089,-0.257858961475997,0.285));
#40947=CARTESIAN_POINT('',(0.0955706858117089,-0.257858961475997,0.1425));
#40948=CARTESIAN_POINT('Ctrl Pts',(0.0920034185546048,-0.252777314991409,
0.291));
#40949=CARTESIAN_POINT('Ctrl Pts',(0.0937673797534969,-0.255290114448038,
0.288035430631026));
#40950=CARTESIAN_POINT('Ctrl Pts',(0.0955706858117088,-0.257858961475997,
0.285));
#40951=CARTESIAN_POINT('Origin',(0.0489687861020743,-0.277715786349443,
0.04));
#40952=CARTESIAN_POINT('',(0.0493420135926707,-0.27053717987482,0.04));
#40953=CARTESIAN_POINT('',(0.0461628389679573,-0.271097754137541,0.04));
#40954=CARTESIAN_POINT('Origin',(0.,0.,0.04));
#40955=CARTESIAN_POINT('',(0.0467113597924042,-0.264913285560284,0.04));
#40956=CARTESIAN_POINT('',(0.0581198666828298,-0.289302749894933,0.04));
#40957=CARTESIAN_POINT('',(0.0467113597924042,-0.264913285560284,0.04));
#40958=CARTESIAN_POINT('Origin',(0.0467113597924042,-0.264913285560284,
0.04));
#40959=CARTESIAN_POINT('',(0.0461628389679573,-0.271097754137541,0.285));
#40960=CARTESIAN_POINT('',(0.0461628389679573,-0.271097754137541,0.1425));
#40961=CARTESIAN_POINT('',(0.0467113597924042,-0.264913285560284,0.291));
#40962=CARTESIAN_POINT('',(0.0467113597924042,-0.264913285560284,0.04));
#40963=CARTESIAN_POINT('Ctrl Pts',(0.0461628389679573,-0.271097754137541,
0.285));
#40964=CARTESIAN_POINT('Ctrl Pts',(0.0464401243112015,-0.26797141432363,
0.288035430631177));
#40965=CARTESIAN_POINT('Ctrl Pts',(0.0467113597924042,-0.264913285560284,
0.291));
#40966=CARTESIAN_POINT('Origin',(0.0581198666828298,-0.289302749894933,
0.04));
#40967=CARTESIAN_POINT('',(0.0493420135926707,-0.27053717987482,0.285));
#40968=CARTESIAN_POINT('',(0.0493420135926707,-0.27053717987482,0.1425));
#40969=CARTESIAN_POINT('Ctrl Pts',(0.0467113597924042,-0.264913285560284,
0.291));
#40970=CARTESIAN_POINT('Ctrl Pts',(0.0480121794105309,-0.267694218594452,
0.288035430631183));
#40971=CARTESIAN_POINT('Ctrl Pts',(0.0493420135926707,-0.27053717987482,
0.285));
#40972=CARTESIAN_POINT('Origin',(-4.85722573273506E-17,-0.282,0.04));
#40973=CARTESIAN_POINT('',(0.00161410925888288,-0.274995262961565,0.04));
#40974=CARTESIAN_POINT('',(-0.00161410925888299,-0.274995262961565,0.04));
#40975=CARTESIAN_POINT('Origin',(0.,0.,0.04));
#40976=CARTESIAN_POINT('',(-6.24500451351651E-17,-0.269,0.04));
#40977=CARTESIAN_POINT('',(0.00699999999999995,-0.295,0.04));
#40978=CARTESIAN_POINT('',(-6.24500451351651E-17,-0.269,0.04));
#40979=CARTESIAN_POINT('Origin',(-6.24500451351651E-17,-0.269,0.04));
#40980=CARTESIAN_POINT('',(-0.00161410925888297,-0.274995262961565,0.285));
#40981=CARTESIAN_POINT('',(-0.00161410925888297,-0.274995262961565,0.1425));
#40982=CARTESIAN_POINT('',(-6.2450045135165E-17,-0.269,0.291));
#40983=CARTESIAN_POINT('',(-6.24500451351651E-17,-0.269,0.04));
#40984=CARTESIAN_POINT('Ctrl Pts',(-0.00161410925888296,-0.274995262961565,
0.285));
#40985=CARTESIAN_POINT('Ctrl Pts',(-0.000798153291622722,-0.271964569368884,
0.288035430631116));
#40986=CARTESIAN_POINT('Ctrl Pts',(-6.24500451351651E-17,-0.269,0.291));
#40987=CARTESIAN_POINT('Origin',(0.00699999999999995,-0.295,0.04));
#40988=CARTESIAN_POINT('',(0.00161410925888286,-0.274995262961565,0.285));
#40989=CARTESIAN_POINT('',(0.00161410925888286,-0.274995262961565,0.1425));
#40990=CARTESIAN_POINT('Ctrl Pts',(-6.2450045135165E-17,-0.269,0.291));
#40991=CARTESIAN_POINT('Ctrl Pts',(0.000798153291617013,-0.271964569368863,
0.288035430631137));
#40992=CARTESIAN_POINT('Ctrl Pts',(0.00161410925888284,-0.274995262961565,
0.285));
#40993=CARTESIAN_POINT('Origin',(-0.0489687861020744,-0.277715786349443,
0.04));
#40994=CARTESIAN_POINT('',(-0.0461628389679574,-0.271097754137541,0.04));
#40995=CARTESIAN_POINT('',(-0.0493420135926708,-0.27053717987482,0.04));
#40996=CARTESIAN_POINT('Origin',(0.,0.,0.04));
#40997=CARTESIAN_POINT('',(-0.0467113597924043,-0.264913285560284,0.04));
#40998=CARTESIAN_POINT('',(-0.044332558140659,-0.29173382438227,0.04));
#40999=CARTESIAN_POINT('',(-0.0467113597924043,-0.264913285560284,0.04));
#41000=CARTESIAN_POINT('Origin',(-0.0467113597924043,-0.264913285560284,
0.04));
#41001=CARTESIAN_POINT('',(-0.0493420135926708,-0.27053717987482,0.285));
#41002=CARTESIAN_POINT('',(-0.0493420135926708,-0.27053717987482,0.1425));
#41003=CARTESIAN_POINT('',(-0.0467113597924043,-0.264913285560284,0.291));
#41004=CARTESIAN_POINT('',(-0.0467113597924043,-0.264913285560284,0.04));
#41005=CARTESIAN_POINT('Ctrl Pts',(-0.0493420135926708,-0.27053717987482,
0.285));
#41006=CARTESIAN_POINT('Ctrl Pts',(-0.0480121794105265,-0.267694218594442,
0.288035430631193));
#41007=CARTESIAN_POINT('Ctrl Pts',(-0.0467113597924043,-0.264913285560284,
0.291));
#41008=CARTESIAN_POINT('Origin',(-0.044332558140659,-0.29173382438227,0.04));
#41009=CARTESIAN_POINT('',(-0.0461628389679574,-0.271097754137541,0.285));
#41010=CARTESIAN_POINT('',(-0.0461628389679574,-0.271097754137541,0.1425));
#41011=CARTESIAN_POINT('Ctrl Pts',(-0.0467113597924043,-0.264913285560284,
0.291));
#41012=CARTESIAN_POINT('Ctrl Pts',(-0.046440124311189,-0.267971414323772,
0.288035430631039));
#41013=CARTESIAN_POINT('Ctrl Pts',(-0.0461628389679575,-0.271097754137541,
0.285));
#41014=CARTESIAN_POINT('Origin',(-0.0964496804178388,-0.264993319061626,
0.04));
#41015=CARTESIAN_POINT('',(-0.0925371526922802,-0.25896307723613,0.04));
#41016=CARTESIAN_POINT('',(-0.0955706858117092,-0.257858961475997,0.04));
#41017=CARTESIAN_POINT('Origin',(0.,0.,0.04));
#41018=CARTESIAN_POINT('',(-0.0920034185546051,-0.252777314991409,0.04));
#41019=CARTESIAN_POINT('',(-0.0943180939355711,-0.279603464135123,0.04));
#41020=CARTESIAN_POINT('',(-0.0920034185546051,-0.252777314991409,0.04));
#41021=CARTESIAN_POINT('Origin',(-0.0920034185546051,-0.252777314991409,
0.04));
#41022=CARTESIAN_POINT('',(-0.0955706858117092,-0.257858961475997,0.285));
#41023=CARTESIAN_POINT('',(-0.0955706858117092,-0.257858961475997,0.1425));
#41024=CARTESIAN_POINT('',(-0.0920034185546051,-0.252777314991409,0.291));
#41025=CARTESIAN_POINT('',(-0.0920034185546051,-0.252777314991409,0.04));
#41026=CARTESIAN_POINT('Ctrl Pts',(-0.0955706858117091,-0.257858961475997,
0.285));
#41027=CARTESIAN_POINT('Ctrl Pts',(-0.0937673797534664,-0.255290114447994,
0.288035430631078));
#41028=CARTESIAN_POINT('Ctrl Pts',(-0.0920034185546051,-0.252777314991409,
0.291));
#41029=CARTESIAN_POINT('Origin',(-0.0943180939355711,-0.279603464135123,
0.04));
#41030=CARTESIAN_POINT('',(-0.0925371526922802,-0.25896307723613,0.285));
#41031=CARTESIAN_POINT('',(-0.0925371526922802,-0.25896307723613,0.1425));
#41032=CARTESIAN_POINT('Ctrl Pts',(-0.0920034185546051,-0.252777314991409,
0.291));
#41033=CARTESIAN_POINT('Ctrl Pts',(-0.0922673422366578,-0.255836083454375,
0.288035430631095));
#41034=CARTESIAN_POINT('Ctrl Pts',(-0.0925371526922802,-0.25896307723613,
0.285));
#41035=CARTESIAN_POINT('Origin',(-0.141,-0.244219163867212,0.04));
#41036=CARTESIAN_POINT('',(-0.136099771858106,-0.238959938274539,0.04));
#41037=CARTESIAN_POINT('',(-0.138895491103459,-0.237345829015656,0.04));
#41038=CARTESIAN_POINT('Origin',(0.,0.,0.04));
#41039=CARTESIAN_POINT('',(-0.1345,-0.232960833618014,0.04));
#41040=CARTESIAN_POINT('',(-0.141437822173509,-0.258977494116409,0.04));
#41041=CARTESIAN_POINT('',(-0.1345,-0.232960833618014,0.04));
#41042=CARTESIAN_POINT('Origin',(-0.1345,-0.232960833618014,0.04));
#41043=CARTESIAN_POINT('',(-0.138895491103459,-0.237345829015656,0.285));
#41044=CARTESIAN_POINT('',(-0.138895491103459,-0.237345829015656,0.1425));
#41045=CARTESIAN_POINT('',(-0.1345,-0.232960833618014,0.291));
#41046=CARTESIAN_POINT('',(-0.1345,-0.232960833618014,0.04));
#41047=CARTESIAN_POINT('Ctrl Pts',(-0.138895491103459,-0.237345829015656,
0.285));
#41048=CARTESIAN_POINT('Ctrl Pts',(-0.136673505711122,-0.235129149356958,
0.288035430631088));
#41049=CARTESIAN_POINT('Ctrl Pts',(-0.1345,-0.232960833618014,0.291));
#41050=CARTESIAN_POINT('Origin',(-0.141437822173509,-0.258977494116409,
0.04));
#41051=CARTESIAN_POINT('',(-0.136099771858106,-0.238959938274539,0.285));
#41052=CARTESIAN_POINT('',(-0.136099771858106,-0.238959938274539,0.1425));
#41053=CARTESIAN_POINT('Ctrl Pts',(-0.1345,-0.232960833618014,0.291));
#41054=CARTESIAN_POINT('Ctrl Pts',(-0.135291063657789,-0.235927302648582,
0.288035430631094));
#41055=CARTESIAN_POINT('Ctrl Pts',(-0.136099771858106,-0.238959938274539,
0.285));
#41056=CARTESIAN_POINT('Origin',(-0.181266105931604,-0.216024532959552,
0.04));
#41057=CARTESIAN_POINT('',(-0.175527068325832,-0.211696122508039,0.04));
#41058=CARTESIAN_POINT('',(-0.17800002718254,-0.209621063643459,0.04));
#41059=CARTESIAN_POINT('Origin',(0.,0.,0.04));
#41060=CARTESIAN_POINT('',(-0.172909867005679,-0.206065955199005,0.04));
#41061=CARTESIAN_POINT('',(-0.184260033755696,-0.230482623987904,0.04));
#41062=CARTESIAN_POINT('',(-0.172909867005679,-0.206065955199005,0.04));
#41063=CARTESIAN_POINT('Origin',(-0.172909867005679,-0.206065955199005,
0.04));
#41064=CARTESIAN_POINT('',(-0.17800002718254,-0.209621063643459,0.285));
#41065=CARTESIAN_POINT('',(-0.17800002718254,-0.209621063643459,0.1425));
#41066=CARTESIAN_POINT('',(-0.172909867005679,-0.206065955199005,0.291));
#41067=CARTESIAN_POINT('',(-0.172909867005679,-0.206065955199005,0.04));
#41068=CARTESIAN_POINT('Ctrl Pts',(-0.17800002718254,-0.209621063643459,
0.285));
#41069=CARTESIAN_POINT('Ctrl Pts',(-0.175426876357765,-0.207823904043728,
0.288035430631226));
#41070=CARTESIAN_POINT('Ctrl Pts',(-0.172909867005679,-0.206065955199005,
0.291));
#41071=CARTESIAN_POINT('Origin',(-0.184260033755696,-0.230482623987904,
0.04));
#41072=CARTESIAN_POINT('',(-0.175527068325832,-0.211696122508039,0.285));
#41073=CARTESIAN_POINT('',(-0.175527068325832,-0.211696122508039,0.1425));
#41074=CARTESIAN_POINT('Ctrl Pts',(-0.172909867005679,-0.206065955199005,
0.291));
#41075=CARTESIAN_POINT('Ctrl Pts',(-0.174204034570293,-0.208849990136858,
0.288035430631017));
#41076=CARTESIAN_POINT('Ctrl Pts',(-0.175527068325832,-0.211696122508039,
0.285));
#41077=CARTESIAN_POINT('Origin',(-0.216024532959552,-0.181266105931604,
0.04));
#41078=CARTESIAN_POINT('',(-0.209621063643459,-0.17800002718254,0.04));
#41079=CARTESIAN_POINT('',(-0.211696122508039,-0.175527068325832,0.04));
#41080=CARTESIAN_POINT('Origin',(0.,0.,0.04));
#41081=CARTESIAN_POINT('',(-0.206065955199005,-0.172909867005679,0.04));
#41082=CARTESIAN_POINT('',(-0.221483597452293,-0.194984655959362,0.04));
#41083=CARTESIAN_POINT('',(-0.206065955199005,-0.172909867005679,0.04));
#41084=CARTESIAN_POINT('Origin',(-0.206065955199005,-0.172909867005679,
0.04));
#41085=CARTESIAN_POINT('',(-0.211696122508039,-0.175527068325832,0.285));
#41086=CARTESIAN_POINT('',(-0.211696122508039,-0.175527068325832,0.1425));
#41087=CARTESIAN_POINT('',(-0.206065955199005,-0.172909867005679,0.291));
#41088=CARTESIAN_POINT('',(-0.206065955199005,-0.172909867005679,0.04));
#41089=CARTESIAN_POINT('Ctrl Pts',(-0.211696122508039,-0.175527068325832,
0.285));
#41090=CARTESIAN_POINT('Ctrl Pts',(-0.208849990136656,-0.174204034570199,
0.288035430631232));
#41091=CARTESIAN_POINT('Ctrl Pts',(-0.206065955199005,-0.172909867005679,
0.291));
#41092=CARTESIAN_POINT('Origin',(-0.221483597452293,-0.194984655959362,
0.04));
#41093=CARTESIAN_POINT('',(-0.209621063643459,-0.17800002718254,0.285));
#41094=CARTESIAN_POINT('',(-0.209621063643459,-0.17800002718254,0.1425));
#41095=CARTESIAN_POINT('Ctrl Pts',(-0.206065955199005,-0.172909867005679,
0.291));
#41096=CARTESIAN_POINT('Ctrl Pts',(-0.207823904043843,-0.175426876357928,
0.288035430631034));
#41097=CARTESIAN_POINT('Ctrl Pts',(-0.209621063643459,-0.17800002718254,
0.285));
#41098=CARTESIAN_POINT('Origin',(-0.244219163867212,-0.141,0.04));
#41099=CARTESIAN_POINT('',(-0.237345829015656,-0.138895491103459,0.04));
#41100=CARTESIAN_POINT('',(-0.238959938274539,-0.136099771858106,0.04));
#41101=CARTESIAN_POINT('Origin',(0.,0.,0.04));
#41102=CARTESIAN_POINT('',(-0.232960833618014,-0.1345,0.04));
#41103=CARTESIAN_POINT('',(-0.25197749411641,-0.153562177826491,0.04));
#41104=CARTESIAN_POINT('',(-0.232960833618014,-0.1345,0.04));
#41105=CARTESIAN_POINT('Origin',(-0.232960833618014,-0.1345,0.04));
#41106=CARTESIAN_POINT('',(-0.238959938274539,-0.136099771858106,0.285));
#41107=CARTESIAN_POINT('',(-0.238959938274539,-0.136099771858106,0.1425));
#41108=CARTESIAN_POINT('',(-0.232960833618014,-0.1345,0.291));
#41109=CARTESIAN_POINT('',(-0.232960833618014,-0.1345,0.04));
#41110=CARTESIAN_POINT('Ctrl Pts',(-0.238959938274539,-0.136099771858106,
0.285));
#41111=CARTESIAN_POINT('Ctrl Pts',(-0.23592730264851,-0.135291063657769,
0.288035430631166));
#41112=CARTESIAN_POINT('Ctrl Pts',(-0.232960833618014,-0.1345,0.291));
#41113=CARTESIAN_POINT('Origin',(-0.25197749411641,-0.153562177826491,0.04));
#41114=CARTESIAN_POINT('',(-0.237345829015656,-0.138895491103459,0.285));
#41115=CARTESIAN_POINT('',(-0.237345829015656,-0.138895491103459,0.1425));
#41116=CARTESIAN_POINT('Ctrl Pts',(-0.232960833618014,-0.1345,0.291));
#41117=CARTESIAN_POINT('Ctrl Pts',(-0.235129149356959,-0.136673505711123,
0.288035430631086));
#41118=CARTESIAN_POINT('Ctrl Pts',(-0.237345829015656,-0.138895491103459,
0.285));
#41119=CARTESIAN_POINT('Origin',(-0.264993319061626,-0.0964496804178386,
0.04));
#41120=CARTESIAN_POINT('',(-0.257858961475997,-0.095570685811709,0.04));
#41121=CARTESIAN_POINT('',(-0.25896307723613,-0.09253715269228,0.04));
#41122=CARTESIAN_POINT('Origin',(0.,0.,0.04));
#41123=CARTESIAN_POINT('',(-0.252777314991409,-0.0920034185546049,0.04));
#41124=CARTESIAN_POINT('',(-0.274815182128563,-0.107473790626574,0.04));
#41125=CARTESIAN_POINT('',(-0.252777314991409,-0.0920034185546049,0.04));
#41126=CARTESIAN_POINT('Origin',(-0.252777314991409,-0.0920034185546049,
0.04));
#41127=CARTESIAN_POINT('',(-0.25896307723613,-0.09253715269228,0.285));
#41128=CARTESIAN_POINT('',(-0.25896307723613,-0.09253715269228,0.1425));
#41129=CARTESIAN_POINT('',(-0.252777314991409,-0.0920034185546049,0.291));
#41130=CARTESIAN_POINT('',(-0.252777314991409,-0.0920034185546049,0.04));
#41131=CARTESIAN_POINT('Ctrl Pts',(-0.25896307723613,-0.09253715269228,
0.285));
#41132=CARTESIAN_POINT('Ctrl Pts',(-0.255836083454338,-0.0922673422366543,
0.288035430631132));
#41133=CARTESIAN_POINT('Ctrl Pts',(-0.252777314991409,-0.0920034185546049,
0.291));
#41134=CARTESIAN_POINT('Origin',(-0.274815182128563,-0.107473790626574,
0.04));
#41135=CARTESIAN_POINT('',(-0.257858961475997,-0.095570685811709,0.285));
#41136=CARTESIAN_POINT('',(-0.257858961475997,-0.095570685811709,0.1425));
#41137=CARTESIAN_POINT('Ctrl Pts',(-0.252777314991409,-0.0920034185546049,
0.291));
#41138=CARTESIAN_POINT('Ctrl Pts',(-0.255290114448016,-0.0937673797534821,
0.288035430631051));
#41139=CARTESIAN_POINT('Ctrl Pts',(-0.257858961475997,-0.0955706858117089,
0.285));
#41140=CARTESIAN_POINT('Origin',(-0.277715786349443,-0.0489687861020743,
0.04));
#41141=CARTESIAN_POINT('',(-0.27053717987482,-0.0493420135926707,0.04));
#41142=CARTESIAN_POINT('',(-0.271097754137541,-0.0461628389679573,0.04));
#41143=CARTESIAN_POINT('Origin',(0.,0.,0.04));
#41144=CARTESIAN_POINT('',(-0.264913285560284,-0.0467113597924042,0.04));
#41145=CARTESIAN_POINT('',(-0.289302749894933,-0.0581198666828298,0.04));
#41146=CARTESIAN_POINT('',(-0.264913285560284,-0.0467113597924042,0.04));
#41147=CARTESIAN_POINT('Origin',(-0.264913285560284,-0.0467113597924042,
0.04));
#41148=CARTESIAN_POINT('',(-0.271097754137541,-0.0461628389679573,0.285));
#41149=CARTESIAN_POINT('',(-0.271097754137541,-0.0461628389679573,0.1425));
#41150=CARTESIAN_POINT('',(-0.264913285560284,-0.0467113597924042,0.291));
#41151=CARTESIAN_POINT('',(-0.264913285560284,-0.0467113597924042,0.04));
#41152=CARTESIAN_POINT('Ctrl Pts',(-0.271097754137541,-0.0461628389679573,
0.285));
#41153=CARTESIAN_POINT('Ctrl Pts',(-0.267971414323669,-0.0464401243111981,
0.288035430631139));
#41154=CARTESIAN_POINT('Ctrl Pts',(-0.264913285560284,-0.0467113597924042,
0.291));
#41155=CARTESIAN_POINT('Origin',(-0.289302749894933,-0.0581198666828298,
0.04));
#41156=CARTESIAN_POINT('',(-0.27053717987482,-0.0493420135926707,0.285));
#41157=CARTESIAN_POINT('',(-0.27053717987482,-0.0493420135926707,0.1425));
#41158=CARTESIAN_POINT('Ctrl Pts',(-0.264913285560284,-0.0467113597924042,
0.291));
#41159=CARTESIAN_POINT('Ctrl Pts',(-0.2676942185945,-0.0480121794105537,
0.288035430631131));
#41160=CARTESIAN_POINT('Ctrl Pts',(-0.27053717987482,-0.0493420135926707,
0.285));
#41161=CARTESIAN_POINT('Origin',(-0.282,2.77555756156289E-17,0.04));
#41162=CARTESIAN_POINT('',(-0.274995262961565,-0.0016141092588829,0.04));
#41163=CARTESIAN_POINT('',(-0.275,-3.36777869765522E-17,0.04));
#41164=CARTESIAN_POINT('Origin',(0.,0.,0.04));
#41165=CARTESIAN_POINT('',(-0.269,4.16333634234434E-17,0.04));
#41166=CARTESIAN_POINT('',(-0.295,-0.00699999999999998,0.04));
#41167=CARTESIAN_POINT('',(-0.274995262961565,0.00161410925888296,0.04));
#41168=CARTESIAN_POINT('',(-0.269,4.16333634234434E-17,0.04));
#41169=CARTESIAN_POINT('Origin',(0.,0.,0.04));
#41170=CARTESIAN_POINT('Origin',(-0.269,4.16333634234434E-17,0.04));
#41171=CARTESIAN_POINT('',(-0.274995262961565,0.00161410925888297,0.285));
#41172=CARTESIAN_POINT('',(-0.274995262961565,0.00161410925888297,0.1425));
#41173=CARTESIAN_POINT('',(-0.269,4.16333634234434E-17,0.291));
#41174=CARTESIAN_POINT('',(-0.269,4.16333634234434E-17,0.04));
#41175=CARTESIAN_POINT('Ctrl Pts',(-0.274995262961565,0.00161410925888294,
0.285));
#41176=CARTESIAN_POINT('Ctrl Pts',(-0.271964569368884,0.000798153291622702,
0.288035430631116));
#41177=CARTESIAN_POINT('Ctrl Pts',(-0.269,4.16333634234434E-17,0.291));
#41178=CARTESIAN_POINT('Origin',(-0.295,-0.00699999999999998,0.04));
#41179=CARTESIAN_POINT('',(-0.274995262961565,-0.0016141092588829,0.285));
#41180=CARTESIAN_POINT('',(-0.274995262961565,-0.0016141092588829,0.1425));
#41181=CARTESIAN_POINT('Ctrl Pts',(-0.269,4.16333634234434E-17,0.291));
#41182=CARTESIAN_POINT('Ctrl Pts',(-0.271964569368901,-0.000798153291627193,
0.288035430631099));
#41183=CARTESIAN_POINT('Ctrl Pts',(-0.274995262961565,-0.00161410925888289,
0.285));
#41184=CARTESIAN_POINT('Origin',(-0.277715786349443,0.0489687861020745,
0.04));
#41185=CARTESIAN_POINT('',(-0.271097754137541,0.0461628389679575,0.04));
#41186=CARTESIAN_POINT('',(-0.27053717987482,0.0493420135926709,0.04));
#41187=CARTESIAN_POINT('Origin',(0.,0.,0.04));
#41188=CARTESIAN_POINT('',(-0.264913285560284,0.0467113597924044,0.04));
#41189=CARTESIAN_POINT('',(-0.29173382438227,0.0443325581406591,0.04));
#41190=CARTESIAN_POINT('',(-0.264913285560284,0.0467113597924044,0.04));
#41191=CARTESIAN_POINT('Origin',(-0.264913285560284,0.0467113597924044,
0.04));
#41192=CARTESIAN_POINT('',(-0.27053717987482,0.0493420135926709,0.285));
#41193=CARTESIAN_POINT('',(-0.27053717987482,0.0493420135926709,0.1425));
#41194=CARTESIAN_POINT('',(-0.264913285560284,0.0467113597924044,0.291));
#41195=CARTESIAN_POINT('',(-0.264913285560284,0.0467113597924044,0.04));
#41196=CARTESIAN_POINT('Ctrl Pts',(-0.27053717987482,0.0493420135926709,
0.285));
#41197=CARTESIAN_POINT('Ctrl Pts',(-0.267694218594536,0.0480121794105704,
0.288035430631093));
#41198=CARTESIAN_POINT('Ctrl Pts',(-0.264913285560284,0.0467113597924044,
0.291));
#41199=CARTESIAN_POINT('Origin',(-0.29173382438227,0.0443325581406591,0.04));
#41200=CARTESIAN_POINT('',(-0.271097754137541,0.0461628389679575,0.285));
#41201=CARTESIAN_POINT('',(-0.271097754137541,0.0461628389679575,0.1425));
#41202=CARTESIAN_POINT('Ctrl Pts',(-0.264913285560284,0.0467113597924044,
0.291));
#41203=CARTESIAN_POINT('Ctrl Pts',(-0.267971414323744,0.0464401243111915,
0.288035430631066));
#41204=CARTESIAN_POINT('Ctrl Pts',(-0.271097754137541,0.0461628389679575,
0.285));
#41205=CARTESIAN_POINT('Origin',(-0.264993319061626,0.0964496804178386,
0.04));
#41206=CARTESIAN_POINT('',(-0.25896307723613,0.09253715269228,0.04));
#41207=CARTESIAN_POINT('',(-0.257858961475997,0.095570685811709,0.04));
#41208=CARTESIAN_POINT('Origin',(0.,0.,0.04));
#41209=CARTESIAN_POINT('',(-0.252777314991409,0.0920034185546049,0.04));
#41210=CARTESIAN_POINT('',(-0.279603464135123,0.094318093935571,0.04));
#41211=CARTESIAN_POINT('',(-0.252777314991409,0.0920034185546049,0.04));
#41212=CARTESIAN_POINT('Origin',(-0.252777314991409,0.0920034185546049,
0.04));
#41213=CARTESIAN_POINT('',(-0.257858961475997,0.095570685811709,0.285));
#41214=CARTESIAN_POINT('',(-0.257858961475997,0.095570685811709,0.1425));
#41215=CARTESIAN_POINT('',(-0.252777314991409,0.0920034185546049,0.291));
#41216=CARTESIAN_POINT('',(-0.252777314991409,0.0920034185546049,0.04));
#41217=CARTESIAN_POINT('Ctrl Pts',(-0.257858961475997,0.095570685811709,
0.285));
#41218=CARTESIAN_POINT('Ctrl Pts',(-0.255290114447956,0.0937673797534397,
0.288035430631122));
#41219=CARTESIAN_POINT('Ctrl Pts',(-0.252777314991409,0.0920034185546049,
0.291));
#41220=CARTESIAN_POINT('Origin',(-0.279603464135123,0.094318093935571,0.04));
#41221=CARTESIAN_POINT('',(-0.25896307723613,0.09253715269228,0.285));
#41222=CARTESIAN_POINT('',(-0.25896307723613,0.09253715269228,0.1425));
#41223=CARTESIAN_POINT('Ctrl Pts',(-0.252777314991409,0.0920034185546049,
0.291));
#41224=CARTESIAN_POINT('Ctrl Pts',(-0.255836083454369,0.0922673422366571,
0.288035430631101));
#41225=CARTESIAN_POINT('Ctrl Pts',(-0.25896307723613,0.09253715269228,0.285));
#41226=CARTESIAN_POINT('Origin',(-0.244219163867212,0.141,0.04));
#41227=CARTESIAN_POINT('',(-0.238959938274539,0.136099771858106,0.04));
#41228=CARTESIAN_POINT('',(-0.237345829015656,0.138895491103459,0.04));
#41229=CARTESIAN_POINT('Origin',(0.,0.,0.04));
#41230=CARTESIAN_POINT('',(-0.232960833618014,0.1345,0.04));
#41231=CARTESIAN_POINT('',(-0.25897749411641,0.141437822173509,0.04));
#41232=CARTESIAN_POINT('',(-0.232960833618014,0.1345,0.04));
#41233=CARTESIAN_POINT('Origin',(-0.232960833618014,0.1345,0.04));
#41234=CARTESIAN_POINT('',(-0.237345829015656,0.138895491103459,0.285));
#41235=CARTESIAN_POINT('',(-0.237345829015656,0.138895491103459,0.1425));
#41236=CARTESIAN_POINT('',(-0.232960833618014,0.1345,0.291));
#41237=CARTESIAN_POINT('',(-0.232960833618014,0.1345,0.04));
#41238=CARTESIAN_POINT('Ctrl Pts',(-0.237345829015656,0.138895491103459,
0.285));
#41239=CARTESIAN_POINT('Ctrl Pts',(-0.23512914935695,0.136673505711114,
0.288035430631098));
#41240=CARTESIAN_POINT('Ctrl Pts',(-0.232960833618014,0.1345,0.291));
#41241=CARTESIAN_POINT('Origin',(-0.25897749411641,0.141437822173509,0.04));
#41242=CARTESIAN_POINT('',(-0.238959938274539,0.136099771858106,0.285));
#41243=CARTESIAN_POINT('',(-0.238959938274539,0.136099771858106,0.1425));
#41244=CARTESIAN_POINT('Ctrl Pts',(-0.232960833618014,0.1345,0.291));
#41245=CARTESIAN_POINT('Ctrl Pts',(-0.235927302648541,0.135291063657777,
0.288035430631136));
#41246=CARTESIAN_POINT('Ctrl Pts',(-0.238959938274539,0.136099771858106,
0.285));
#41247=CARTESIAN_POINT('Origin',(-0.216024532959552,0.181266105931604,0.04));
#41248=CARTESIAN_POINT('',(-0.211696122508039,0.175527068325832,0.04));
#41249=CARTESIAN_POINT('',(-0.209621063643459,0.17800002718254,0.04));
#41250=CARTESIAN_POINT('Origin',(0.,0.,0.04));
#41251=CARTESIAN_POINT('',(-0.206065955199005,0.172909867005679,0.04));
#41252=CARTESIAN_POINT('',(-0.230482623987904,0.184260033755696,0.04));
#41253=CARTESIAN_POINT('',(-0.206065955199005,0.172909867005679,0.04));
#41254=CARTESIAN_POINT('Origin',(-0.206065955199005,0.172909867005679,0.04));
#41255=CARTESIAN_POINT('',(-0.209621063643459,0.17800002718254,0.285));
#41256=CARTESIAN_POINT('',(-0.209621063643459,0.17800002718254,0.1425));
#41257=CARTESIAN_POINT('',(-0.206065955199005,0.172909867005679,0.291));
#41258=CARTESIAN_POINT('',(-0.206065955199005,0.172909867005679,0.04));
#41259=CARTESIAN_POINT('Ctrl Pts',(-0.209621063643459,0.17800002718254,
0.285));
#41260=CARTESIAN_POINT('Ctrl Pts',(-0.207823904043728,0.175426876357765,
0.288035430631226));
#41261=CARTESIAN_POINT('Ctrl Pts',(-0.206065955199005,0.172909867005679,
0.291));
#41262=CARTESIAN_POINT('Origin',(-0.230482623987904,0.184260033755696,0.04));
#41263=CARTESIAN_POINT('',(-0.211696122508039,0.175527068325832,0.285));
#41264=CARTESIAN_POINT('',(-0.211696122508039,0.175527068325832,0.1425));
#41265=CARTESIAN_POINT('Ctrl Pts',(-0.206065955199005,0.172909867005679,
0.291));
#41266=CARTESIAN_POINT('Ctrl Pts',(-0.208849990136858,0.174204034570293,
0.288035430631017));
#41267=CARTESIAN_POINT('Ctrl Pts',(-0.211696122508039,0.175527068325832,
0.285));
#41268=CARTESIAN_POINT('Origin',(-0.181266105931604,0.216024532959552,0.04));
#41269=CARTESIAN_POINT('',(-0.17800002718254,0.209621063643459,0.04));
#41270=CARTESIAN_POINT('',(-0.175527068325832,0.211696122508039,0.04));
#41271=CARTESIAN_POINT('Origin',(0.,0.,0.04));
#41272=CARTESIAN_POINT('',(-0.172909867005679,0.206065955199005,0.04));
#41273=CARTESIAN_POINT('',(-0.194984655959362,0.221483597452293,0.04));
#41274=CARTESIAN_POINT('',(-0.172909867005679,0.206065955199005,0.04));
#41275=CARTESIAN_POINT('Origin',(-0.172909867005679,0.206065955199005,0.04));
#41276=CARTESIAN_POINT('',(-0.175527068325832,0.211696122508039,0.285));
#41277=CARTESIAN_POINT('',(-0.175527068325832,0.211696122508039,0.1425));
#41278=CARTESIAN_POINT('',(-0.172909867005679,0.206065955199005,0.291));
#41279=CARTESIAN_POINT('',(-0.172909867005679,0.206065955199005,0.04));
#41280=CARTESIAN_POINT('Ctrl Pts',(-0.175527068325832,0.211696122508039,
0.285));
#41281=CARTESIAN_POINT('Ctrl Pts',(-0.174204034570238,0.208849990136741,
0.288035430631142));
#41282=CARTESIAN_POINT('Ctrl Pts',(-0.172909867005679,0.206065955199005,
0.291));
#41283=CARTESIAN_POINT('Origin',(-0.194984655959362,0.221483597452293,0.04));
#41284=CARTESIAN_POINT('',(-0.17800002718254,0.209621063643459,0.285));
#41285=CARTESIAN_POINT('',(-0.17800002718254,0.209621063643459,0.1425));
#41286=CARTESIAN_POINT('Ctrl Pts',(-0.172909867005679,0.206065955199005,
0.291));
#41287=CARTESIAN_POINT('Ctrl Pts',(-0.175426876357856,0.207823904043792,
0.288035430631119));
#41288=CARTESIAN_POINT('Ctrl Pts',(-0.17800002718254,0.209621063643459,
0.285));
#41289=CARTESIAN_POINT('Origin',(-0.141,0.244219163867212,0.04));
#41290=CARTESIAN_POINT('',(-0.138895491103459,0.237345829015656,0.04));
#41291=CARTESIAN_POINT('',(-0.136099771858106,0.238959938274539,0.04));
#41292=CARTESIAN_POINT('Origin',(0.,0.,0.04));
#41293=CARTESIAN_POINT('',(-0.1345,0.232960833618014,0.04));
#41294=CARTESIAN_POINT('',(-0.153562177826491,0.25197749411641,0.04));
#41295=CARTESIAN_POINT('',(-0.1345,0.232960833618014,0.04));
#41296=CARTESIAN_POINT('Origin',(-0.1345,0.232960833618014,0.04));
#41297=CARTESIAN_POINT('',(-0.136099771858106,0.238959938274539,0.285));
#41298=CARTESIAN_POINT('',(-0.136099771858106,0.238959938274539,0.1425));
#41299=CARTESIAN_POINT('',(-0.1345,0.232960833618014,0.291));
#41300=CARTESIAN_POINT('',(-0.1345,0.232960833618014,0.04));
#41301=CARTESIAN_POINT('Ctrl Pts',(-0.136099771858106,0.238959938274539,
0.285));
#41302=CARTESIAN_POINT('Ctrl Pts',(-0.135291063657772,0.235927302648521,
0.288035430631155));
#41303=CARTESIAN_POINT('Ctrl Pts',(-0.1345,0.232960833618014,0.291));
#41304=CARTESIAN_POINT('Origin',(-0.153562177826491,0.25197749411641,0.04));
#41305=CARTESIAN_POINT('',(-0.138895491103459,0.237345829015656,0.285));
#41306=CARTESIAN_POINT('',(-0.138895491103459,0.237345829015656,0.1425));
#41307=CARTESIAN_POINT('Ctrl Pts',(-0.1345,0.232960833618014,0.291));
#41308=CARTESIAN_POINT('Ctrl Pts',(-0.13667350571114,0.235129149356976,
0.288035430631063));
#41309=CARTESIAN_POINT('Ctrl Pts',(-0.138895491103459,0.237345829015656,
0.285));
#41310=CARTESIAN_POINT('Origin',(-0.0964496804178386,0.264993319061626,
0.04));
#41311=CARTESIAN_POINT('',(-0.095570685811709,0.257858961475997,0.04));
#41312=CARTESIAN_POINT('',(-0.09253715269228,0.25896307723613,0.04));
#41313=CARTESIAN_POINT('Origin',(0.,0.,0.04));
#41314=CARTESIAN_POINT('',(-0.0920034185546049,0.252777314991409,0.04));
#41315=CARTESIAN_POINT('',(-0.107473790626574,0.274815182128563,0.04));
#41316=CARTESIAN_POINT('',(-0.0920034185546049,0.252777314991409,0.04));
#41317=CARTESIAN_POINT('Origin',(-0.0920034185546049,0.252777314991409,
0.04));
#41318=CARTESIAN_POINT('',(-0.09253715269228,0.25896307723613,0.285));
#41319=CARTESIAN_POINT('',(-0.09253715269228,0.25896307723613,0.1425));
#41320=CARTESIAN_POINT('',(-0.0920034185546049,0.252777314991409,0.291));
#41321=CARTESIAN_POINT('',(-0.0920034185546049,0.252777314991409,0.04));
#41322=CARTESIAN_POINT('Ctrl Pts',(-0.09253715269228,0.25896307723613,0.285));
#41323=CARTESIAN_POINT('Ctrl Pts',(-0.0922673422366543,0.255836083454338,
0.288035430631132));
#41324=CARTESIAN_POINT('Ctrl Pts',(-0.0920034185546049,0.252777314991409,
0.291));
#41325=CARTESIAN_POINT('Origin',(-0.107473790626574,0.274815182128563,0.04));
#41326=CARTESIAN_POINT('',(-0.095570685811709,0.257858961475997,0.285));
#41327=CARTESIAN_POINT('',(-0.095570685811709,0.257858961475997,0.1425));
#41328=CARTESIAN_POINT('Ctrl Pts',(-0.0920034185546049,0.252777314991409,
0.291));
#41329=CARTESIAN_POINT('Ctrl Pts',(-0.0937673797534821,0.255290114448016,
0.288035430631051));
#41330=CARTESIAN_POINT('Ctrl Pts',(-0.0955706858117089,0.257858961475997,
0.285));
#41331=CARTESIAN_POINT('Origin',(-0.0489687861020744,0.277715786349443,
0.04));
#41332=CARTESIAN_POINT('',(-0.0493420135926708,0.27053717987482,0.04));
#41333=CARTESIAN_POINT('',(-0.0461628389679574,0.271097754137541,0.04));
#41334=CARTESIAN_POINT('Origin',(0.,0.,0.04));
#41335=CARTESIAN_POINT('',(-0.0467113597924043,0.264913285560284,0.04));
#41336=CARTESIAN_POINT('',(-0.0581198666828299,0.289302749894933,0.04));
#41337=CARTESIAN_POINT('',(-0.0467113597924043,0.264913285560284,0.04));
#41338=CARTESIAN_POINT('Origin',(-0.0467113597924043,0.264913285560284,
0.04));
#41339=CARTESIAN_POINT('',(-0.0461628389679574,0.271097754137541,0.285));
#41340=CARTESIAN_POINT('',(-0.0461628389679574,0.271097754137541,0.1425));
#41341=CARTESIAN_POINT('',(-0.0467113597924043,0.264913285560284,0.291));
#41342=CARTESIAN_POINT('',(-0.0467113597924043,0.264913285560284,0.04));
#41343=CARTESIAN_POINT('Ctrl Pts',(-0.0461628389679575,0.271097754137541,
0.285));
#41344=CARTESIAN_POINT('Ctrl Pts',(-0.0464401243112017,0.267971414323629,
0.288035430631178));
#41345=CARTESIAN_POINT('Ctrl Pts',(-0.0467113597924043,0.264913285560284,
0.291));
#41346=CARTESIAN_POINT('Origin',(-0.0581198666828299,0.289302749894933,
0.04));
#41347=CARTESIAN_POINT('',(-0.0493420135926708,0.27053717987482,0.285));
#41348=CARTESIAN_POINT('',(-0.0493420135926708,0.27053717987482,0.1425));
#41349=CARTESIAN_POINT('Ctrl Pts',(-0.0467113597924043,0.264913285560284,
0.291));
#41350=CARTESIAN_POINT('Ctrl Pts',(-0.0480121794105643,0.267694218594523,
0.288035430631107));
#41351=CARTESIAN_POINT('Ctrl Pts',(-0.0493420135926707,0.27053717987482,
0.285));
#41352=CARTESIAN_POINT('Origin',(1.38777878078145E-17,0.282,0.04));
#41353=CARTESIAN_POINT('',(-0.0016141092588829,0.274995262961565,0.04));
#41354=CARTESIAN_POINT('',(0.00161410925888293,0.274995262961565,0.04));
#41355=CARTESIAN_POINT('Origin',(0.,0.,0.04));
#41356=CARTESIAN_POINT('',(2.08166817117217E-17,0.269,0.04));
#41357=CARTESIAN_POINT('',(-0.00699999999999999,0.295,0.04));
#41358=CARTESIAN_POINT('',(2.08166817117217E-17,0.269,0.04));
#41359=CARTESIAN_POINT('Origin',(2.08166817117217E-17,0.269,0.04));
#41360=CARTESIAN_POINT('',(0.00161410925888295,0.274995262961565,0.285));
#41361=CARTESIAN_POINT('',(0.00161410925888295,0.274995262961565,0.1425));
#41362=CARTESIAN_POINT('',(2.08166817117217E-17,0.269,0.291));
#41363=CARTESIAN_POINT('',(2.08166817117217E-17,0.269,0.04));
#41364=CARTESIAN_POINT('Ctrl Pts',(0.00161410925888293,0.274995262961565,
0.285));
#41365=CARTESIAN_POINT('Ctrl Pts',(0.000798153291618306,0.271964569368868,
0.288035430631132));
#41366=CARTESIAN_POINT('Ctrl Pts',(2.08166817117217E-17,0.269,0.291));
#41367=CARTESIAN_POINT('Origin',(-0.00699999999999999,0.295,0.04));
#41368=CARTESIAN_POINT('',(-0.00161410925888292,0.274995262961565,0.285));
#41369=CARTESIAN_POINT('',(-0.00161410925888292,0.274995262961565,0.1425));
#41370=CARTESIAN_POINT('Ctrl Pts',(2.08166817117217E-17,0.269,0.291));
#41371=CARTESIAN_POINT('Ctrl Pts',(-0.000798153291634971,0.27196456936893,
0.28803543063107));
#41372=CARTESIAN_POINT('Ctrl Pts',(-0.00161410925888289,0.274995262961565,
0.285));
#41373=CARTESIAN_POINT('Origin',(0.0489687861020744,0.277715786349443,0.04));
#41374=CARTESIAN_POINT('',(0.0461628389679574,0.271097754137541,0.04));
#41375=CARTESIAN_POINT('',(0.0493420135926708,0.27053717987482,0.04));
#41376=CARTESIAN_POINT('Origin',(0.,0.,0.04));
#41377=CARTESIAN_POINT('',(0.0467113597924043,0.264913285560284,0.04));
#41378=CARTESIAN_POINT('',(0.044332558140659,0.29173382438227,0.04));
#41379=CARTESIAN_POINT('',(0.0467113597924043,0.264913285560284,0.04));
#41380=CARTESIAN_POINT('Origin',(0.0467113597924043,0.264913285560284,0.04));
#41381=CARTESIAN_POINT('',(0.0493420135926708,0.27053717987482,0.285));
#41382=CARTESIAN_POINT('',(0.0493420135926708,0.27053717987482,0.1425));
#41383=CARTESIAN_POINT('',(0.0467113597924043,0.264913285560284,0.291));
#41384=CARTESIAN_POINT('',(0.0467113597924043,0.264913285560284,0.04));
#41385=CARTESIAN_POINT('Ctrl Pts',(0.0493420135926708,0.27053717987482,
0.285));
#41386=CARTESIAN_POINT('Ctrl Pts',(0.048012179410518,0.267694218594424,
0.288035430631212));
#41387=CARTESIAN_POINT('Ctrl Pts',(0.0467113597924043,0.264913285560284,
0.291));
#41388=CARTESIAN_POINT('Origin',(0.044332558140659,0.29173382438227,0.04));
#41389=CARTESIAN_POINT('',(0.0461628389679575,0.271097754137541,0.285));
#41390=CARTESIAN_POINT('',(0.0461628389679575,0.271097754137541,0.1425));
#41391=CARTESIAN_POINT('Ctrl Pts',(0.0467113597924043,0.264913285560284,
0.291));
#41392=CARTESIAN_POINT('Ctrl Pts',(0.0464401243111968,0.267971414323684,
0.288035430631124));
#41393=CARTESIAN_POINT('Ctrl Pts',(0.0461628389679575,0.271097754137541,
0.285));
#41394=CARTESIAN_POINT('Origin',(0.0964496804178386,0.264993319061626,0.04));
#41395=CARTESIAN_POINT('',(0.09253715269228,0.25896307723613,0.04));
#41396=CARTESIAN_POINT('',(0.095570685811709,0.257858961475997,0.04));
#41397=CARTESIAN_POINT('Origin',(0.,0.,0.04));
#41398=CARTESIAN_POINT('',(0.0920034185546049,0.252777314991409,0.04));
#41399=CARTESIAN_POINT('',(0.094318093935571,0.279603464135123,0.04));
#41400=CARTESIAN_POINT('',(0.0920034185546049,0.252777314991409,0.04));
#41401=CARTESIAN_POINT('Origin',(0.0920034185546049,0.252777314991409,0.04));
#41402=CARTESIAN_POINT('',(0.095570685811709,0.257858961475997,0.285));
#41403=CARTESIAN_POINT('',(0.095570685811709,0.257858961475997,0.1425));
#41404=CARTESIAN_POINT('',(0.0920034185546049,0.252777314991409,0.291));
#41405=CARTESIAN_POINT('',(0.0920034185546049,0.252777314991409,0.04));
#41406=CARTESIAN_POINT('Ctrl Pts',(0.095570685811709,0.257858961475997,
0.285));
#41407=CARTESIAN_POINT('Ctrl Pts',(0.0937673797534397,0.255290114447956,
0.288035430631122));
#41408=CARTESIAN_POINT('Ctrl Pts',(0.0920034185546049,0.252777314991409,
0.291));
#41409=CARTESIAN_POINT('Origin',(0.094318093935571,0.279603464135123,0.04));
#41410=CARTESIAN_POINT('',(0.09253715269228,0.25896307723613,0.285));
#41411=CARTESIAN_POINT('',(0.09253715269228,0.25896307723613,0.1425));
#41412=CARTESIAN_POINT('Ctrl Pts',(0.0920034185546049,0.252777314991409,
0.291));
#41413=CARTESIAN_POINT('Ctrl Pts',(0.0922673422366571,0.255836083454369,
0.288035430631101));
#41414=CARTESIAN_POINT('Ctrl Pts',(0.09253715269228,0.25896307723613,0.285));
#41415=CARTESIAN_POINT('Origin',(0.141,0.244219163867212,0.04));
#41416=CARTESIAN_POINT('',(0.136099771858106,0.238959938274539,0.04));
#41417=CARTESIAN_POINT('',(0.138895491103459,0.237345829015656,0.04));
#41418=CARTESIAN_POINT('Origin',(0.,0.,0.04));
#41419=CARTESIAN_POINT('',(0.1345,0.232960833618014,0.04));
#41420=CARTESIAN_POINT('',(0.141437822173509,0.258977494116409,0.04));
#41421=CARTESIAN_POINT('',(0.1345,0.232960833618014,0.04));
#41422=CARTESIAN_POINT('Origin',(0.1345,0.232960833618014,0.04));
#41423=CARTESIAN_POINT('',(0.138895491103459,0.237345829015656,0.285));
#41424=CARTESIAN_POINT('',(0.138895491103459,0.237345829015656,0.1425));
#41425=CARTESIAN_POINT('',(0.1345,0.232960833618014,0.291));
#41426=CARTESIAN_POINT('',(0.1345,0.232960833618014,0.04));
#41427=CARTESIAN_POINT('Ctrl Pts',(0.138895491103459,0.237345829015656,
0.285));
#41428=CARTESIAN_POINT('Ctrl Pts',(0.136673505711127,0.235129149356963,
0.288035430631081));
#41429=CARTESIAN_POINT('Ctrl Pts',(0.1345,0.232960833618014,0.291));
#41430=CARTESIAN_POINT('Origin',(0.141437822173509,0.258977494116409,0.04));
#41431=CARTESIAN_POINT('',(0.136099771858106,0.238959938274539,0.285));
#41432=CARTESIAN_POINT('',(0.136099771858106,0.238959938274539,0.1425));
#41433=CARTESIAN_POINT('Ctrl Pts',(0.1345,0.232960833618014,0.291));
#41434=CARTESIAN_POINT('Ctrl Pts',(0.1352910636578,0.235927302648627,0.28803543063105));
#41435=CARTESIAN_POINT('Ctrl Pts',(0.136099771858106,0.238959938274539,
0.285));
#41436=CARTESIAN_POINT('Origin',(0.181266105931604,0.216024532959552,0.04));
#41437=CARTESIAN_POINT('',(0.175527068325832,0.211696122508039,0.04));
#41438=CARTESIAN_POINT('',(0.17800002718254,0.209621063643459,0.04));
#41439=CARTESIAN_POINT('Origin',(0.,0.,0.04));
#41440=CARTESIAN_POINT('',(0.172909867005679,0.206065955199005,0.04));
#41441=CARTESIAN_POINT('',(0.184260033755696,0.230482623987904,0.04));
#41442=CARTESIAN_POINT('',(0.172909867005679,0.206065955199005,0.04));
#41443=CARTESIAN_POINT('Origin',(0.172909867005679,0.206065955199005,0.04));
#41444=CARTESIAN_POINT('',(0.17800002718254,0.209621063643459,0.285));
#41445=CARTESIAN_POINT('',(0.17800002718254,0.209621063643459,0.1425));
#41446=CARTESIAN_POINT('',(0.172909867005679,0.206065955199005,0.291));
#41447=CARTESIAN_POINT('',(0.172909867005679,0.206065955199005,0.04));
#41448=CARTESIAN_POINT('Ctrl Pts',(0.17800002718254,0.209621063643459,0.285));
#41449=CARTESIAN_POINT('Ctrl Pts',(0.175426876357847,0.207823904043786,
0.28803543063113));
#41450=CARTESIAN_POINT('Ctrl Pts',(0.172909867005679,0.206065955199005,
0.291));
#41451=CARTESIAN_POINT('Origin',(0.184260033755696,0.230482623987904,0.04));
#41452=CARTESIAN_POINT('',(0.175527068325832,0.211696122508039,0.285));
#41453=CARTESIAN_POINT('',(0.175527068325832,0.211696122508039,0.1425));
#41454=CARTESIAN_POINT('Ctrl Pts',(0.172909867005679,0.206065955199005,
0.291));
#41455=CARTESIAN_POINT('Ctrl Pts',(0.174204034570257,0.208849990136781,
0.288035430631099));
#41456=CARTESIAN_POINT('Ctrl Pts',(0.175527068325832,0.211696122508039,
0.285));
#41457=CARTESIAN_POINT('Origin',(0.216024532959552,0.181266105931604,0.04));
#41458=CARTESIAN_POINT('',(0.209621063643459,0.17800002718254,0.04));
#41459=CARTESIAN_POINT('',(0.211696122508039,0.175527068325832,0.04));
#41460=CARTESIAN_POINT('Origin',(0.,0.,0.04));
#41461=CARTESIAN_POINT('',(0.206065955199005,0.172909867005679,0.04));
#41462=CARTESIAN_POINT('',(0.221483597452293,0.194984655959362,0.04));
#41463=CARTESIAN_POINT('',(0.206065955199005,0.172909867005679,0.04));
#41464=CARTESIAN_POINT('Origin',(0.206065955199005,0.172909867005679,0.04));
#41465=CARTESIAN_POINT('',(0.211696122508039,0.175527068325832,0.285));
#41466=CARTESIAN_POINT('',(0.211696122508039,0.175527068325832,0.1425));
#41467=CARTESIAN_POINT('',(0.206065955199005,0.172909867005679,0.291));
#41468=CARTESIAN_POINT('',(0.206065955199005,0.172909867005679,0.04));
#41469=CARTESIAN_POINT('Ctrl Pts',(0.211696122508039,0.175527068325832,
0.285));
#41470=CARTESIAN_POINT('Ctrl Pts',(0.208849990136656,0.174204034570199,
0.288035430631232));
#41471=CARTESIAN_POINT('Ctrl Pts',(0.206065955199005,0.172909867005679,
0.291));
#41472=CARTESIAN_POINT('Origin',(0.221483597452293,0.194984655959362,0.04));
#41473=CARTESIAN_POINT('',(0.209621063643459,0.17800002718254,0.285));
#41474=CARTESIAN_POINT('',(0.209621063643459,0.17800002718254,0.1425));
#41475=CARTESIAN_POINT('Ctrl Pts',(0.206065955199005,0.172909867005679,
0.291));
#41476=CARTESIAN_POINT('Ctrl Pts',(0.207823904043843,0.175426876357928,
0.288035430631034));
#41477=CARTESIAN_POINT('Ctrl Pts',(0.209621063643459,0.17800002718254,0.285));
#41478=CARTESIAN_POINT('Origin',(0.244219163867212,0.141,0.04));
#41479=CARTESIAN_POINT('',(0.237345829015656,0.138895491103459,0.04));
#41480=CARTESIAN_POINT('',(0.238959938274539,0.136099771858106,0.04));
#41481=CARTESIAN_POINT('Origin',(0.,0.,0.04));
#41482=CARTESIAN_POINT('',(0.232960833618014,0.1345,0.04));
#41483=CARTESIAN_POINT('',(0.25197749411641,0.153562177826491,0.04));
#41484=CARTESIAN_POINT('',(0.232960833618014,0.1345,0.04));
#41485=CARTESIAN_POINT('Origin',(0.232960833618014,0.1345,0.04));
#41486=CARTESIAN_POINT('',(0.238959938274539,0.136099771858106,0.285));
#41487=CARTESIAN_POINT('',(0.238959938274539,0.136099771858106,0.1425));
#41488=CARTESIAN_POINT('',(0.232960833618014,0.1345,0.291));
#41489=CARTESIAN_POINT('',(0.232960833618014,0.1345,0.04));
#41490=CARTESIAN_POINT('Ctrl Pts',(0.238959938274539,0.136099771858106,
0.285));
#41491=CARTESIAN_POINT('Ctrl Pts',(0.235927302648562,0.135291063657783,
0.288035430631114));
#41492=CARTESIAN_POINT('Ctrl Pts',(0.232960833618014,0.1345,0.291));
#41493=CARTESIAN_POINT('Origin',(0.25197749411641,0.153562177826491,0.04));
#41494=CARTESIAN_POINT('',(0.237345829015656,0.138895491103459,0.285));
#41495=CARTESIAN_POINT('',(0.237345829015656,0.138895491103459,0.1425));
#41496=CARTESIAN_POINT('Ctrl Pts',(0.232960833618014,0.1345,0.291));
#41497=CARTESIAN_POINT('Ctrl Pts',(0.235129149356992,0.136673505711156,
0.288035430631041));
#41498=CARTESIAN_POINT('Ctrl Pts',(0.237345829015656,0.138895491103459,
0.285));
#41499=CARTESIAN_POINT('Origin',(0.264993319061626,0.0964496804178386,0.04));
#41500=CARTESIAN_POINT('',(0.257858961475997,0.095570685811709,0.04));
#41501=CARTESIAN_POINT('',(0.25896307723613,0.09253715269228,0.04));
#41502=CARTESIAN_POINT('Origin',(0.,0.,0.04));
#41503=CARTESIAN_POINT('',(0.252777314991409,0.0920034185546049,0.04));
#41504=CARTESIAN_POINT('',(0.274815182128563,0.107473790626574,0.04));
#41505=CARTESIAN_POINT('',(0.252777314991409,0.0920034185546049,0.04));
#41506=CARTESIAN_POINT('Origin',(0.252777314991409,0.0920034185546049,0.04));
#41507=CARTESIAN_POINT('',(0.25896307723613,0.09253715269228,0.285));
#41508=CARTESIAN_POINT('',(0.25896307723613,0.09253715269228,0.1425));
#41509=CARTESIAN_POINT('',(0.252777314991409,0.0920034185546049,0.291));
#41510=CARTESIAN_POINT('',(0.252777314991409,0.0920034185546049,0.04));
#41511=CARTESIAN_POINT('Ctrl Pts',(0.25896307723613,0.09253715269228,0.285));
#41512=CARTESIAN_POINT('Ctrl Pts',(0.255836083454338,0.0922673422366543,
0.288035430631132));
#41513=CARTESIAN_POINT('Ctrl Pts',(0.252777314991409,0.0920034185546049,
0.291));
#41514=CARTESIAN_POINT('Origin',(0.274815182128563,0.107473790626574,0.04));
#41515=CARTESIAN_POINT('',(0.257858961475997,0.095570685811709,0.285));
#41516=CARTESIAN_POINT('',(0.257858961475997,0.095570685811709,0.1425));
#41517=CARTESIAN_POINT('Ctrl Pts',(0.252777314991409,0.0920034185546049,
0.291));
#41518=CARTESIAN_POINT('Ctrl Pts',(0.255290114448016,0.0937673797534821,
0.288035430631051));
#41519=CARTESIAN_POINT('Ctrl Pts',(0.257858961475997,0.0955706858117089,
0.285));
#41520=CARTESIAN_POINT('Origin',(0.277715786349443,0.0489687861020744,0.04));
#41521=CARTESIAN_POINT('',(0.27053717987482,0.0493420135926708,0.04));
#41522=CARTESIAN_POINT('',(0.271097754137541,0.0461628389679574,0.04));
#41523=CARTESIAN_POINT('Origin',(0.,0.,0.04));
#41524=CARTESIAN_POINT('',(0.264913285560284,0.0467113597924043,0.04));
#41525=CARTESIAN_POINT('',(0.289302749894933,0.0581198666828299,0.04));
#41526=CARTESIAN_POINT('',(0.264913285560284,0.0467113597924043,0.04));
#41527=CARTESIAN_POINT('Origin',(0.264913285560284,0.0467113597924043,0.04));
#41528=CARTESIAN_POINT('',(0.271097754137541,0.0461628389679574,0.285));
#41529=CARTESIAN_POINT('',(0.271097754137541,0.0461628389679574,0.1425));
#41530=CARTESIAN_POINT('',(0.264913285560284,0.0467113597924043,0.291));
#41531=CARTESIAN_POINT('',(0.264913285560284,0.0467113597924043,0.04));
#41532=CARTESIAN_POINT('Ctrl Pts',(0.271097754137541,0.0461628389679574,
0.285));
#41533=CARTESIAN_POINT('Ctrl Pts',(0.267971414323704,0.0464401243111951,
0.288035430631105));
#41534=CARTESIAN_POINT('Ctrl Pts',(0.264913285560284,0.0467113597924043,
0.291));
#41535=CARTESIAN_POINT('Origin',(0.289302749894933,0.0581198666828299,0.04));
#41536=CARTESIAN_POINT('',(0.27053717987482,0.0493420135926708,0.285));
#41537=CARTESIAN_POINT('',(0.27053717987482,0.0493420135926708,0.1425));
#41538=CARTESIAN_POINT('Ctrl Pts',(0.264913285560284,0.0467113597924043,
0.291));
#41539=CARTESIAN_POINT('Ctrl Pts',(0.26769421859449,0.0480121794105489,
0.288035430631142));
#41540=CARTESIAN_POINT('Ctrl Pts',(0.27053717987482,0.0493420135926708,
0.285));
#41541=CARTESIAN_POINT('Origin',(0.,0.,0.1425));
#41542=CARTESIAN_POINT('Origin',(0.,0.,0.285));
#41543=CARTESIAN_POINT('Origin',(0.,0.,0.285));
#41544=CARTESIAN_POINT('Origin',(0.,0.,0.285));
#41545=CARTESIAN_POINT('Origin',(0.,0.,0.285));
#41546=CARTESIAN_POINT('Origin',(0.,0.,0.285));
#41547=CARTESIAN_POINT('Origin',(0.,0.,0.285));
#41548=CARTESIAN_POINT('Origin',(0.,0.,0.285));
#41549=CARTESIAN_POINT('Origin',(0.,0.,0.285));
#41550=CARTESIAN_POINT('Origin',(0.,0.,0.285));
#41551=CARTESIAN_POINT('Origin',(0.,0.,0.285));
#41552=CARTESIAN_POINT('Origin',(0.,0.,0.285));
#41553=CARTESIAN_POINT('Origin',(0.,0.,0.285));
#41554=CARTESIAN_POINT('Origin',(0.,0.,0.285));
#41555=CARTESIAN_POINT('Origin',(0.,0.,0.285));
#41556=CARTESIAN_POINT('Origin',(0.,0.,0.285));
#41557=CARTESIAN_POINT('Origin',(0.,0.,0.285));
#41558=CARTESIAN_POINT('Origin',(0.,0.,0.285));
#41559=CARTESIAN_POINT('',(-0.275,-3.36777869765522E-17,0.));
#41560=CARTESIAN_POINT('',(-0.275,-3.36777869765522E-17,0.1425));
#41561=CARTESIAN_POINT('Origin',(0.,0.,0.));
#41562=CARTESIAN_POINT('Origin',(0.,0.,0.285));
#41563=CARTESIAN_POINT('Origin',(0.,0.,0.285));
#41564=CARTESIAN_POINT('Origin',(0.,0.,0.285));
#41565=CARTESIAN_POINT('Origin',(0.,0.,0.285));
#41566=CARTESIAN_POINT('Origin',(0.,0.,0.285));
#41567=CARTESIAN_POINT('Origin',(0.,0.,0.285));
#41568=CARTESIAN_POINT('Origin',(0.,0.,0.285));
#41569=CARTESIAN_POINT('Origin',(0.,0.,0.285));
#41570=CARTESIAN_POINT('Origin',(0.,0.,0.285));
#41571=CARTESIAN_POINT('Origin',(0.,0.,0.285));
#41572=CARTESIAN_POINT('Origin',(0.,0.,0.285));
#41573=CARTESIAN_POINT('Origin',(0.,0.,0.285));
#41574=CARTESIAN_POINT('Origin',(0.,0.,0.285));
#41575=CARTESIAN_POINT('Origin',(0.,0.,0.285));
#41576=CARTESIAN_POINT('Origin',(0.,0.,0.285));
#41577=CARTESIAN_POINT('Origin',(0.,0.,0.285));
#41578=CARTESIAN_POINT('Origin',(0.,0.,0.285));
#41579=CARTESIAN_POINT('',(0.274995262961565,0.00161410925888293,0.285));
#41580=CARTESIAN_POINT('Origin',(0.,0.,0.285));
#41581=CARTESIAN_POINT('',(0.274995262961565,0.00161410925888293,0.04));
#41582=CARTESIAN_POINT('',(0.274995262961565,0.00161410925888293,0.1425));
#41583=CARTESIAN_POINT('',(0.274995262961565,-0.00161410925888293,0.04));
#41584=CARTESIAN_POINT('Origin',(0.,0.,0.04));
#41585=CARTESIAN_POINT('',(0.274995262961565,-0.00161410925888293,0.285));
#41586=CARTESIAN_POINT('',(0.274995262961565,-0.00161410925888293,0.1425));
#41587=CARTESIAN_POINT('Origin',(0.,0.,0.285));
#41588=CARTESIAN_POINT('Origin',(0.269,0.,0.04));
#41589=CARTESIAN_POINT('',(0.269,0.,0.04));
#41590=CARTESIAN_POINT('',(0.269,0.,0.04));
#41591=CARTESIAN_POINT('',(0.269,0.,0.291));
#41592=CARTESIAN_POINT('',(0.269,0.,0.04));
#41593=CARTESIAN_POINT('Ctrl Pts',(0.274995262961565,-0.00161410925888293,
0.285));
#41594=CARTESIAN_POINT('Ctrl Pts',(0.271964569368838,-0.000798153291610108,
0.288035430631162));
#41595=CARTESIAN_POINT('Ctrl Pts',(0.269,0.,0.291));
#41596=CARTESIAN_POINT('Origin',(0.295,0.007,0.04));
#41597=CARTESIAN_POINT('Ctrl Pts',(0.269,0.,0.291));
#41598=CARTESIAN_POINT('Ctrl Pts',(0.27196456936891,0.000798153291629561,
0.28803543063109));
#41599=CARTESIAN_POINT('Ctrl Pts',(0.274995262961565,0.00161410925888293,
0.285));
#41600=CARTESIAN_POINT('',(0.295,0.007,0.04));
#41601=CARTESIAN_POINT('Origin',(0.282,0.,0.04));
#41602=CARTESIAN_POINT('Origin',(0.,0.,0.2925));
#41603=CARTESIAN_POINT('',(-0.26,-3.18408167778312E-17,0.3));
#41604=CARTESIAN_POINT('Origin',(0.,0.,0.3));
#41605=CARTESIAN_POINT('',(-0.2675,-3.27593018771917E-17,0.2925));
#41606=CARTESIAN_POINT('Origin',(0.,0.,0.134415608175648));
#41607=CARTESIAN_POINT('',(0.,0.,0.0978312163512968));
#41608=CARTESIAN_POINT('',(-0.113891921086774,1.39477376607661E-17,0.17));
#41609=CARTESIAN_POINT('',(-0.0577350269189626,-7.07050159149938E-18,0.134415608175648));
#41610=CARTESIAN_POINT('Origin',(0.,0.,0.17));
#41611=CARTESIAN_POINT('Origin',(0.,0.144337567297406,0.3));
#41612=CARTESIAN_POINT('',(8.83812698937423E-18,0.144337567297406,0.3));
#41613=CARTESIAN_POINT('',(0.125,0.0721687836487032,0.3));
#41614=CARTESIAN_POINT('',(0.03125,0.126295371385231,0.3));
#41615=CARTESIAN_POINT('',(1.38777878078145E-17,0.144337567297406,0.17));
#41616=CARTESIAN_POINT('',(8.83812698937423E-18,0.144337567297406,0.3));
#41617=CARTESIAN_POINT('',(0.125,0.0721687836487032,0.17));
#41618=CARTESIAN_POINT('',(0.125,0.0721687836487032,0.17));
#41619=CARTESIAN_POINT('',(0.125,0.0721687836487032,0.3));
#41620=CARTESIAN_POINT('Origin',(-0.125,0.0721687836487032,0.3));
#41621=CARTESIAN_POINT('',(-0.125,0.0721687836487032,0.3));
#41622=CARTESIAN_POINT('',(-0.09375,0.090210979560879,0.3));
#41623=CARTESIAN_POINT('',(-0.125,0.0721687836487032,0.17));
#41624=CARTESIAN_POINT('',(-0.125,0.0721687836487032,0.3));
#41625=CARTESIAN_POINT('',(8.83812698937423E-18,0.144337567297406,0.17));
#41626=CARTESIAN_POINT('Origin',(-0.125,-0.0721687836487032,0.3));
#41627=CARTESIAN_POINT('',(-0.125,-0.0721687836487032,0.3));
#41628=CARTESIAN_POINT('',(-0.125,-0.0360843918243516,0.3));
#41629=CARTESIAN_POINT('',(-0.125,-0.0721687836487032,0.17));
#41630=CARTESIAN_POINT('',(-0.125,-0.0721687836487032,0.3));
#41631=CARTESIAN_POINT('',(-0.125,0.0721687836487032,0.17));
#41632=CARTESIAN_POINT('Origin',(-2.77555756156289E-17,-0.144337567297406,
0.3));
#41633=CARTESIAN_POINT('',(-2.65143809681227E-17,-0.144337567297406,0.3));
#41634=CARTESIAN_POINT('',(-0.03125,-0.126295371385231,0.3));
#41635=CARTESIAN_POINT('',(-2.77555756156289E-17,-0.144337567297406,0.17));
#41636=CARTESIAN_POINT('',(-2.65143809681227E-17,-0.144337567297406,0.3));
#41637=CARTESIAN_POINT('',(-0.125,-0.0721687836487032,0.17));
#41638=CARTESIAN_POINT('Origin',(0.125,-0.0721687836487033,0.3));
#41639=CARTESIAN_POINT('',(0.125,-0.0721687836487033,0.3));
#41640=CARTESIAN_POINT('',(0.09375,-0.0902109795608791,0.3));
#41641=CARTESIAN_POINT('',(0.125,-0.0721687836487033,0.17));
#41642=CARTESIAN_POINT('',(0.125,-0.0721687836487033,0.3));
#41643=CARTESIAN_POINT('',(-2.65143809681227E-17,-0.144337567297406,0.17));
#41644=CARTESIAN_POINT('Origin',(0.125,0.0721687836487032,0.3));
#41645=CARTESIAN_POINT('',(0.125,0.0360843918243516,0.3));
#41646=CARTESIAN_POINT('',(0.125,-0.0721687836487033,0.17));
#41647=CARTESIAN_POINT('Origin',(0.,0.,0.17));
#41648=CARTESIAN_POINT('Origin',(0.114,0.,-0.8));
#41649=CARTESIAN_POINT('',(-0.114,-1.39609735102798E-17,-0.8));
#41650=CARTESIAN_POINT('Origin',(0.,0.,-0.8));
#41651=CARTESIAN_POINT('Origin',(0.,0.,-0.782));
#41652=CARTESIAN_POINT('',(-0.132,-1.61653377487451E-17,-0.782));
#41653=CARTESIAN_POINT('Origin',(0.,0.,-0.387));
#41654=CARTESIAN_POINT('Origin',(0.,0.,-0.01365));
#41655=CARTESIAN_POINT('Origin',(0.,0.,-0.005));
#41656=CARTESIAN_POINT('',(-0.16,-1.95943487863577E-17,-2.60208521396521E-18));
#41657=CARTESIAN_POINT('Origin',(0.,0.,0.));
#41658=CARTESIAN_POINT('',(-0.155,-1.8982025386784E-17,-0.005));
#41659=CARTESIAN_POINT('Origin',(0.275,0.,0.));
#41660=CARTESIAN_POINT('Origin',(0.,0.,0.3));
#41661=CARTESIAN_POINT('',(0.,0.,0.));
#41662=CARTESIAN_POINT('Origin',(0.,0.,-1.487));
#41663=CARTESIAN_POINT('',(-0.146158606821014,-8.60648302992845E-5,-2.90158449541571));
#41664=CARTESIAN_POINT('',(-0.146182739311418,-0.000106450303776882,-2.90871550458429));
#41665=CARTESIAN_POINT('',(-0.14635,-1.79227059055215E-17,-1.487));
#41666=CARTESIAN_POINT('',(0.0262268935511073,-0.144224038131951,-2.93765));
#41667=CARTESIAN_POINT('Ctrl Pts',(-0.146158606821014,-8.60648302992845E-5,
-2.90158449541571));
#41668=CARTESIAN_POINT('Ctrl Pts',(-0.145999351227507,0.0299154702969904,
-2.90321100897527));
#41669=CARTESIAN_POINT('Ctrl Pts',(-0.137018833441673,0.0600042754394542,
-2.90483752253483));
#41670=CARTESIAN_POINT('Ctrl Pts',(-0.119884214267969,0.0843568428068597,
-2.90646403609438));
#41671=CARTESIAN_POINT('Ctrl Pts',(-0.0919771182949038,0.124019786454636,
-2.90911313319704));
#41672=CARTESIAN_POINT('Ctrl Pts',(-0.0424400239805762,0.148466483988013,
-2.91176223029968));
#41673=CARTESIAN_POINT('Ctrl Pts',(0.00601684655231771,0.146471621494668,
-2.91441132740233));
#41674=CARTESIAN_POINT('Ctrl Pts',(0.0544737170852115,0.144476759001322,
-2.91706042450498));
#41675=CARTESIAN_POINT('Ctrl Pts',(0.101850363836672,0.116040336481254,
-2.91970952160764));
#41676=CARTESIAN_POINT('Ctrl Pts',(0.126406665804976,0.0742301586072307,
-2.92235861871029));
#41677=CARTESIAN_POINT('Ctrl Pts',(0.150962967773281,0.0324199807332077,
-2.92500771581294));
#41678=CARTESIAN_POINT('Ctrl Pts',(0.15269892495843,-0.02276395249477,-2.92765681291559));
#41679=CARTESIAN_POINT('Ctrl Pts',(0.130844409959043,-0.0660664516720163,
-2.93030591001824));
#41680=CARTESIAN_POINT('Ctrl Pts',(0.110648657916751,-0.106082280722433,
-2.93275394001216));
#41681=CARTESIAN_POINT('Ctrl Pts',(0.0703075776504436,-0.135951836020819,
-2.93520197000608));
#41682=CARTESIAN_POINT('Ctrl Pts',(0.0262268935511073,-0.144224038131951,
-2.93765));
#41683=CARTESIAN_POINT('',(-0.14635,-1.79227059055215E-17,-2.93765));
#41684=CARTESIAN_POINT('Origin',(0.,0.,-2.93765));
#41685=CARTESIAN_POINT('',(-0.14635,-1.79227059055215E-17,-2.96765));
#41686=CARTESIAN_POINT('',(-0.14635,-1.79227059055215E-17,-1.487));
#41687=CARTESIAN_POINT('Origin',(0.,0.,-2.96765));
#41688=CARTESIAN_POINT('',(0.128823493644022,-0.0694465980833372,-2.93765));
#41689=CARTESIAN_POINT('Origin',(0.,0.,-2.93765));
#41690=CARTESIAN_POINT('Ctrl Pts',(0.128823493644022,-0.069446598083337,
-2.93765));
#41691=CARTESIAN_POINT('Ctrl Pts',(0.151941943903563,-0.0265618548091487,
-2.93500090289735));
#41692=CARTESIAN_POINT('Ctrl Pts',(0.151761457505771,0.0284019287429394,
-2.9323518057947));
#41693=CARTESIAN_POINT('Ctrl Pts',(0.128356941858912,0.0707835761050192,
-2.92970270869205));
#41694=CARTESIAN_POINT('Ctrl Pts',(0.104952426212054,0.113165223467099,
-2.9270536115894));
#41695=CARTESIAN_POINT('Ctrl Pts',(0.0583238813161294,0.142964734639171,
-2.92440451448675));
#41696=CARTESIAN_POINT('Ctrl Pts',(0.00992989165371453,0.146282598160944,
-2.9217554173841));
#41697=CARTESIAN_POINT('Ctrl Pts',(-0.0384640980087004,0.149600461682717,
-2.91910632028145));
#41698=CARTESIAN_POINT('Ctrl Pts',(-0.088623532437606,0.126436677554191,
-2.9164572231788));
#41699=CARTESIAN_POINT('Ctrl Pts',(-0.11757903185869,0.0875226022274051,
-2.91380812607615));
#41700=CARTESIAN_POINT('Ctrl Pts',(-0.136133705765244,0.0625864763618698,
-2.91211058557886));
#41701=CARTESIAN_POINT('Ctrl Pts',(-0.145981530992649,0.0311828998997731,
-2.91041304508157));
#41702=CARTESIAN_POINT('Ctrl Pts',(-0.146182739311418,-0.000106450303776882,
-2.90871550458429));
#41703=CARTESIAN_POINT('Origin',(0.,0.,-1.487));
#41704=CARTESIAN_POINT('',(-0.146537174558168,-7.96020625374039E-5,-2.85158449541571));
#41705=CARTESIAN_POINT('',(-0.146561971875871,-5.90665209240155E-5,-2.85871550458428));
#41706=CARTESIAN_POINT('',(-0.14635,-1.79227059055215E-17,-1.487));
#41707=CARTESIAN_POINT('Ctrl Pts',(-0.146537174558168,-7.96020625374039E-5,
-2.85158449541571));
#41708=CARTESIAN_POINT('Ctrl Pts',(-0.146249092612562,0.0438734690207087,
-2.85398309302603));
#41709=CARTESIAN_POINT('Ctrl Pts',(-0.125145271349427,0.0880663097270068,
-2.85638169063635));
#41710=CARTESIAN_POINT('Ctrl Pts',(-0.0906335957691385,0.115214904500943,
-2.85878028824667));
#41711=CARTESIAN_POINT('Ctrl Pts',(-0.0525176652796136,0.145198784851356,
-2.86142938534933));
#41712=CARTESIAN_POINT('Ctrl Pts',(0.00195287717864085,0.154392461047573,
-2.86407848245198));
#41713=CARTESIAN_POINT('Ctrl Pts',(0.0477983995988501,0.138579477442402,
-2.86672757955463));
#41714=CARTESIAN_POINT('Ctrl Pts',(0.0936439220190594,0.122766493837231,
-2.86937667665728));
#41715=CARTESIAN_POINT('Ctrl Pts',(0.130864424401223,0.0819468504306727,
-2.87202577375993));
#41716=CARTESIAN_POINT('Ctrl Pts',(0.142390573434243,0.0348407087048676,
-2.87467487086258));
#41717=CARTESIAN_POINT('Ctrl Pts',(0.153916722467262,-0.0122654330209376,
-2.87732396796523));
#41718=CARTESIAN_POINT('Ctrl Pts',(0.139748518151136,-0.0656580730659899,
-2.87997306506788));
#41719=CARTESIAN_POINT('Ctrl Pts',(0.106383941342532,-0.10085284189918,
-2.88262216217053));
#41720=CARTESIAN_POINT('Ctrl Pts',(0.0730193645339283,-0.13604761073237,
-2.88527125927318));
#41721=CARTESIAN_POINT('Ctrl Pts',(0.0204584152328461,-0.153044508353697,
-2.88792035637583));
#41722=CARTESIAN_POINT('Ctrl Pts',(-0.027195887990429,-0.144046802896069,
-2.89056945347848));
#41723=CARTESIAN_POINT('Ctrl Pts',(-0.0748501912137042,-0.13504909743844,
-2.89321855058113));
#41724=CARTESIAN_POINT('Ctrl Pts',(-0.117597848359172,-0.100056788901855,
-2.89586764768378));
#41725=CARTESIAN_POINT('Ctrl Pts',(-0.135833128116005,-0.055121039752474,
-2.89851674478643));
#41726=CARTESIAN_POINT('Ctrl Pts',(-0.142872166799927,-0.0377752967328191,
-2.89953932832952));
#41727=CARTESIAN_POINT('Ctrl Pts',(-0.146258730271021,-0.0189479279290693,
-2.90056191187262));
#41728=CARTESIAN_POINT('Ctrl Pts',(-0.146158606821014,-8.60648302992845E-5,
-2.90158449541571));
#41729=CARTESIAN_POINT('Ctrl Pts',(-0.146182739311418,-0.000106450303776882,
-2.90871550458429));
#41730=CARTESIAN_POINT('Ctrl Pts',(-0.146295526667645,-0.0176457007141658,
-2.90776394797892));
#41731=CARTESIAN_POINT('Ctrl Pts',(-0.143377187945856,-0.0351490593508527,
-2.90681239137356));
#41732=CARTESIAN_POINT('Ctrl Pts',(-0.137262197911326,-0.0514572684605561,
-2.9058608347682));
#41733=CARTESIAN_POINT('Ctrl Pts',(-0.120238300129616,-0.0968586972966848,
-2.90321173766555));
#41734=CARTESIAN_POINT('Ctrl Pts',(-0.0784389401529336,-0.132997188443895,
-2.90056264056289));
#41735=CARTESIAN_POINT('Ctrl Pts',(-0.0310416975091987,-0.143270901492602,
-2.89791354346024));
#41736=CARTESIAN_POINT('Ctrl Pts',(0.0163555451345362,-0.153544614541308,
-2.89526444635759));
#41737=CARTESIAN_POINT('Ctrl Pts',(0.0693506704453232,-0.13795354949151,
-2.89261534925494));
#41738=CARTESIAN_POINT('Ctrl Pts',(0.103645083731081,-0.103662905171766,
-2.88996625215229));
#41739=CARTESIAN_POINT('Ctrl Pts',(0.137939497016838,-0.0693722608520209,
-2.88731715504964));
#41740=CARTESIAN_POINT('Ctrl Pts',(0.153533198277566,-0.0163820372623291,
-2.88466805794699));
#41741=CARTESIAN_POINT('Ctrl Pts',(0.143272624045871,0.0310148776620776,
-2.88201896084434));
#41742=CARTESIAN_POINT('Ctrl Pts',(0.133012049814177,0.0784117925864847,
-2.87936986374169));
#41743=CARTESIAN_POINT('Ctrl Pts',(0.0968972000900611,0.120215398845607,
-2.87672076663904));
#41744=CARTESIAN_POINT('Ctrl Pts',(0.0514913441008033,0.137250642800901,
-2.87407166953639));
#41745=CARTESIAN_POINT('Ctrl Pts',(0.0060854881115459,0.154285886756194,
-2.87142257243374));
#41746=CARTESIAN_POINT('Ctrl Pts',(-0.0486113741428529,0.14655276840766,
-2.86877347533109));
#41747=CARTESIAN_POINT('Ctrl Pts',(-0.087516338371486,0.117599867637059,
-2.86612437822844));
#41748=CARTESIAN_POINT('Ctrl Pts',(-0.123785546700601,0.0906084846451613,
-2.86365475368039));
#41749=CARTESIAN_POINT('Ctrl Pts',(-0.146330131439324,0.0451751432555005,
-2.86118512913233));
#41750=CARTESIAN_POINT('Ctrl Pts',(-0.146561971875871,-5.90665209240155E-5,
-2.85871550458428));
#41751=CARTESIAN_POINT('Origin',(0.,0.,-1.487));
#41752=CARTESIAN_POINT('',(-0.146403203488696,0.000129450652049418,-2.80158449541571));
#41753=CARTESIAN_POINT('',(-0.146363430029852,0.000133824904544822,-2.80871550458428));
#41754=CARTESIAN_POINT('',(-0.14635,-1.79227059055215E-17,-1.487));
#41755=CARTESIAN_POINT('Ctrl Pts',(-0.146403203488696,0.000129450652049418,
-2.80158449541571));
#41756=CARTESIAN_POINT('Ctrl Pts',(-0.146491477515772,0.00970999864112991,
-2.80210607997414));
#41757=CARTESIAN_POINT('Ctrl Pts',(-0.145631706000451,0.01927477608682,
-2.80262766453258));
#41758=CARTESIAN_POINT('Ctrl Pts',(-0.143766246362832,0.0286392135733044,
-2.80314924909101));
#41759=CARTESIAN_POINT('Ctrl Pts',(-0.134291687269365,0.0762006373391004,
-2.80579834619366));
#41760=CARTESIAN_POINT('Ctrl Pts',(-0.098874759612967,0.118594163677882,
-2.80844744329632));
#41761=CARTESIAN_POINT('Ctrl Pts',(-0.053757403740153,0.136378441311147,
-2.81109654039897));
#41762=CARTESIAN_POINT('Ctrl Pts',(-0.0086400478673393,0.154162718944412,
-2.81374563750162));
#41763=CARTESIAN_POINT('Ctrl Pts',(0.0461777362218906,0.147337747872162,
-2.81639473460426));
#41764=CARTESIAN_POINT('Ctrl Pts',(0.085556925217133,0.119033402370627,
-2.81904383170692));
#41765=CARTESIAN_POINT('Ctrl Pts',(0.124936114212376,0.0907290568690924,
-2.82169292880957));
#41766=CARTESIAN_POINT('Ctrl Pts',(0.148876708113631,0.0409453369382727,
-2.82434202591222));
#41767=CARTESIAN_POINT('Ctrl Pts',(0.146399723101655,-0.00748730274776978,
-2.82699112301487));
#41768=CARTESIAN_POINT('Ctrl Pts',(0.143922738089679,-0.0559199424338124,
-2.82964022011752));
#41769=CARTESIAN_POINT('Ctrl Pts',(0.115028174164472,-0.103001501875078,
-2.83228931722017));
#41770=CARTESIAN_POINT('Ctrl Pts',(0.0729668743621239,-0.127140752828838,
-2.83493841432282));
#41771=CARTESIAN_POINT('Ctrl Pts',(0.0309055745597762,-0.151280003782598,
-2.83758751142547));
#41772=CARTESIAN_POINT('Ctrl Pts',(-0.0243224611197121,-0.152476946248854,
-2.84023660852812));
#41773=CARTESIAN_POINT('Ctrl Pts',(-0.0673900900429651,-0.130182626839244,
-2.84288570563077));
#41774=CARTESIAN_POINT('Ctrl Pts',(-0.110457718966218,-0.107888307429635,
-2.84553480273342));
#41775=CARTESIAN_POINT('Ctrl Pts',(-0.141364941133235,-0.0621027261441617,
-2.84818389983607));
#41776=CARTESIAN_POINT('Ctrl Pts',(-0.145937892956347,-0.0138228932491204,
-2.85083299693872));
#41777=CARTESIAN_POINT('Ctrl Pts',(-0.146370312783083,-0.00925753638929341,
-2.85108349643105));
#41778=CARTESIAN_POINT('Ctrl Pts',(-0.146567260630468,-0.00466987679026642,
-2.85133399592338));
#41779=CARTESIAN_POINT('Ctrl Pts',(-0.146537174558168,-7.96020625374039E-5,
-2.85158449541571));
#41780=CARTESIAN_POINT('Ctrl Pts',(-0.146561971875871,-5.90665209240155E-5,
-2.85871550458428));
#41781=CARTESIAN_POINT('Ctrl Pts',(-0.146578820184024,-0.0033463270036002,
-2.85853603202968));
#41782=CARTESIAN_POINT('Ctrl Pts',(-0.146477829990726,-0.00663253582850726,
-2.85835655947508));
#41783=CARTESIAN_POINT('Ctrl Pts',(-0.14625570520285,-0.0099105386052108,
-2.85817708692048));
#41784=CARTESIAN_POINT('Ctrl Pts',(-0.142977041602714,-0.0582953608842119,
-2.85552798981783));
#41785=CARTESIAN_POINT('Ctrl Pts',(-0.113306648199574,-0.104892322249546,
-2.85287889271518));
#41786=CARTESIAN_POINT('Ctrl Pts',(-0.0708513314510232,-0.128331785211355,
-2.85022979561253));
#41787=CARTESIAN_POINT('Ctrl Pts',(-0.0283960147024727,-0.151771248173164,
-2.84758069850988));
#41788=CARTESIAN_POINT('Ctrl Pts',(0.0268442253914879,-0.152053212731447,
-2.84493160140723));
#41789=CARTESIAN_POINT('Ctrl Pts',(0.0695367248469116,-0.12904869809198,
-2.84228250430458));
#41790=CARTESIAN_POINT('Ctrl Pts',(0.112229224302335,-0.106044183452514,
-2.83963340720193));
#41791=CARTESIAN_POINT('Ctrl Pts',(0.142373983119222,-0.0597531896152975,
-2.83698431009928));
#41792=CARTESIAN_POINT('Ctrl Pts',(0.146146788437797,-0.011404249008567,
-2.83433521299663));
#41793=CARTESIAN_POINT('Ctrl Pts',(0.149919593756371,0.0369446915981632,
-2.83168611589398));
#41794=CARTESIAN_POINT('Ctrl Pts',(0.127320445576634,0.0873515789744077,
-2.82903701879133));
#41795=CARTESIAN_POINT('Ctrl Pts',(0.0887131716818962,0.116700100359139,
-2.82638792168868));
#41796=CARTESIAN_POINT('Ctrl Pts',(0.0501058977871583,0.14604862174387,
-2.82373882458603));
#41797=CARTESIAN_POINT('Ctrl Pts',(-0.00450950182258007,0.154338777137088,
-2.82108972748338));
#41798=CARTESIAN_POINT('Ctrl Pts',(-0.0500868268902308,0.137768810843643,
-2.81844063038073));
#41799=CARTESIAN_POINT('Ctrl Pts',(-0.0956641519578814,0.121198844550198,
-2.81579153327808));
#41800=CARTESIAN_POINT('Ctrl Pts',(-0.132203402483444,0.0797687565700892,
-2.81314243617543));
#41801=CARTESIAN_POINT('Ctrl Pts',(-0.142947943413378,0.0324780508505072,
-2.81049333907278));
#41802=CARTESIAN_POINT('Ctrl Pts',(-0.145351531590539,0.0218989687009335,
-2.80990072757661));
#41803=CARTESIAN_POINT('Ctrl Pts',(-0.146464271988682,0.0110266029474243,
-2.80930811608045));
#41804=CARTESIAN_POINT('Ctrl Pts',(-0.146363430029852,0.000133824904544822,
-2.80871550458428));
#41805=CARTESIAN_POINT('Origin',(0.,0.,-1.487));
#41806=CARTESIAN_POINT('',(-0.146109113220983,9.39517128401013E-6,-2.75158449541571));
#41807=CARTESIAN_POINT('',(-0.146109487156769,-1.22079509434409E-5,-2.75871550458428));
#41808=CARTESIAN_POINT('',(-0.14635,-1.79227059055215E-17,-1.487));
#41809=CARTESIAN_POINT('Ctrl Pts',(-0.146109113220983,9.39517128401013E-6,
-2.75158449541571));
#41810=CARTESIAN_POINT('Ctrl Pts',(-0.146122761734058,0.0238929355757029,
-2.75287816402491));
#41811=CARTESIAN_POINT('Ctrl Pts',(-0.140597949611965,0.047770526414132,
-2.7541718326341));
#41812=CARTESIAN_POINT('Ctrl Pts',(-0.129500331978527,0.0686920815018531,
-2.7554655012433));
#41813=CARTESIAN_POINT('Ctrl Pts',(-0.106775295203236,0.111533989059758,
-2.75811459834595));
#41814=CARTESIAN_POINT('Ctrl Pts',(-0.0606821498632086,0.141980530548785,
-2.7607636954486));
#41815=CARTESIAN_POINT('Ctrl Pts',(-0.0123588683584905,0.146069149401598,
-2.76341279255126));
#41816=CARTESIAN_POINT('Ctrl Pts',(0.0359644131462274,0.150157768254412,
-2.76606188965391));
#41817=CARTESIAN_POINT('Ctrl Pts',(0.0865178308156365,0.127888464471012,
-2.76871098675656));
#41818=CARTESIAN_POINT('Ctrl Pts',(0.116117964761986,0.0894737743849098,
-2.77136008385921));
#41819=CARTESIAN_POINT('Ctrl Pts',(0.145718098708336,0.0510590842988072,
-2.77400918096186));
#41820=CARTESIAN_POINT('Ctrl Pts',(0.154364948931627,-0.00350099208999865,
-2.77665827806451));
#41821=CARTESIAN_POINT('Ctrl Pts',(0.138093134336948,-0.0491856107813916,
-2.77930737516716));
#41822=CARTESIAN_POINT('Ctrl Pts',(0.121821319742268,-0.0948702294727843,
-2.78195647226981));
#41823=CARTESIAN_POINT('Ctrl Pts',(0.0806308403296187,-0.131679390466764,
-2.78460556937246));
#41824=CARTESIAN_POINT('Ctrl Pts',(0.0334113427175706,-0.142732687816649,
-2.78725466647511));
#41825=CARTESIAN_POINT('Ctrl Pts',(-0.0138081548944779,-0.153785985166534,
-2.78990376357776));
#41826=CARTESIAN_POINT('Ctrl Pts',(-0.0670566707059247,-0.139083418872324,
-2.79255286068041));
#41827=CARTESIAN_POINT('Ctrl Pts',(-0.10191483334638,-0.105367475128813,
-2.79520195778306));
#41828=CARTESIAN_POINT('Ctrl Pts',(-0.129909721948874,-0.0782899122932978,
-2.79732947032728));
#41829=CARTESIAN_POINT('Ctrl Pts',(-0.146043138956694,-0.0389490375769943,
-2.79945698287149));
#41830=CARTESIAN_POINT('Ctrl Pts',(-0.146403203488696,0.000129450652049418,
-2.80158449541571));
#41831=CARTESIAN_POINT('Ctrl Pts',(-0.146363430029852,0.000133824904544822,
-2.80871550458428));
#41832=CARTESIAN_POINT('Ctrl Pts',(-0.146013487380734,-0.0376663889030354,
-2.8066590189778));
#41833=CARTESIAN_POINT('Ctrl Pts',(-0.131049162627967,-0.075712414620085,
-2.80460253337131));
#41834=CARTESIAN_POINT('Ctrl Pts',(-0.104699336383414,-0.102601106132693,
-2.80254604776482));
#41835=CARTESIAN_POINT('Ctrl Pts',(-0.070756357089213,-0.137238233937254,
-2.79989695066217));
#41836=CARTESIAN_POINT('Ctrl Pts',(-0.0179205671665077,-0.153361166087323,
-2.79724785355952));
#41837=CARTESIAN_POINT('Ctrl Pts',(0.0295779366406567,-0.143576053231004,
-2.79459875645687));
#41838=CARTESIAN_POINT('Ctrl Pts',(0.0770764404478212,-0.133790940374685,
-2.79194965935422));
#41839=CARTESIAN_POINT('Ctrl Pts',(0.119237658139444,-0.0980977825119792,
-2.78930056225157));
#41840=CARTESIAN_POINT('Ctrl Pts',(0.136726768918096,-0.0528651917123114,
-2.78665146514892));
#41841=CARTESIAN_POINT('Ctrl Pts',(0.154215879696748,-0.00763260091264373,
-2.78400236804627));
#41842=CARTESIAN_POINT('Ctrl Pts',(0.147032883562428,0.0471394228239861,
-2.78135327094362));
#41843=CARTESIAN_POINT('Ctrl Pts',(0.118471849500886,0.0863328363546023,
-2.77870417384097));
#41844=CARTESIAN_POINT('Ctrl Pts',(0.0899108154393433,0.125526249885218,
-2.77605507673832));
#41845=CARTESIAN_POINT('Ctrl Pts',(0.0399717434505784,0.149141053209821,
-2.77340597963567));
#41846=CARTESIAN_POINT('Ctrl Pts',(-0.00844368115681214,0.146347674830144,
-2.77075688253302));
#41847=CARTESIAN_POINT('Ctrl Pts',(-0.056859105764203,0.143554296450466,
-2.76810778543037));
#41848=CARTESIAN_POINT('Ctrl Pts',(-0.103750882990219,0.114352736366508,
-2.76545868832772));
#41849=CARTESIAN_POINT('Ctrl Pts',(-0.127614793689341,0.0721346115032102,
-2.76280959122507));
#41850=CARTESIAN_POINT('Ctrl Pts',(-0.13990840596606,0.0503857345205872,
-2.76144489567814));
#41851=CARTESIAN_POINT('Ctrl Pts',(-0.146090776026834,0.0251824610964542,
-2.76008020013121));
#41852=CARTESIAN_POINT('Ctrl Pts',(-0.146109487156769,-1.22079509434409E-5,
-2.75871550458428));
#41853=CARTESIAN_POINT('Origin',(0.,0.,-1.487));
#41854=CARTESIAN_POINT('',(-0.146368629392587,-0.000133465523585494,-2.70158449541571));
#41855=CARTESIAN_POINT('',(-0.146408351835359,-0.000128600226034899,-2.70871550458428));
#41856=CARTESIAN_POINT('',(-0.14635,-1.79227059055215E-17,-1.487));
#41857=CARTESIAN_POINT('Ctrl Pts',(-0.146368629392587,-0.000133465523585494,
-2.70158449541571));
#41858=CARTESIAN_POINT('Ctrl Pts',(-0.14601683807807,0.0378336302900692,
-2.70365024807567));
#41859=CARTESIAN_POINT('Ctrl Pts',(-0.13090301761128,0.0760490326861501,
-2.70571600073563));
#41860=CARTESIAN_POINT('Ctrl Pts',(-0.104340252656597,0.102966255230573,
-2.7077817533956));
#41861=CARTESIAN_POINT('Ctrl Pts',(-0.0702764728809716,0.137484587282563,
-2.71043085049825));
#41862=CARTESIAN_POINT('Ctrl Pts',(-0.017384676891153,0.153422838553933,
-2.71307994760089));
#41863=CARTESIAN_POINT('Ctrl Pts',(0.0300793525132317,0.143471845993703,
-2.71572904470354));
#41864=CARTESIAN_POINT('Ctrl Pts',(0.0775433819176172,0.133520853433473,
-2.71837814180619));
#41865=CARTESIAN_POINT('Ctrl Pts',(0.119579644736569,0.0976806170416416,
-2.72102723890885));
#41866=CARTESIAN_POINT('Ctrl Pts',(0.136910624647343,0.0523872016738897,
-2.7236763360115));
#41867=CARTESIAN_POINT('Ctrl Pts',(0.154241604558118,0.00709378630613784,
-2.72632543311415));
#41868=CARTESIAN_POINT('Ctrl Pts',(0.146867301560715,-0.0476528080375341,
-2.7289745302168));
#41869=CARTESIAN_POINT('Ctrl Pts',(0.118169515957076,-0.0867462018737963,
-2.73162362731945));
#41870=CARTESIAN_POINT('Ctrl Pts',(0.0894717303534362,-0.125839595710059,
-2.7342727244221));
#41871=CARTESIAN_POINT('Ctrl Pts',(0.0394504621435592,-0.149279789038911,
-2.73692182152475));
#41872=CARTESIAN_POINT('Ctrl Pts',(-0.00895490847948087,-0.146317284193646,
-2.7395709186274));
#41873=CARTESIAN_POINT('Ctrl Pts',(-0.0573602791025203,-0.143354779348381,
-2.74222001573005));
#41874=CARTESIAN_POINT('Ctrl Pts',(-0.104149752138723,-0.113989576329,-2.7448691128327));
#41875=CARTESIAN_POINT('Ctrl Pts',(-0.127866024551547,-0.0716883380059181,
-2.74751820993535));
#41876=CARTESIAN_POINT('Ctrl Pts',(-0.140000616127923,-0.0500446226154691,
-2.7488736384288));
#41877=CARTESIAN_POINT('Ctrl Pts',(-0.146094813126366,-0.0250143481262689,
-2.75022906692226));
#41878=CARTESIAN_POINT('Ctrl Pts',(-0.146109113220983,9.39517128401013E-6,
-2.75158449541571));
#41879=CARTESIAN_POINT('Ctrl Pts',(-0.146109487156769,-1.22079509434409E-5,
-2.75871550458428));
#41880=CARTESIAN_POINT('Ctrl Pts',(-0.146127097388187,-0.0237245093453919,
-2.75743110302856));
#41881=CARTESIAN_POINT('Ctrl Pts',(-0.140685008674315,-0.0474291890808367,
-2.75614670147284));
#41882=CARTESIAN_POINT('Ctrl Pts',(-0.129739522674641,-0.0682392408035371,
-2.75486229991711));
#41883=CARTESIAN_POINT('Ctrl Pts',(-0.107164296788595,-0.11116027860435,
-2.75221320281446));
#41884=CARTESIAN_POINT('Ctrl Pts',(-0.0611778008442754,-0.14176766456334,
-2.74956410571181));
#41885=CARTESIAN_POINT('Ctrl Pts',(-0.0128690985436487,-0.14602508011577,
-2.74691500860916));
#41886=CARTESIAN_POINT('Ctrl Pts',(0.035439603756978,-0.150282495668201,
-2.74426591150651));
#41887=CARTESIAN_POINT('Ctrl Pts',(0.0860705124139122,-0.128189940814073,
-2.74161681440386));
#41888=CARTESIAN_POINT('Ctrl Pts',(0.115804670657886,-0.0898788962079824,
-2.73896771730121));
#41889=CARTESIAN_POINT('Ctrl Pts',(0.145538828901859,-0.0515678516018915,
-2.73631862019856));
#41890=CARTESIAN_POINT('Ctrl Pts',(0.154376236732872,0.00296168275616224,
-2.73366952309591));
#41891=CARTESIAN_POINT('Ctrl Pts',(0.138264124904087,0.0487028694361347,
-2.73102042599326));
#41892=CARTESIAN_POINT('Ctrl Pts',(0.122152013075302,0.0944440561161064,
-2.72837132889061));
#41893=CARTESIAN_POINT('Ctrl Pts',(0.081090381586721,0.131396895117997,
-2.72572223178796));
#41894=CARTESIAN_POINT('Ctrl Pts',(0.0339097881036398,0.142615090353666,
-2.72307313468531));
#41895=CARTESIAN_POINT('Ctrl Pts',(-0.0132708053794418,0.153833285589334,
-2.72042403758266));
#41896=CARTESIAN_POINT('Ctrl Pts',(-0.0665703608570236,0.13931683705878,
-2.71777494048001));
#41897=CARTESIAN_POINT('Ctrl Pts',(-0.10154610006969,0.105722879680012,
-2.71512584337736));
#41898=CARTESIAN_POINT('Ctrl Pts',(-0.129757767316244,0.0786257669842071,
-2.71298906377966));
#41899=CARTESIAN_POINT('Ctrl Pts',(-0.146047695012257,0.0391165514560332,
-2.71085228418197));
#41900=CARTESIAN_POINT('Ctrl Pts',(-0.146408351835359,-0.0001286002260349,
-2.70871550458428));
#41901=CARTESIAN_POINT('Origin',(0.,0.,-1.487));
#41902=CARTESIAN_POINT('',(-0.146559056518854,6.20051383258494E-5,-2.65158449541571));
#41903=CARTESIAN_POINT('',(-0.146533501836025,8.20954179803956E-5,-2.65871550458428));
#41904=CARTESIAN_POINT('',(-0.14635,-1.79227059055215E-17,-1.487));
#41905=CARTESIAN_POINT('Ctrl Pts',(-0.146559056518854,6.20051383258494E-5,
-2.65158449541571));
#41906=CARTESIAN_POINT('Ctrl Pts',(-0.146577480383996,0.00351919868299243,
-2.65177323502378));
#41907=CARTESIAN_POINT('Ctrl Pts',(-0.146465774681179,0.00697518102620523,
-2.65196197463186));
#41908=CARTESIAN_POINT('Ctrl Pts',(-0.146220135174594,0.0104216174415365,
-2.65215071423993));
#41909=CARTESIAN_POINT('Ctrl Pts',(-0.142772406783976,0.0587948487705055,
-2.65479981134258));
#41910=CARTESIAN_POINT('Ctrl Pts',(-0.112939510581635,0.10528751744827,
-2.65744890844523));
#41911=CARTESIAN_POINT('Ctrl Pts',(-0.0704025900606613,0.128578432691205,
-2.66009800554788));
#41912=CARTESIAN_POINT('Ctrl Pts',(-0.027865669539689,0.15186934793414,
-2.66274710265053));
#41913=CARTESIAN_POINT('Ctrl Pts',(0.027375275299915,0.151958509742246,
-2.66539619975318));
#41914=CARTESIAN_POINT('Ctrl Pts',(0.0699871595333896,0.128805029175963,
-2.66804529685583));
#41915=CARTESIAN_POINT('Ctrl Pts',(0.112599043766865,0.105651548609678,
-2.67069439395849));
#41916=CARTESIAN_POINT('Ctrl Pts',(0.142581867394211,0.0592554256690021,
-2.67334349106114));
#41917=CARTESIAN_POINT('Ctrl Pts',(0.146185731324473,0.0108935759831704,
-2.67599258816379));
#41918=CARTESIAN_POINT('Ctrl Pts',(0.149789595254736,-0.0374682737026606,
-2.67864168526644));
#41919=CARTESIAN_POINT('Ctrl Pts',(0.127014499487917,-0.087795850133647,
-2.68129078236909));
#41920=CARTESIAN_POINT('Ctrl Pts',(0.0883049329244487,-0.117009302458371,
-2.68393987947174));
#41921=CARTESIAN_POINT('Ctrl Pts',(0.0495953663609803,-0.146222754783096,
-2.68658897657439));
#41922=CARTESIAN_POINT('Ctrl Pts',(-0.00504867099913701,-0.154322083001559,
-2.68923807367704));
#41923=CARTESIAN_POINT('Ctrl Pts',(-0.0505678315451675,-0.137592995655226,
-2.69188717077969));
#41924=CARTESIAN_POINT('Ctrl Pts',(-0.0960869920911979,-0.120863908308893,
-2.69453626788234));
#41925=CARTESIAN_POINT('Ctrl Pts',(-0.132481275823141,-0.0793064053977654,
-2.69718536498499));
#41926=CARTESIAN_POINT('Ctrl Pts',(-0.143060535908398,-0.0319784475258966,
-2.69983446208764));
#41927=CARTESIAN_POINT('Ctrl Pts',(-0.145390141936173,-0.021556594291164,
-2.70041780653033));
#41928=CARTESIAN_POINT('Ctrl Pts',(-0.146467971154205,-0.0108549302842089,
-2.70100115097302));
#41929=CARTESIAN_POINT('Ctrl Pts',(-0.146368629392587,-0.000133465523585494,
-2.70158449541571));
#41930=CARTESIAN_POINT('Ctrl Pts',(-0.146408351835359,-0.0001286002260349,
-2.70871550458428));
#41931=CARTESIAN_POINT('Ctrl Pts',(-0.146494823460208,-0.00953807709170797,
-2.70820318707932));
#41932=CARTESIAN_POINT('Ctrl Pts',(-0.145665591675795,-0.0189323740934643,
-2.70769086957437));
#41933=CARTESIAN_POINT('Ctrl Pts',(-0.143865421359047,-0.0281367777804909,
-2.70717855206941));
#41934=CARTESIAN_POINT('Ctrl Pts',(-0.134557080487986,-0.0757310116352448,
-2.70452945496676));
#41935=CARTESIAN_POINT('Ctrl Pts',(-0.0992884757981104,-0.11824801311777,
-2.7018803578641));
#41936=CARTESIAN_POINT('Ctrl Pts',(-0.0542335261158874,-0.136189802744669,
-2.69923126076145));
#41937=CARTESIAN_POINT('Ctrl Pts',(-0.00917857643366479,-0.154131592371568,
-2.6965821636588));
#41938=CARTESIAN_POINT('Ctrl Pts',(0.0456627182409053,-0.14749817014284,
-2.69393306655615));
#41939=CARTESIAN_POINT('Ctrl Pts',(0.085140549564834,-0.119331573971797,
-2.6912839694535));
#41940=CARTESIAN_POINT('Ctrl Pts',(0.124618380888763,-0.0911649778007544,
-2.68863487235085));
#41941=CARTESIAN_POINT('Ctrl Pts',(0.14873274886205,-0.0414652076873958,
-2.6859857752482));
#41942=CARTESIAN_POINT('Ctrl Pts',(0.146424984348371,0.00697579280672859,
-2.68333667814555));
#41943=CARTESIAN_POINT('Ctrl Pts',(0.144117219834691,0.0554167933008527,
-2.6806875810429));
#41944=CARTESIAN_POINT('Ctrl Pts',(0.115387322834044,0.102599024175743,
-2.67803848394025));
#41945=CARTESIAN_POINT('Ctrl Pts',(0.0734106096394822,0.126885066572302,
-2.6753893868376));
#41946=CARTESIAN_POINT('Ctrl Pts',(0.0314338964449205,0.151171108968862,
-2.67274028973495));
#41947=CARTESIAN_POINT('Ctrl Pts',(-0.0237896329435564,0.15256096288709,
-2.6700911926323));
#41948=CARTESIAN_POINT('Ctrl Pts',(-0.0669348801970078,0.130417251695229,
-2.66744209552965));
#41949=CARTESIAN_POINT('Ctrl Pts',(-0.110080127450459,0.108273540503368,
-2.664792998427));
#41950=CARTESIAN_POINT('Ctrl Pts',(-0.141147092568885,0.0625962642014186,
-2.66214390132435));
#41951=CARTESIAN_POINT('Ctrl Pts',(-0.145888697266746,0.0143326807165443,
-2.6594948042217));
#41952=CARTESIAN_POINT('Ctrl Pts',(-0.146353652014044,0.00960002506664754,
-2.65923503767589));
#41953=CARTESIAN_POINT('Ctrl Pts',(-0.146565475951003,0.00484250084809524,
-2.65897527113009));
#41954=CARTESIAN_POINT('Ctrl Pts',(-0.146533501836025,8.20954179803956E-5,
-2.65871550458428));
#41955=CARTESIAN_POINT('Origin',(0.,0.,-1.487));
#41956=CARTESIAN_POINT('',(-0.146180868122056,9.89477992565866E-5,-2.60158449541571));
#41957=CARTESIAN_POINT('',(-0.146156100335505,8.29196033931501E-5,-2.60871550458429));
#41958=CARTESIAN_POINT('',(-0.14635,-1.79227059055215E-17,-1.487));
#41959=CARTESIAN_POINT('Ctrl Pts',(-0.146180868122056,9.89477992565866E-5,
-2.60158449541571));
#41960=CARTESIAN_POINT('Ctrl Pts',(-0.146290754520116,0.0178157742921191,
-2.60254531907455));
#41961=CARTESIAN_POINT('Ctrl Pts',(-0.143311879978458,0.0354969061612443,
-2.60350614273339));
#41962=CARTESIAN_POINT('Ctrl Pts',(-0.137079022290335,0.0519449678842955,
-2.60446696639222));
#41963=CARTESIAN_POINT('Ctrl Pts',(-0.119894344237327,0.0972940933496845,
-2.60711606349487));
#41964=CARTESIAN_POINT('Ctrl Pts',(-0.0779739962146589,0.133269840155799,
-2.60976516059752));
#41965=CARTESIAN_POINT('Ctrl Pts',(-0.0305423368863008,0.143373999379589,
-2.61241425770017));
#41966=CARTESIAN_POINT('Ctrl Pts',(0.0168893224420581,0.153478158603379,
-2.61506335480282));
#41967=CARTESIAN_POINT('Ctrl Pts',(0.0698322930761075,0.137710730244845,
-2.61771245190547));
#41968=CARTESIAN_POINT('Ctrl Pts',(0.104007323907182,0.103302539243917,
-2.62036154900813));
#41969=CARTESIAN_POINT('Ctrl Pts',(0.138182354738256,0.068894348242991,
-2.62301064611078));
#41970=CARTESIAN_POINT('Ctrl Pts',(0.153589445766355,0.0158453945996729,
-2.62565974321343));
#41971=CARTESIAN_POINT('Ctrl Pts',(0.143163020061337,-0.031516467560496,
-2.62830884031608));
#41972=CARTESIAN_POINT('Ctrl Pts',(0.132736594356318,-0.078878329720666,
-2.63095793741873));
#41973=CARTESIAN_POINT('Ctrl Pts',(0.0964766519181793,-0.120553100397687,
-2.63360703452138));
#41974=CARTESIAN_POINT('Ctrl Pts',(0.0510117316652691,-0.137429040865042,
-2.63625613162403));
#41975=CARTESIAN_POINT('Ctrl Pts',(0.00554681141235967,-0.154304981332397,
-2.63890522872668));
#41976=CARTESIAN_POINT('Ctrl Pts',(-0.049123086655321,-0.146382091590088,
-2.64155432582933));
#41977=CARTESIAN_POINT('Ctrl Pts',(-0.0879267553997137,-0.117293749728846,
-2.64420342293198));
#41978=CARTESIAN_POINT('Ctrl Pts',(-0.12396578813913,-0.0902778582269869,
-2.64666378042656));
#41979=CARTESIAN_POINT('Ctrl Pts',(-0.146318888092397,-0.0450050167475421,
-2.64912413792113));
#41980=CARTESIAN_POINT('Ctrl Pts',(-0.146559056518854,6.20051383258494E-5,
-2.65158449541571));
#41981=CARTESIAN_POINT('Ctrl Pts',(-0.146533501836025,8.20954179803956E-5,
-2.65871550458428));
#41982=CARTESIAN_POINT('Ctrl Pts',(-0.146239404188817,-0.0437040746677485,
-2.65632617402744));
#41983=CARTESIAN_POINT('Ctrl Pts',(-0.125319247018811,-0.0877340040481646,
-2.65393684347059));
#41984=CARTESIAN_POINT('Ctrl Pts',(-0.0910355793483402,-0.114897611025745,
-2.65154751291374));
#41985=CARTESIAN_POINT('Ctrl Pts',(-0.0530246124547761,-0.14501442861536,
-2.64889841581109));
#41986=CARTESIAN_POINT('Ctrl Pts',(0.00141356560964873,-0.154398173126793,
-2.64624931870844));
#41987=CARTESIAN_POINT('Ctrl Pts',(0.0473140127705487,-0.138745529377574,
-2.64360022160579));
#41988=CARTESIAN_POINT('Ctrl Pts',(0.0932144599314493,-0.123092885628354,
-2.64095112450314));
#41989=CARTESIAN_POINT('Ctrl Pts',(0.130577176188825,-0.0824038536184819,
-2.63830202740049));
#41990=CARTESIAN_POINT('Ctrl Pts',(0.142267898783137,-0.0353381196803642,
-2.63565293029784));
#41991=CARTESIAN_POINT('Ctrl Pts',(0.153958621377449,0.0117276142577528,
-2.63300383319519));
#41992=CARTESIAN_POINT('Ctrl Pts',(0.139977350308698,0.0651700501241154,
-2.63035473609254));
#41993=CARTESIAN_POINT('Ctrl Pts',(0.106735792117545,0.100480885783083,
-2.62770563898989));
#41994=CARTESIAN_POINT('Ctrl Pts',(0.0734942339263919,0.135791721442052,
-2.62505654188724));
#41995=CARTESIAN_POINT('Ctrl Pts',(0.0209923886128374,0.152970956893625,
-2.62240744478459));
#41996=CARTESIAN_POINT('Ctrl Pts',(-0.0266927894933914,0.144140323004268,
-2.61975834768194));
#41997=CARTESIAN_POINT('Ctrl Pts',(-0.07437796759962,0.135309689114912,
-2.61710925057929));
#41998=CARTESIAN_POINT('Ctrl Pts',(-0.117246478498522,0.100469185884624,
-2.61446015347664));
#41999=CARTESIAN_POINT('Ctrl Pts',(-0.135639143109211,0.0555964080072815,
-2.61181105637399));
#42000=CARTESIAN_POINT('Ctrl Pts',(-0.142803275345818,0.0381179990142528,
-2.61077920577742));
#42001=CARTESIAN_POINT('Ctrl Pts',(-0.146253974510039,0.0191175106607409,
-2.60974735518085));
#42002=CARTESIAN_POINT('Ctrl Pts',(-0.146156100335505,8.29196033931501E-5,
-2.60871550458429));
#42003=CARTESIAN_POINT('Origin',(0.,0.,-1.487));
#42004=CARTESIAN_POINT('',(-0.146198678720714,-0.000107744948522656,-2.55158449541571));
#42005=CARTESIAN_POINT('',(-0.146230181331583,-0.000119433189373819,-2.55871550458428));
#42006=CARTESIAN_POINT('',(-0.14635,-1.79227059055215E-17,-1.487));
#42007=CARTESIAN_POINT('Ctrl Pts',(-0.146198678720714,-0.000107744948522656,
-2.55158449541571));
#42008=CARTESIAN_POINT('Ctrl Pts',(-0.145981193910011,0.0318359205676525,
-2.55331740312531));
#42009=CARTESIAN_POINT('Ctrl Pts',(-0.135687907137135,0.0639071118611217,
-2.55505031083491));
#42010=CARTESIAN_POINT('Ctrl Pts',(-0.116406189831084,0.0890984680540818,
-2.55678321854451));
#42011=CARTESIAN_POINT('Ctrl Pts',(-0.0869302164906803,0.127608510067782,
-2.55943231564716));
#42012=CARTESIAN_POINT('Ctrl Pts',(-0.0364489496635117,0.15004088925777,
-2.56208141274981));
#42013=CARTESIAN_POINT('Ctrl Pts',(0.0118872785307486,0.146108283987278,
-2.56473050985246));
#42014=CARTESIAN_POINT('Ctrl Pts',(0.0602235067250097,0.142175678716785,
-2.56737960695512));
#42015=CARTESIAN_POINT('Ctrl Pts',(0.106414696286363,0.11187808898581,-2.57002870405777));
#42016=CARTESIAN_POINT('Ctrl Pts',(0.129277912503419,0.0691097632707052,
-2.57267780116042));
#42017=CARTESIAN_POINT('Ctrl Pts',(0.152141128720475,0.0263414375556003,
-2.57532689826307));
#42018=CARTESIAN_POINT('Ctrl Pts',(0.151676371593235,-0.0288976241436341,
-2.57797599536572));
#42019=CARTESIAN_POINT('Ctrl Pts',(0.128096775270796,-0.0712752004963703,
-2.58062509246837));
#42020=CARTESIAN_POINT('Ctrl Pts',(0.104517178948357,-0.113652776849106,
-2.58327418957102));
#42021=CARTESIAN_POINT('Ctrl Pts',(0.0578227434307195,-0.143168867855344,
-2.58592328667367));
#42022=CARTESIAN_POINT('Ctrl Pts',(0.00942718826804761,-0.146287614519936,
-2.58857238377632));
#42023=CARTESIAN_POINT('Ctrl Pts',(-0.038968366894625,-0.149406361184528,
-2.59122148087897));
#42024=CARTESIAN_POINT('Ctrl Pts',(-0.0890650417023317,-0.126127763507476,
-2.59387057798162));
#42025=CARTESIAN_POINT('Ctrl Pts',(-0.117888875064511,-0.0871272126066167,
-2.59651967508427));
#42026=CARTESIAN_POINT('Ctrl Pts',(-0.136258346068636,-0.0622721046854669,
-2.59820794852808));
#42027=CARTESIAN_POINT('Ctrl Pts',(-0.1459877855663,-0.0310314759797697,
-2.5998962219719));
#42028=CARTESIAN_POINT('Ctrl Pts',(-0.146180868122056,9.89477992565866E-5,
-2.60158449541571));
#42029=CARTESIAN_POINT('Ctrl Pts',(-0.146156100335505,8.29196033931501E-5,
-2.60871550458429));
#42030=CARTESIAN_POINT('Ctrl Pts',(-0.146002699574458,-0.0297504942499515,
-2.6070982580782));
#42031=CARTESIAN_POINT('Ctrl Pts',(-0.137132187551342,-0.0596676817879004,
-2.60548101157212));
#42032=CARTESIAN_POINT('Ctrl Pts',(-0.12017929978244,-0.0839397023494568,
-2.60386376506603));
#42033=CARTESIAN_POINT('Ctrl Pts',(-0.0924099735225071,-0.123697982304454,
-2.60121466796338));
#42034=CARTESIAN_POINT('Ctrl Pts',(-0.0429545026801662,-0.148309489690051,
-2.59856557086073));
#42035=CARTESIAN_POINT('Ctrl Pts',(0.00550720300589055,-0.146487570946361,
-2.59591647375808));
#42036=CARTESIAN_POINT('Ctrl Pts',(0.0539689086919474,-0.14466565220267,
-2.59326737665543));
#42037=CARTESIAN_POINT('Ctrl Pts',(0.10143684922172,-0.116410307329694,
-2.59061827955278));
#42038=CARTESIAN_POINT('Ctrl Pts',(0.126142581420765,-0.0746792265574484,
-2.58796918245013));
#42039=CARTESIAN_POINT('Ctrl Pts',(0.15084831361981,-0.0329481457852034,
-2.58532008534748));
#42040=CARTESIAN_POINT('Ctrl Pts',(0.152791837488128,0.0222586708863098,
-2.58267098824483));
#42041=CARTESIAN_POINT('Ctrl Pts',(0.131081867488292,0.0656237894554635,
-2.58002189114218));
#42042=CARTESIAN_POINT('Ctrl Pts',(0.109371897488455,0.108988908024618,
-2.57737279403953));
#42043=CARTESIAN_POINT('Ctrl Pts',(0.0640084336204636,0.140512328491412,
-2.57472369693687));
#42044=CARTESIAN_POINT('Ctrl Pts',(0.015794821771778,0.145737645554986,
-2.57207459983422));
#42045=CARTESIAN_POINT('Ctrl Pts',(-0.0324187900769076,0.150962962618561,
-2.56942550273157));
#42046=CARTESIAN_POINT('Ctrl Pts',(-0.0834825499062879,0.129890176278916,
-2.56677640562893));
#42047=CARTESIAN_POINT('Ctrl Pts',(-0.113978998654238,0.0921831090411383,
-2.56412730852628));
#42048=CARTESIAN_POINT('Ctrl Pts',(-0.134745923529105,0.0665060264716099,
-2.56232337387895));
#42049=CARTESIAN_POINT('Ctrl Pts',(-0.145975594133634,0.0331154724666765,
-2.56051943923161));
#42050=CARTESIAN_POINT('Ctrl Pts',(-0.146230181331583,-0.000119433189373819,
-2.55871550458428));
#42051=CARTESIAN_POINT('Origin',(0.,0.,-1.487));
#42052=CARTESIAN_POINT('',(-0.146571805443423,-4.82250285658153E-5,-2.50158449541571));
#42053=CARTESIAN_POINT('',(-0.14658585947319,-2.49429472847227E-5,-2.50871550458428));
#42054=CARTESIAN_POINT('',(-0.14635,-1.79227059055215E-17,-1.487));
#42055=CARTESIAN_POINT('Ctrl Pts',(-0.146571805443423,-4.82250285658153E-5,
-2.50158449541571));
#42056=CARTESIAN_POINT('Ctrl Pts',(-0.146375076469616,0.0458257689308958,
-2.50408948717608));
#42057=CARTESIAN_POINT('Ctrl Pts',(-0.123091181584723,0.0918718820885898,
-2.50659447893644));
#42058=CARTESIAN_POINT('Ctrl Pts',(-0.0859407318081494,0.118756594161564,
-2.5090994706968));
#42059=CARTESIAN_POINT('Ctrl Pts',(-0.0466531180034015,0.147187910377845,
-2.51174856779945));
#42060=CARTESIAN_POINT('Ctrl Pts',(0.00814235063893784,0.154189806754235,
-2.5143976649021));
#42061=CARTESIAN_POINT('Ctrl Pts',(0.0533168812526686,0.136551265882318,
-2.51704676200475));
#42062=CARTESIAN_POINT('Ctrl Pts',(0.0984914118663987,0.1189127250104,-2.51969585910741));
#42063=CARTESIAN_POINT('Ctrl Pts',(0.13404500445152,0.0766337468901765,
-2.52234495621006));
#42064=CARTESIAN_POINT('Ctrl Pts',(0.143673046859312,0.0291031552711476,
-2.52499405331271));
#42065=CARTESIAN_POINT('Ctrl Pts',(0.153301089267104,-0.0184274363478816,
-2.52764315041536));
#42066=CARTESIAN_POINT('Ctrl Pts',(0.137003581497565,-0.0712096414657163,
-2.53029224751801));
#42067=CARTESIAN_POINT('Ctrl Pts',(0.102254438951422,-0.105037934839297,
-2.53294134462066));
#42068=CARTESIAN_POINT('Ctrl Pts',(0.0675052964052803,-0.138866228212877,
-2.53559044172331));
#42069=CARTESIAN_POINT('Ctrl Pts',(0.0143045190825352,-0.153740609842205,
-2.53823953882596));
#42070=CARTESIAN_POINT('Ctrl Pts',(-0.0329504136852633,-0.142839799350687,
-2.54088863592861));
#42071=CARTESIAN_POINT('Ctrl Pts',(-0.0802053464530617,-0.131938988859169,
-2.54353773303126));
#42072=CARTESIAN_POINT('Ctrl Pts',(-0.121514434665913,-0.0952629862468065,
-2.54618683013391));
#42073=CARTESIAN_POINT('Ctrl Pts',(-0.13793363884552,-0.0496311325219192,
-2.54883592723656));
#42074=CARTESIAN_POINT('Ctrl Pts',(-0.14361221540529,-0.0338493703788515,
-2.54975211662961));
#42075=CARTESIAN_POINT('Ctrl Pts',(-0.146313663076552,-0.0169963809438984,
-2.55066830602266));
#42076=CARTESIAN_POINT('Ctrl Pts',(-0.146198678720714,-0.000107744948522656,
-2.55158449541571));
#42077=CARTESIAN_POINT('Ctrl Pts',(-0.146230181331583,-0.000119433189373819,
-2.55871550458428));
#42078=CARTESIAN_POINT('Ctrl Pts',(-0.146349458125579,-0.0156903378827077,
-2.55787034212896));
#42079=CARTESIAN_POINT('Ctrl Pts',(-0.144059680438183,-0.0312270774277224,
-2.55702517967364));
#42080=CARTESIAN_POINT('Ctrl Pts',(-0.139212983241851,-0.0459203987745881,
-2.55618001721832));
#42081=CARTESIAN_POINT('Ctrl Pts',(-0.124021381414995,-0.0919754912166281,
-2.55353092011567));
#42082=CARTESIAN_POINT('Ctrl Pts',(-0.083709040094762,-0.129744327964798,
-2.55088182301302));
#42083=CARTESIAN_POINT('Ctrl Pts',(-0.0367628980753028,-0.141906402434203,
-2.54823272591037));
#42084=CARTESIAN_POINT('Ctrl Pts',(0.0101832439441568,-0.154068476903608,
-2.54558362880772));
#42085=CARTESIAN_POINT('Ctrl Pts',(0.0637631866628425,-0.140623789094247,
-2.54293453170507));
#42086=CARTESIAN_POINT('Ctrl Pts',(0.099405568329131,-0.107737972469671,
-2.54028543460242));
#42087=CARTESIAN_POINT('Ctrl Pts',(0.135047949995419,-0.074852155845095,
-2.53763633749977));
#42088=CARTESIAN_POINT('Ctrl Pts',(0.15275277060931,-0.0225252104053042,
-2.53498724039712));
#42089=CARTESIAN_POINT('Ctrl Pts',(0.144400731605375,0.0252461172964389,
-2.53233814329447));
#42090=CARTESIAN_POINT('Ctrl Pts',(0.13604869260144,0.0730174449981818,
-2.52968904619182));
#42091=CARTESIAN_POINT('Ctrl Pts',(0.10163979397968,0.116233154961878,-2.52703994908917));
#42092=CARTESIAN_POINT('Ctrl Pts',(0.0569536997824638,0.135074845207396,
-2.52439085198652));
#42093=CARTESIAN_POINT('Ctrl Pts',(0.0122676055852467,0.153916535452915,
-2.52174175488387));
#42094=CARTESIAN_POINT('Ctrl Pts',(-0.0426956841874264,0.148384205980257,
-2.51909265778122));
#42095=CARTESIAN_POINT('Ctrl Pts',(-0.0827304151517853,0.121014941786237,
-2.51644356067857));
#42096=CARTESIAN_POINT('Ctrl Pts',(-0.121660741803148,0.094400690369656,
-2.51386754198047));
#42097=CARTESIAN_POINT('Ctrl Pts',(-0.146474792161809,0.0471376805651769,
-2.51129152328238));
#42098=CARTESIAN_POINT('Ctrl Pts',(-0.14658585947319,-2.49429472847227E-5,
-2.50871550458428));
#42099=CARTESIAN_POINT('Origin',(0.,0.,-1.487));
#42100=CARTESIAN_POINT('',(-0.146343637318237,0.000134580547271598,-2.45158449541571));
#42101=CARTESIAN_POINT('',(-0.146304536544652,0.000133297989308676,-2.45871550458428));
#42102=CARTESIAN_POINT('',(-0.14635,-1.79227059055215E-17,-1.487));
#42103=CARTESIAN_POINT('Ctrl Pts',(-0.146343637318237,0.000134580547271598,
-2.45158449541571));
#42104=CARTESIAN_POINT('Ctrl Pts',(-0.146449762957763,0.0116814355873594,
-2.45221247412419));
#42105=CARTESIAN_POINT('Ctrl Pts',(-0.145198490549426,0.0232055565890608,
-2.45284045283267));
#42106=CARTESIAN_POINT('Ctrl Pts',(-0.142502216361462,0.0343810467066606,
-2.45346843154114));
#42107=CARTESIAN_POINT('Ctrl Pts',(-0.131128117139851,0.081524298685688,
-2.45611752864379));
#42108=CARTESIAN_POINT('Ctrl Pts',(-0.0940397420577331,0.122463550881684,
-2.45876662574644));
#42109=CARTESIAN_POINT('Ctrl Pts',(-0.0482455430596612,0.13842436785282,
-2.46141572284909));
#42110=CARTESIAN_POINT('Ctrl Pts',(-0.00245134406158928,0.154385184823957,
-2.46406481995174));
#42111=CARTESIAN_POINT('Ctrl Pts',(0.0520486788524363,0.145367566570235,
-2.4667139170544));
#42112=CARTESIAN_POINT('Ctrl Pts',(0.0902612220216918,0.115506925505467,
-2.46936301415705));
#42113=CARTESIAN_POINT('Ctrl Pts',(0.128473765190947,0.0856462844406988,
-2.4720121112597));
#42114=CARTESIAN_POINT('Ctrl Pts',(0.150398828615432,0.0349426205648845,
-2.47466120836235));
#42115=CARTESIAN_POINT('Ctrl Pts',(0.145981741881279,-0.0133517443760076,
-2.477310305465));
#42116=CARTESIAN_POINT('Ctrl Pts',(0.141564655147125,-0.0616461093169007,
-2.47995940256765));
#42117=CARTESIAN_POINT('Ctrl Pts',(0.110805418254332,-0.107531175322872,
-2.4826084996703));
#42118=CARTESIAN_POINT('Ctrl Pts',(0.0678099876214229,-0.129964393659791,
-2.48525759677295));
#42119=CARTESIAN_POINT('Ctrl Pts',(0.0248145569885134,-0.152397611996709,
-2.4879066938756));
#42120=CARTESIAN_POINT('Ctrl Pts',(-0.0304170673845123,-0.151378982664575,
-2.49055579097825));
#42121=CARTESIAN_POINT('Ctrl Pts',(-0.072556074869304,-0.127375641470944,
-2.4932048880809));
#42122=CARTESIAN_POINT('Ctrl Pts',(-0.114695082354095,-0.103372300277313,
-2.49585398518355));
#42123=CARTESIAN_POINT('Ctrl Pts',(-0.143741472950652,-0.0563842472221864,
-2.4985030822862));
#42124=CARTESIAN_POINT('Ctrl Pts',(-0.146374788765353,-0.00795985266653731,
-2.50115217938885));
#42125=CARTESIAN_POINT('Ctrl Pts',(-0.146518035638578,-0.00532566687340771,
-2.50129628473114));
#42126=CARTESIAN_POINT('Ctrl Pts',(-0.146583122724603,-0.00268723075550709,
-2.50144039007342));
#42127=CARTESIAN_POINT('Ctrl Pts',(-0.146571805443423,-4.82250285658153E-5,
-2.50158449541571));
#42128=CARTESIAN_POINT('Ctrl Pts',(-0.14658585947319,-2.49429472847227E-5,
-2.50871550458428));
#42129=CARTESIAN_POINT('Ctrl Pts',(-0.146589010312864,-0.00136288714913549,
-2.50864242617973));
#42130=CARTESIAN_POINT('Ctrl Pts',(-0.146572280552286,-0.00270075056156342,
-2.50856934777517));
#42131=CARTESIAN_POINT('Ctrl Pts',(-0.146535428489023,-0.00403805946607697,
-2.50849626937062));
#42132=CARTESIAN_POINT('Ctrl Pts',(-0.145199538705858,-0.0525155976089924,
-2.50584717226796));
#42133=CARTESIAN_POINT('Ctrl Pts',(-0.117421586983486,-0.100264474979443,
-2.50319807516531));
#42134=CARTESIAN_POINT('Ctrl Pts',(-0.0759403346168386,-0.125387412865071,
-2.50054897806266));
#42135=CARTESIAN_POINT('Ctrl Pts',(-0.0344590822501911,-0.150510350750698,
-2.49789988096001));
#42136=CARTESIAN_POINT('Ctrl Pts',(0.0207254707607316,-0.153007349151502,
-2.49525078385736));
#42137=CARTESIAN_POINT('Ctrl Pts',(0.0643061003628465,-0.131733303241195,
-2.49260168675471));
#42138=CARTESIAN_POINT('Ctrl Pts',(0.107886729964961,-0.110459257330887,
-2.48995258965206));
#42139=CARTESIAN_POINT('Ctrl Pts',(0.139863436158269,-0.0654141671094696,
-2.48730349254941));
#42140=CARTESIAN_POINT('Ctrl Pts',(0.14557194019155,-0.0172553746867708,
-2.48465439544676));
#42141=CARTESIAN_POINT('Ctrl Pts',(0.151280444224832,0.0309034177359276,
-2.48200529834411));
#42142=CARTESIAN_POINT('Ctrl Pts',(0.130720746098087,0.0821759123599069,
-2.47935620124146));
#42143=CARTESIAN_POINT('Ctrl Pts',(0.0933213698922176,0.113048925904464,
-2.47670710413881));
#42144=CARTESIAN_POINT('Ctrl Pts',(0.0559219936863476,0.143921939449022,
-2.47405800703616));
#42145=CARTESIAN_POINT('Ctrl Pts',(0.00168293940135239,0.154395471914157,
-2.47140890993351));
#42146=CARTESIAN_POINT('Ctrl Pts',(-0.0445221675671624,0.139666439497234,
-2.46875981283086));
#42147=CARTESIAN_POINT('Ctrl Pts',(-0.0907272745356775,0.124937407080312,
-2.46611071572821));
#42148=CARTESIAN_POINT('Ctrl Pts',(-0.128898434187712,0.0850058097813312,
-2.46346161862556));
#42149=CARTESIAN_POINT('Ctrl Pts',(-0.141530637658034,0.0381839800285859,
-2.46081252152291));
#42150=CARTESIAN_POINT('Ctrl Pts',(-0.144863841843323,0.0258293089483245,
-2.4601135158767));
#42151=CARTESIAN_POINT('Ctrl Pts',(-0.146418894550156,0.01299490498715,
-2.45941451023049));
#42152=CARTESIAN_POINT('Ctrl Pts',(-0.146304536544652,0.000133297989308676,
-2.45871550458428));
#42153=CARTESIAN_POINT('Origin',(0.,0.,-1.487));
#42154=CARTESIAN_POINT('',(-0.146111815181358,-2.28850520822416E-5,-2.40158449541571));
#42155=CARTESIAN_POINT('',(-0.14612072978227,-4.38323123618543E-5,-2.40871550458428));
#42156=CARTESIAN_POINT('',(-0.14635,-1.79227059055215E-17,-1.487));
#42157=CARTESIAN_POINT('Ctrl Pts',(-0.146111815181358,-2.28850520822416E-5,
-2.40158449541571));
#42158=CARTESIAN_POINT('Ctrl Pts',(-0.146075798550186,0.0258236983025542,
-2.40298455817495));
#42159=CARTESIAN_POINT('Ctrl Pts',(-0.139550277491284,0.0516872750199038,
-2.40438462093419));
#42160=CARTESIAN_POINT('Ctrl Pts',(-0.126641700285093,0.0738296538626264,
-2.40578468369343));
#42161=CARTESIAN_POINT('Ctrl Pts',(-0.10221702771199,0.115725855479931,
-2.40843378079608));
#42162=CARTESIAN_POINT('Ctrl Pts',(-0.0549400816815103,0.144299625105766,
-2.41108287789873));
#42163=CARTESIAN_POINT('Ctrl Pts',(-0.00649171671651216,0.146447245295523,
-2.41373197500138));
#42164=CARTESIAN_POINT('Ctrl Pts',(0.0419566482484867,0.14859486548528,
-2.41638107210403));
#42165=CARTESIAN_POINT('Ctrl Pts',(0.0915764321480043,0.124316336238958,
-2.41903016920669));
#42166=CARTESIAN_POINT('Ctrl Pts',(0.119612372501939,0.0847456098274833,
-2.42167926630934));
#42167=CARTESIAN_POINT('Ctrl Pts',(0.147648312855873,0.0451748834160083,
-2.42432836341199));
#42168=CARTESIAN_POINT('Ctrl Pts',(0.154100409664225,-0.00968804016061831,
-2.42697746051464));
#42169=CARTESIAN_POINT('Ctrl Pts',(0.136009779496176,-0.0546834337068921,
-2.42962655761729));
#42170=CARTESIAN_POINT('Ctrl Pts',(0.117919149328128,-0.0996788272531659,
-2.43227565471994));
#42171=CARTESIAN_POINT('Ctrl Pts',(0.0752857921836774,-0.134806690769086,
-2.43492475182259));
#42172=CARTESIAN_POINT('Ctrl Pts',(0.0276610473873672,-0.143957648278959,
-2.43757384892524));
#42173=CARTESIAN_POINT('Ctrl Pts',(-0.0199636974089416,-0.153108605788832,
-2.44022294602789));
#42174=CARTESIAN_POINT('Ctrl Pts',(-0.0725798298571109,-0.136282657292659,
-2.44287204313054));
#42175=CARTESIAN_POINT('Ctrl Pts',(-0.106057984400644,-0.101196057163545,
-2.44552114023319));
#42176=CARTESIAN_POINT('Ctrl Pts',(-0.131600012997177,-0.0744268712250649,
-2.44754225862736));
#42177=CARTESIAN_POINT('Ctrl Pts',(-0.146002077199647,-0.0370284009381002,
-2.44956337702154));
#42178=CARTESIAN_POINT('Ctrl Pts',(-0.146343637318237,0.000134580547271598,
-2.45158449541571));
#42179=CARTESIAN_POINT('Ctrl Pts',(-0.146304536544652,0.000133297989308676,
-2.45871550458428));
#42180=CARTESIAN_POINT('Ctrl Pts',(-0.145985499680331,-0.0357481144981475,
-2.45676541312784));
#42181=CARTESIAN_POINT('Ctrl Pts',(-0.132673392532962,-0.0718412489811016,
-2.4548153216714));
#42182=CARTESIAN_POINT('Ctrl Pts',(-0.108729319967223,-0.0983202558284832,
-2.45286523021495));
#42183=CARTESIAN_POINT('Ctrl Pts',(-0.0762025515174788,-0.134290599726301,
-2.4502161331123));
#42184=CARTESIAN_POINT('Ctrl Pts',(-0.0240557673293792,-0.152519225315428,
-2.44756703600965));
#42185=CARTESIAN_POINT('Ctrl Pts',(0.0237969066489193,-0.144646620979046,
-2.444917938907));
#42186=CARTESIAN_POINT('Ctrl Pts',(0.0716495806272191,-0.136774016642663,
-2.44226884180435));
#42187=CARTESIAN_POINT('Ctrl Pts',(0.115208144395718,-0.102800182380768,
-2.4396197447017));
#42188=CARTESIAN_POINT('Ctrl Pts',(0.134496965778837,-0.0583052649680928,
-2.43697064759905));
#42189=CARTESIAN_POINT('Ctrl Pts',(0.153785787161955,-0.0138103475554188,
-2.4343215504964));
#42190=CARTESIAN_POINT('Ctrl Pts',(0.148804866159696,0.0412056530080348,
-2.43167245339375));
#42191=CARTESIAN_POINT('Ctrl Pts',(0.121838415960665,0.0815128095633379,
-2.4290233562911));
#42192=CARTESIAN_POINT('Ctrl Pts',(0.0948719657616343,0.121819966118641,
-2.42637425918845));
#42193=CARTESIAN_POINT('Ctrl Pts',(0.0459199863658311,0.147418278665793,
-2.4237251620858));
#42194=CARTESIAN_POINT('Ctrl Pts',(-0.00256850990682517,0.146568552164411,
-2.42107606498315));
#42195=CARTESIAN_POINT('Ctrl Pts',(-0.0510570061794814,0.145718825663028,
-2.4184269678805));
#42196=CARTESIAN_POINT('Ctrl Pts',(-0.0990820193289911,0.118421060113111,
-2.41577787077785));
#42197=CARTESIAN_POINT('Ctrl Pts',(-0.124619636836098,0.0771938070155387,
-2.4131287736752));
#42198=CARTESIAN_POINT('Ctrl Pts',(-0.138801120014761,0.0542995963029285,
-2.41165768397823));
#42199=CARTESIAN_POINT('Ctrl Pts',(-0.14604799843459,0.0271098463392561,
-2.41018659428125));
#42200=CARTESIAN_POINT('Ctrl Pts',(-0.14612072978227,-4.38323123618543E-5,
-2.40871550458428));
#42201=CARTESIAN_POINT('Origin',(0.,0.,-1.487));
#42202=CARTESIAN_POINT('',(-0.14642783004434,-0.00012476929814137,-2.35158449541571));
#42203=CARTESIAN_POINT('',(-0.146465637571143,-0.000114315844697511,-2.35871550458428));
#42204=CARTESIAN_POINT('',(-0.14635,-1.79227059055215E-17,-1.487));
#42205=CARTESIAN_POINT('Ctrl Pts',(-0.14642783004434,-0.00012476929814137,
-2.35158449541571));
#42206=CARTESIAN_POINT('Ctrl Pts',(-0.146066603696939,0.0397562668171756,
-2.35375664222571));
#42207=CARTESIAN_POINT('Ctrl Pts',(-0.129170826335352,0.0799065680416143,
-2.35592878903572));
#42208=CARTESIAN_POINT('Ctrl Pts',(-0.100127500298616,0.107067370027125,
-2.35810093584572));
#42209=CARTESIAN_POINT('Ctrl Pts',(-0.0647069704795052,0.14019201957387,
-2.36075003294837));
#42210=CARTESIAN_POINT('Ctrl Pts',(-0.0112186082459791,0.153996549344,-2.36339913005103));
#42211=CARTESIAN_POINT('Ctrl Pts',(0.0358082227771749,0.142150305037009,
-2.36604822715368));
#42212=CARTESIAN_POINT('Ctrl Pts',(0.0828350538003276,0.130304060730019,
-2.36869732425633));
#42213=CARTESIAN_POINT('Ctrl Pts',(0.123400353613109,0.092807042345909,
-2.37134642135898));
#42214=CARTESIAN_POINT('Ctrl Pts',(0.138901178545045,0.0468551025969656,
-2.37399551846163));
#42215=CARTESIAN_POINT('Ctrl Pts',(0.154402003476981,0.000903162848020875,
-2.37664461556428));
#42216=CARTESIAN_POINT('Ctrl Pts',(0.144838353528071,-0.053503698265758,
-2.37929371266693));
#42217=CARTESIAN_POINT('Ctrl Pts',(0.114596047171364,-0.0914149003897779,
-2.38194280976958));
#42218=CARTESIAN_POINT('Ctrl Pts',(0.0843537408146581,-0.129326102513797,
-2.38459190687223));
#42219=CARTESIAN_POINT('Ctrl Pts',(0.0334327780501559,-0.150741645648058,
-2.38724100397488));
#42220=CARTESIAN_POINT('Ctrl Pts',(-0.0148148677279785,-0.145840521580174,
-2.38989010107753));
#42221=CARTESIAN_POINT('Ctrl Pts',(-0.0630625135061135,-0.140939397512289,
-2.39253919818018));
#42222=CARTESIAN_POINT('Ctrl Pts',(-0.108636842297881,-0.109721606242258,
-2.39518829528283));
#42223=CARTESIAN_POINT('Ctrl Pts',(-0.130637807135901,-0.0665033938028552,
-2.39783739238548));
#42224=CARTESIAN_POINT('Ctrl Pts',(-0.141011137975052,-0.0461262503815869,
-2.39908642672889));
#42225=CARTESIAN_POINT('Ctrl Pts',(-0.146143946604733,-0.0230813301515235,
-2.4003354610723));
#42226=CARTESIAN_POINT('Ctrl Pts',(-0.146111815181358,-2.28850520822416E-5,
-2.40158449541571));
#42227=CARTESIAN_POINT('Ctrl Pts',(-0.14612072978227,-4.38323123618543E-5,
-2.40871550458428));
#42228=CARTESIAN_POINT('Ctrl Pts',(-0.146178971007376,-0.0217877372618158,
-2.4075374971786));
#42229=CARTESIAN_POINT('Ctrl Pts',(-0.141636892583024,-0.0435085119960741,
-2.40635948977292));
#42230=CARTESIAN_POINT('Ctrl Pts',(-0.132371493453238,-0.0629819454103503,
-2.40518148236724));
#42231=CARTESIAN_POINT('Ctrl Pts',(-0.111535510698569,-0.106773704093438,
-2.40253238526459));
#42232=CARTESIAN_POINT('Ctrl Pts',(-0.0668133233245271,-0.139200480814385,
-2.39988328816194));
#42233=CARTESIAN_POINT('Ctrl Pts',(-0.0187141926056368,-0.145391597837813,
-2.39723419105929));
#42234=CARTESIAN_POINT('Ctrl Pts',(0.0293849381132521,-0.15158271486124,
-2.39458509395664));
#42235=CARTESIAN_POINT('Ctrl Pts',(0.0808610121769882,-0.131538172187151,
-2.39193599685399));
#42236=CARTESIAN_POINT('Ctrl Pts',(0.112107486293538,-0.0944502474515405,
-2.38928689975134));
#42237=CARTESIAN_POINT('Ctrl Pts',(0.143353960410089,-0.0573623227159294,
-2.38663780264869));
#42238=CARTESIAN_POINT('Ctrl Pts',(0.154370834579451,-0.00323101591879572,
-2.38398870554604));
#42239=CARTESIAN_POINT('Ctrl Pts',(0.140105852549527,0.0431194597378418,
-2.38133960844339));
#42240=CARTESIAN_POINT('Ctrl Pts',(0.125840870519603,0.0894699353944787,
-2.37869051134074));
#42241=CARTESIAN_POINT('Ctrl Pts',(0.0862940322903931,0.128039579910621,
-2.37604141423809));
#42242=CARTESIAN_POINT('Ctrl Pts',(0.0396012226530549,0.141140642237083,
-2.37339231713544));
#42243=CARTESIAN_POINT('Ctrl Pts',(-0.0070915869842839,0.154241704563545,
-2.37074322003279));
#42244=CARTESIAN_POINT('Ctrl Pts',(-0.0609303680297501,0.141874184700328,
-2.36809412293014));
#42245=CARTESIAN_POINT('Ctrl Pts',(-0.097225057407312,0.109709734932038,
-2.36544502582749));
#42246=CARTESIAN_POINT('Ctrl Pts',(-0.127958281309316,0.0824738705847656,
-2.36320185207975));
#42247=CARTESIAN_POINT('Ctrl Pts',(-0.146112075293418,0.0410432507012986,
-2.36095867833202));
#42248=CARTESIAN_POINT('Ctrl Pts',(-0.146465637571143,-0.000114315844697511,
-2.35871550458428));
#42249=CARTESIAN_POINT('Origin',(0.,0.,-1.487));
#42250=CARTESIAN_POINT('',(-0.146518717508966,9.11058135677975E-5,-2.30158449541571));
#42251=CARTESIAN_POINT('',(-0.146485691396121,0.00010691274947015,-2.30871550458428));
#42252=CARTESIAN_POINT('',(-0.14635,-1.79227059055215E-17,-1.487));
#42253=CARTESIAN_POINT('Ctrl Pts',(-0.146518717508966,9.11058135677975E-5,
-2.30158449541571));
#42254=CARTESIAN_POINT('Ctrl Pts',(-0.146558146874483,0.0055010752982445,
-2.30187962917383));
#42255=CARTESIAN_POINT('Ctrl Pts',(-0.146284538842059,0.0109070158290159,
-2.30217476293194));
#42256=CARTESIAN_POINT('Ctrl Pts',(-0.145684637283403,0.0162765014723047,
-2.30246989669006));
#42257=CARTESIAN_POINT('Ctrl Pts',(-0.140299968680779,0.0644725768758163,
-2.30511899379271));
#42258=CARTESIAN_POINT('Ctrl Pts',(-0.10862676192489,0.10973158603861,-2.30776809089536));
#42259=CARTESIAN_POINT('Ctrl Pts',(-0.0651901131906062,0.131298085221265,
-2.31041718799801));
#42260=CARTESIAN_POINT('Ctrl Pts',(-0.0217534644563208,0.152864584403921,
-2.31306628510066));
#42261=CARTESIAN_POINT('Ctrl Pts',(0.0334466262563611,0.150738573606437,
-2.31571538220332));
#42262=CARTESIAN_POINT('Ctrl Pts',(0.0750958094203205,0.125895025509674,
-2.31836447930597));
#42263=CARTESIAN_POINT('Ctrl Pts',(0.11674499258428,0.101051477412912,-2.32101357640862));
#42264=CARTESIAN_POINT('Ctrl Pts',(0.144843268199517,0.0534903920168709,
-2.32366267351127));
#42265=CARTESIAN_POINT('Ctrl Pts',(0.146504976825077,0.00502292803633103,
-2.32631177061392));
#42266=CARTESIAN_POINT('Ctrl Pts',(0.148166685450637,-0.0434445359442082,
-2.32896086771657));
#42267=CARTESIAN_POINT('Ctrl Pts',(0.123391827086521,-0.0928183785092465,
-2.33160996481922));
#42268=CARTESIAN_POINT('Ctrl Pts',(0.0835419668319325,-0.120456124038701,
-2.33425906192187));
#42269=CARTESIAN_POINT('Ctrl Pts',(0.0436921065773438,-0.148093869568155,
-2.33690815902452));
#42270=CARTESIAN_POINT('Ctrl Pts',(-0.0112327555677177,-0.153995518062025,
-2.33955725612717));
#42271=CARTESIAN_POINT('Ctrl Pts',(-0.0560444878426382,-0.135454617577368,
-2.34220635322982));
#42272=CARTESIAN_POINT('Ctrl Pts',(-0.100856220117559,-0.11691371709271,
-2.34485545033247));
#42273=CARTESIAN_POINT('Ctrl Pts',(-0.135554822522338,-0.0739302676295245,
-2.34750454743512));
#42274=CARTESIAN_POINT('Ctrl Pts',(-0.14422777502238,-0.0262161582362525,
-2.35015364453777));
#42275=CARTESIAN_POINT('Ctrl Pts',(-0.145789275817825,-0.0176255865974496,
-2.35063059483042));
#42276=CARTESIAN_POINT('Ctrl Pts',(-0.146507146511952,-0.00888166904295471,
-2.35110754512306));
#42277=CARTESIAN_POINT('Ctrl Pts',(-0.14642783004434,-0.00012476929814137,
-2.35158449541571));
#42278=CARTESIAN_POINT('Ctrl Pts',(-0.146465637571143,-0.000114315844697511,
-2.35871550458428));
#42279=CARTESIAN_POINT('Ctrl Pts',(-0.146529617985541,-0.00756216401491792,
-2.35830958122937));
#42280=CARTESIAN_POINT('Ctrl Pts',(-0.146010706652304,-0.0150010706983251,
-2.35790365787445));
#42281=CARTESIAN_POINT('Ctrl Pts',(-0.144877966401556,-0.0223453032662951,
-2.35749773451953));
#42282=CARTESIAN_POINT('Ctrl Pts',(-0.137485588308582,-0.0702745120229723,
-2.35484863741688));
#42283=CARTESIAN_POINT('Ctrl Pts',(-0.103950234412977,-0.114171549862962,
-2.35219954031423));
#42284=CARTESIAN_POINT('Ctrl Pts',(-0.0596509676667877,-0.13390556292824,
-2.34955044321158));
#42285=CARTESIAN_POINT('Ctrl Pts',(-0.0153517009205988,-0.153639575993518,
-2.34690134610893));
#42286=CARTESIAN_POINT('Ctrl Pts',(0.0397114786761746,-0.149210564284086,
-2.34425224900628));
#42287=CARTESIAN_POINT('Ctrl Pts',(0.0802870080121162,-0.122649639506912,
-2.34160315190363));
#42288=CARTESIAN_POINT('Ctrl Pts',(0.120862537348058,-0.096088714729738,
-2.33895405480098));
#42289=CARTESIAN_POINT('Ctrl Pts',(0.146950416423168,-0.0473958768848222,
-2.33630495769833));
#42290=CARTESIAN_POINT('Ctrl Pts',(0.146586938642,0.00109870208863794,-2.33365586059568));
#42291=CARTESIAN_POINT('Ctrl Pts',(0.146223460860833,0.0495932810620981,
-2.33100676349303));
#42292=CARTESIAN_POINT('Ctrl Pts',(0.119408626223387,0.0978896011641026,
-2.32835766639038));
#42293=CARTESIAN_POINT('Ctrl Pts',(0.0784395177192075,0.123839330532312,
-2.32570856928773));
#42294=CARTESIAN_POINT('Ctrl Pts',(0.0374704092150271,0.149789059900522,
-2.32305947218508));
#42295=CARTESIAN_POINT('Ctrl Pts',(-0.0176529731558879,0.153392198534936,
-2.32041037508243));
#42296=CARTESIAN_POINT('Ctrl Pts',(-0.0616514577393187,0.132996373955571,
-2.31776127797978));
#42297=CARTESIAN_POINT('Ctrl Pts',(-0.105649942322749,0.112600549376206,
-2.31511218087712));
#42298=CARTESIAN_POINT('Ctrl Pts',(-0.138523529118695,0.0682057615830633,
-2.31246308377448));
#42299=CARTESIAN_POINT('Ctrl Pts',(-0.145196636626864,0.0201711288469323,
-2.30981398667183));
#42300=CARTESIAN_POINT('Ctrl Pts',(-0.146118999829862,0.0135317366820221,
-2.30944782597598));
#42301=CARTESIAN_POINT('Ctrl Pts',(-0.146540802124392,0.00682280517505123,
-2.30908166528013));
#42302=CARTESIAN_POINT('Ctrl Pts',(-0.146485691396121,0.00010691274947015,
-2.30871550458428));
#42303=CARTESIAN_POINT('Origin',(0.,0.,-1.487));
#42304=CARTESIAN_POINT('',(-0.14614553911452,7.41235706846755E-5,-2.25158449541571));
#42305=CARTESIAN_POINT('',(-0.146128142350211,5.51125628420172E-5,-2.25871550458428));
#42306=CARTESIAN_POINT('',(-0.14635,-1.79227059055215E-17,-1.487));
#42307=CARTESIAN_POINT('Ctrl Pts',(-0.14614553911452,7.41235706846755E-5,
-2.25158449541571));
#42308=CARTESIAN_POINT('Ctrl Pts',(-0.146235642754429,0.0197646966306404,
-2.25265171322459));
#42309=CARTESIAN_POINT('Ctrl Pts',(-0.142535886262011,0.039422814349067,
-2.25371893103347));
#42310=CARTESIAN_POINT('Ctrl Pts',(-0.134885835946401,0.0573999068084199,
-2.25478614884235));
#42311=CARTESIAN_POINT('Ctrl Pts',(-0.115896529398507,0.102023472074894,
-2.257435245945));
#42312=CARTESIAN_POINT('Ctrl Pts',(-0.0725673095232115,0.13628932448801,
-2.26008434304765));
#42313=CARTESIAN_POINT('Ctrl Pts',(-0.0247686330987405,0.144483399928831,
-2.2627334401503));
#42314=CARTESIAN_POINT('Ctrl Pts',(0.0230300433257305,0.152677475369652,
-2.26538253725296));
#42315=CARTESIAN_POINT('Ctrl Pts',(0.0752981762993759,0.134799773838178,
-2.2680316343556));
#42316=CARTESIAN_POINT('Ctrl Pts',(0.108065990226868,0.0990488757980672,
-2.27068073145825));
#42317=CARTESIAN_POINT('Ctrl Pts',(0.140833804154361,0.0632979777579564,
-2.2733298285609));
#42318=CARTESIAN_POINT('Ctrl Pts',(0.1541012990357,0.00967388320920951,
-2.27597892566356));
#42319=CARTESIAN_POINT('Ctrl Pts',(0.141784100761364,-0.0372317983968804,
-2.27862802276621));
#42320=CARTESIAN_POINT('Ctrl Pts',(0.129466902487028,-0.0841374800029696,
-2.28127711986886));
#42321=CARTESIAN_POINT('Ctrl Pts',(0.0915650110570157,-0.124324748666403,
-2.28392621697151));
#42322=CARTESIAN_POINT('Ctrl Pts',(0.0454599509400524,-0.139364022979758,
-2.28657531407416));
#42323=CARTESIAN_POINT('Ctrl Pts',(-0.000645109176910887,-0.154403297293113,
-2.28922441117681));
#42324=CARTESIAN_POINT('Ctrl Pts',(-0.0549533379808256,-0.144294577256392,
-2.29187350827946));
#42325=CARTESIAN_POINT('Ctrl Pts',(-0.0925593871581046,-0.113673646415916,
-2.29452260538211));
#42326=CARTESIAN_POINT('Ctrl Pts',(-0.125975776918769,-0.0864641686274881,
-2.29687656872664));
#42327=CARTESIAN_POINT('Ctrl Pts',(-0.146204232030531,-0.043058379840643,
-2.29923053207118));
#42328=CARTESIAN_POINT('Ctrl Pts',(-0.146518717508966,9.11058135677975E-5,
-2.30158449541571));
#42329=CARTESIAN_POINT('Ctrl Pts',(-0.146485691396121,0.00010691274947015,
-2.30871550458428));
#42330=CARTESIAN_POINT('Ctrl Pts',(-0.146142087373619,-0.0417652911665238,
-2.30643256817748));
#42331=CARTESIAN_POINT('Ctrl Pts',(-0.127259609035765,-0.0839080844543,
-2.30414963177068));
#42332=CARTESIAN_POINT('Ctrl Pts',(-0.0955696282125509,-0.111154774481476,
-2.30186669536387));
#42333=CARTESIAN_POINT('Ctrl Pts',(-0.0587968840696793,-0.142771567394633,
-2.29921759826122));
#42334=CARTESIAN_POINT('Ctrl Pts',(-0.00477876756354516,-0.154330675541829,
-2.29656850115857));
#42335=CARTESIAN_POINT('Ctrl Pts',(0.0417124163263103,-0.140531178216557,
-2.29391940405592));
#42336=CARTESIAN_POINT('Ctrl Pts',(0.0882036002161671,-0.126731680891284,
-2.29127030695327));
#42337=CARTESIAN_POINT('Ctrl Pts',(0.127167851489746,-0.0875735780935426,
-2.28862120985062));
#42338=CARTESIAN_POINT('Ctrl Pts',(0.140736455384675,-0.0410144834475642,
-2.28597211274797));
#42339=CARTESIAN_POINT('Ctrl Pts',(0.154305059279604,0.005544611198413,
-2.28332301564532));
#42340=CARTESIAN_POINT('Ctrl Pts',(0.142478015795887,0.0595046976926254,
-2.28067391854267));
#42341=CARTESIAN_POINT('Ctrl Pts',(0.110679118785195,0.096120083185803,
-2.27802482144002));
#42342=CARTESIAN_POINT('Ctrl Pts',(0.0788802217745042,0.132735468678981,
-2.27537572433737));
#42343=CARTESIAN_POINT('Ctrl Pts',(0.0271094712368389,0.152006153171122,
-2.27272662723472));
#42344=CARTESIAN_POINT('Ctrl Pts',(-0.0208914531046072,0.145094744611551,
-2.27007753013207));
#42345=CARTESIAN_POINT('Ctrl Pts',(-0.0688923774460532,0.138183336051979,
-2.26742843302942));
#42346=CARTESIAN_POINT('Ctrl Pts',(-0.113123475591281,0.105089834440694,
-2.26477933592677));
#42347=CARTESIAN_POINT('Ctrl Pts',(-0.133300696120074,0.0609906725706206,
-2.26213023882412));
#42348=CARTESIAN_POINT('Ctrl Pts',(-0.141970297262714,0.0420424659237912,
-2.26099199407751));
#42349=CARTESIAN_POINT('Ctrl Pts',(-0.146199104167309,0.0210624092175888,
-2.25985374933089));
#42350=CARTESIAN_POINT('Ctrl Pts',(-0.146128142350211,5.51125628420172E-5,
-2.25871550458428));
#42351=CARTESIAN_POINT('Origin',(0.,0.,-1.487));
#42352=CARTESIAN_POINT('',(-0.146247143544926,-0.000124102100222137,-2.20158449541571));
#42353=CARTESIAN_POINT('',(-0.146283306677627,-0.000130979094668964,-2.20871550458428));
#42354=CARTESIAN_POINT('',(-0.14635,-1.79227059055215E-17,-1.487));
#42355=CARTESIAN_POINT('Ctrl Pts',(-0.146247143544926,-0.000124102100222137,
-2.20158449541571));
#42356=CARTESIAN_POINT('Ctrl Pts',(-0.145975220405292,0.0337524727000206,
-2.20342379727535));
#42357=CARTESIAN_POINT('Ctrl Pts',(-0.13426106438023,0.0677987052486075,
-2.205263099135));
#42358=CARTESIAN_POINT('Ctrl Pts',(-0.112739815984817,0.0936945672506367,
-2.20710240099464));
#42359=CARTESIAN_POINT('Ctrl Pts',(-0.081743339538734,0.130991682262237,
-2.20975149809729));
#42360=CARTESIAN_POINT('Ctrl Pts',(-0.0304031603579323,0.151381776383703,
-2.21240059519994));
#42361=CARTESIAN_POINT('Ctrl Pts',(0.0177364986444008,0.145514104664846,
-2.21504969230259));
#42362=CARTESIAN_POINT('Ctrl Pts',(0.0658761576467332,0.139646432945988,
-2.21769878940525));
#42363=CARTESIAN_POINT('Ctrl Pts',(0.110815296470595,0.107520995386807,
-2.2203478865079));
#42364=CARTESIAN_POINT('Ctrl Pts',(0.131945161526139,0.0638702778326173,
-2.22299698361055));
#42365=CARTESIAN_POINT('Ctrl Pts',(0.153075026581682,0.0202195602784276,
-2.2256460807132));
#42366=CARTESIAN_POINT('Ctrl Pts',(0.150395617868907,-0.0349564372707706,
-2.22829517781585));
#42367=CARTESIAN_POINT('Ctrl Pts',(0.125135692221462,-0.0763544142327749,
-2.2309442749185));
#42368=CARTESIAN_POINT('Ctrl Pts',(0.099875766574016,-0.11775239119478,
-2.23359337202115));
#42369=CARTESIAN_POINT('Ctrl Pts',(0.0520353239918985,-0.145372347569591,
-2.2362424691238));
#42370=CARTESIAN_POINT('Ctrl Pts',(0.00355363430999713,-0.146547977549216,
-2.23889156622645));
#42371=CARTESIAN_POINT('Ctrl Pts',(-0.0449280553719036,-0.14772360752884,
-2.2415406633291));
#42372=CARTESIAN_POINT('Ctrl Pts',(-0.094050992153589,-0.12245491111328,
-2.24418976043175));
#42373=CARTESIAN_POINT('Ctrl Pts',(-0.121287763934186,-0.0823299238455837,
-2.2468388575344));
#42374=CARTESIAN_POINT('Ctrl Pts',(-0.137551903616247,-0.0583697275741744,
-2.24842073682817));
#42375=CARTESIAN_POINT('Ctrl Pts',(-0.146011983357597,-0.0291121489472482,
-2.25000261612194));
#42376=CARTESIAN_POINT('Ctrl Pts',(-0.14614553911452,7.41235706846755E-5,
-2.25158449541571));
#42377=CARTESIAN_POINT('Ctrl Pts',(-0.146128142350211,5.51125628420172E-5,
-2.25871550458428));
#42378=CARTESIAN_POINT('Ctrl Pts',(-0.14603395098331,-0.0278289815560796,
-2.25720465222824));
#42379=CARTESIAN_POINT('Ctrl Pts',(-0.138364145592754,-0.0557610687996438,
-2.2556937998722));
#42380=CARTESIAN_POINT('Ctrl Pts',(-0.123448530857947,-0.0790531337502038,
-2.25418294751616));
#42381=CARTESIAN_POINT('Ctrl Pts',(-0.0972958021546651,-0.11989295607209,
-2.25153385041351));
#42382=CARTESIAN_POINT('Ctrl Pts',(-0.0488670018357426,-0.146467778586996,
-2.24888475331086));
#42383=CARTESIAN_POINT('Ctrl Pts',(-0.000371216202019402,-0.146590586073064,
-2.24623565620821));
#42384=CARTESIAN_POINT('Ctrl Pts',(0.0481245694317025,-0.146713393559132,
-2.24358655910556));
#42385=CARTESIAN_POINT('Ctrl Pts',(0.0966873403802246,-0.120384186016363,
-2.24093746200291));
#42386=CARTESIAN_POINT('Ctrl Pts',(0.123046572412074,-0.0796773414739313,
-2.23828836490026));
#42387=CARTESIAN_POINT('Ctrl Pts',(0.149405804443923,-0.0389704969314992,
-2.23563926779761));
#42388=CARTESIAN_POINT('Ctrl Pts',(0.153561497559099,0.0161139846105963,
-2.23299017069496));
#42389=CARTESIAN_POINT('Ctrl Pts',(0.133607881917611,0.0603147711278332,
-2.23034107359231));
#42390=CARTESIAN_POINT('Ctrl Pts',(0.113654266276122,0.10451555764507,-2.22769197648966));
#42391=CARTESIAN_POINT('Ctrl Pts',(0.0695913418779708,0.137832649137449,
-2.22504287938701));
#42392=CARTESIAN_POINT('Ctrl Pts',(0.0216260369183928,0.144987076161696,
-2.22239378228436));
#42393=CARTESIAN_POINT('Ctrl Pts',(-0.0263392680411845,0.152141503185943,
-2.21974468518171));
#42394=CARTESIAN_POINT('Ctrl Pts',(-0.0782069535621885,0.133133265742058,
-2.21709558807905));
#42395=CARTESIAN_POINT('Ctrl Pts',(-0.110190886261694,0.0966793996235781,
-2.2144464909764));
#42396=CARTESIAN_POINT('Ctrl Pts',(-0.133255283421017,0.0703916240067169,
-2.21253616217903));
#42397=CARTESIAN_POINT('Ctrl Pts',(-0.145979720895302,0.0350317633164389,
-2.21062583338166));
#42398=CARTESIAN_POINT('Ctrl Pts',(-0.146283306677627,-0.000130979094668964,
-2.20871550458428));
#42399=CARTESIAN_POINT('Origin',(0.,0.,-1.487));
#42400=CARTESIAN_POINT('',(-0.146589640615231,-1.29382981380044E-5,-2.15158449541571));
#42401=CARTESIAN_POINT('',(-0.146589947336248,1.14350527840421E-5,-2.15871550458428));
#42402=CARTESIAN_POINT('',(-0.14635,-1.79227059055215E-17,-1.487));
#42403=CARTESIAN_POINT('Ctrl Pts',(-0.146589640615231,-1.29382981380044E-5,
-2.15158449541571));
#42404=CARTESIAN_POINT('Ctrl Pts',(-0.146529298073255,0.0477938860680167,
-2.15419588132612));
#42405=CARTESIAN_POINT('Ctrl Pts',(-0.120930624581389,0.0956561308620035,
-2.15680726723653));
#42406=CARTESIAN_POINT('Ctrl Pts',(-0.0811096027371204,0.122107208568541,
-2.15941865314693));
#42407=CARTESIAN_POINT('Ctrl Pts',(-0.0407135229498382,0.148940267993073,
-2.16206775024958));
#42408=CARTESIAN_POINT('Ctrl Pts',(0.0143186428785755,0.153739295064571,
-2.16471684735223));
#42409=CARTESIAN_POINT('Ctrl Pts',(0.0587495543193546,0.134303491793221,
-2.16736594445488));
#42410=CARTESIAN_POINT('Ctrl Pts',(0.103180465760136,0.114867688521869,
-2.17001504155753));
#42411=CARTESIAN_POINT('Ctrl Pts',(0.137010122813282,0.0711970549076663,
-2.17266413866019));
#42412=CARTESIAN_POINT('Ctrl Pts',(0.144724497295698,0.0233186175208184,
-2.17531323576284));
#42413=CARTESIAN_POINT('Ctrl Pts',(0.152438871778113,-0.0245598198660281,
-2.17796233286549));
#42414=CARTESIAN_POINT('Ctrl Pts',(0.1340379636898,-0.0766460610255191,
-2.18061142996814));
#42415=CARTESIAN_POINT('Ctrl Pts',(0.0979602921155994,-0.109053744590459,
-2.18326052707079));
#42416=CARTESIAN_POINT('Ctrl Pts',(0.0618826205413989,-0.141461428155398,
-2.18590962417344));
#42417=CARTESIAN_POINT('Ctrl Pts',(0.00812818548131124,-0.154190554125787,
-2.18855872127609));
#42418=CARTESIAN_POINT('Ctrl Pts',(-0.0386516304278741,-0.141403640355691,
-2.19120781837874));
#42419=CARTESIAN_POINT('Ctrl Pts',(-0.0854314463370593,-0.128616726585596,
-2.19385691548139));
#42420=CARTESIAN_POINT('Ctrl Pts',(-0.125236643095342,-0.0903137730750164,
-2.19650601258404));
#42421=CARTESIAN_POINT('Ctrl Pts',(-0.139812854618803,-0.0440602283688595,
-2.19915510968669));
#42422=CARTESIAN_POINT('Ctrl Pts',(-0.144268616825835,-0.0299211088787746,
-2.1999649049297));
#42423=CARTESIAN_POINT('Ctrl Pts',(-0.146366864005047,-0.0150390487571437,
-2.2007747001727));
#42424=CARTESIAN_POINT('Ctrl Pts',(-0.146247143544926,-0.000124102100222137,
-2.20158449541571));
#42425=CARTESIAN_POINT('Ctrl Pts',(-0.146283306677627,-0.000130979094668964,
-2.20871550458428));
#42426=CARTESIAN_POINT('Ctrl Pts',(-0.146400710317368,-0.013729224410152,
-2.20797673627901));
#42427=CARTESIAN_POINT('Ctrl Pts',(-0.14466051635752,-0.0272979897470232,
-2.20723796797373));
#42428=CARTESIAN_POINT('Ctrl Pts',(-0.140942373732611,-0.040301178808194,
-2.20649919966845));
#42429=CARTESIAN_POINT('Ctrl Pts',(-0.127609748626014,-0.0869283963284094,
-2.2038501025658));
#42430=CARTESIAN_POINT('Ctrl Pts',(-0.088844318534813,-0.126283336575766,
-2.20120100546315));
#42431=CARTESIAN_POINT('Ctrl Pts',(-0.0424236203113571,-0.140318117741049,
-2.1985519083605));
#42432=CARTESIAN_POINT('Ctrl Pts',(0.00399707791210018,-0.154352898906332,
-2.19590281125785));
#42433=CARTESIAN_POINT('Ctrl Pts',(0.0580730442678115,-0.14306752098954,
-2.1932537141552));
#42434=CARTESIAN_POINT('Ctrl Pts',(0.0950054442670761,-0.111637374056938,
-2.19060461705255));
#42435=CARTESIAN_POINT('Ctrl Pts',(0.13193784426634,-0.0802072271243357,
-2.1879555199499));
#42436=CARTESIAN_POINT('Ctrl Pts',(0.151726677909156,-0.0286323111759234,
-2.18530642284725));
#42437=CARTESIAN_POINT('Ctrl Pts',(0.145296933812379,0.0194355023458139,
-2.1826573257446));
#42438=CARTESIAN_POINT('Ctrl Pts',(0.138867189715603,0.0675033158675512,
-2.18000822864195));
#42439=CARTESIAN_POINT('Ctrl Pts',(0.106218867879233,0.112064026962615,
-2.1773591315393));
#42440=CARTESIAN_POINT('Ctrl Pts',(0.0623242449747267,0.132682426172585,
-2.17471003443665));
#42441=CARTESIAN_POINT('Ctrl Pts',(0.0184296220702193,0.153300825382555,
-2.172060937334));
#42442=CARTESIAN_POINT('Ctrl Pts',(-0.0367113019024245,0.149976912707432,
-2.16941184023135));
#42443=CARTESIAN_POINT('Ctrl Pts',(-0.0778113108413852,0.124235009686716,
-2.1667627431287));
#42444=CARTESIAN_POINT('Ctrl Pts',(-0.118911319780345,0.0984931066660002,
-2.16411364602605));
#42445=CARTESIAN_POINT('Ctrl Pts',(-0.145970413685621,0.0503332132996906,
-2.16146454892339));
#42446=CARTESIAN_POINT('Ctrl Pts',(-0.14657949409086,0.00184109716757596,
-2.15881545182074));
#42447=CARTESIAN_POINT('Ctrl Pts',(-0.146587154047055,0.00123124749556039,
-2.15878213607526));
#42448=CARTESIAN_POINT('Ctrl Pts',(-0.146590630604965,0.000621345278386432,
-2.15874882032977));
#42449=CARTESIAN_POINT('Ctrl Pts',(-0.146589947336248,1.14350527840421E-5,
-2.15871550458428));
#42450=CARTESIAN_POINT('Origin',(0.,0.,-1.487));
#42451=CARTESIAN_POINT('',(-0.146285624387341,0.00013129064497696,-2.10158449541571));
#42452=CARTESIAN_POINT('',(-0.146249303190328,0.000124626032094787,-2.10871550458428));
#42453=CARTESIAN_POINT('',(-0.14635,-1.79227059055215E-17,-1.487));
#42454=CARTESIAN_POINT('Ctrl Pts',(-0.146285624387341,0.00013129064497696,
-2.10158449541571));
#42455=CARTESIAN_POINT('Ctrl Pts',(-0.146402750591997,0.0136480875377478,
-2.10231886827423));
#42456=CARTESIAN_POINT('Ctrl Pts',(-0.144683559179741,0.0271356452517675,
-2.10305324113275));
#42457=CARTESIAN_POINT('Ctrl Pts',(-0.141008962074582,0.0400675761086641,
-2.10378761399127));
#42458=CARTESIAN_POINT('Ctrl Pts',(-0.12775361850934,0.0867168226966701,
-2.10643671109392));
#42459=CARTESIAN_POINT('Ctrl Pts',(-0.0890534542095754,0.126135945210629,
-2.10908580819657));
#42460=CARTESIAN_POINT('Ctrl Pts',(-0.0426560756228998,0.140247628332988,
-2.11173490529922));
#42461=CARTESIAN_POINT('Ctrl Pts',(0.0037413029637753,0.154359311455347,
-2.11438400240188));
#42462=CARTESIAN_POINT('Ctrl Pts',(0.0578358958373609,0.143163555186107,
-2.11703309950452));
#42463=CARTESIAN_POINT('Ctrl Pts',(0.0948203265271063,0.111794649772999,
-2.11968219660717));
#42464=CARTESIAN_POINT('Ctrl Pts',(0.131804757216852,0.0804257443598906,
-2.12233129370982));
#42465=CARTESIAN_POINT('Ctrl Pts',(0.151679025722757,0.0288836898029136,
-2.12498039081248));
#42466=CARTESIAN_POINT('Ctrl Pts',(0.145328940871243,-0.0191947124442461,
-2.12762948791513));
#42467=CARTESIAN_POINT('Ctrl Pts',(0.138978856019729,-0.0672731146914066,
-2.13027858501778));
#42468=CARTESIAN_POINT('Ctrl Pts',(0.106404417810795,-0.11188786462875,
-2.13292768212043));
#42469=CARTESIAN_POINT('Ctrl Pts',(0.0625440204359034,-0.132578970988192,
-2.13557677922308));
#42470=CARTESIAN_POINT('Ctrl Pts',(0.0186836230610119,-0.153270077347634,
-2.13822587632573));
#42471=CARTESIAN_POINT('Ctrl Pts',(-0.0364627334798375,-0.150037540129176,
-2.14087497342838));
#42472=CARTESIAN_POINT('Ctrl Pts',(-0.0776053417495988,-0.124363776770017,
-2.14352407053103));
#42473=CARTESIAN_POINT('Ctrl Pts',(-0.118747950019361,-0.0986900134108574,
-2.14617316763368));
#42474=CARTESIAN_POINT('Ctrl Pts',(-0.145886810018034,-0.0505750239109964,
-2.14882226473633));
#42475=CARTESIAN_POINT('Ctrl Pts',(-0.146576243144295,-0.00208398327228049,
-2.15147136183898));
#42476=CARTESIAN_POINT('Ctrl Pts',(-0.14658605756187,-0.00139368960439911,
-2.15150907303122));
#42477=CARTESIAN_POINT('Ctrl Pts',(-0.146590512025769,-0.000703319730076893,
-2.15154678422347));
#42478=CARTESIAN_POINT('Ctrl Pts',(-0.146589640615231,-1.29382981380044E-5,
-2.15158449541571));
#42479=CARTESIAN_POINT('Ctrl Pts',(-0.146589947336248,1.14350527840421E-5,
-2.15871550458428));
#42480=CARTESIAN_POINT('Ctrl Pts',(-0.146536300583162,-0.0478755857641898,
-2.15609972322712));
#42481=CARTESIAN_POINT('Ctrl Pts',(-0.12083905113848,-0.0958119752148835,
-2.15348394186996));
#42482=CARTESIAN_POINT('Ctrl Pts',(-0.0809071538188127,-0.12224144218575,
-2.15086816051279));
#42483=CARTESIAN_POINT('Ctrl Pts',(-0.0404666662363262,-0.149007526509037,
-2.14821906341014));
#42484=CARTESIAN_POINT('Ctrl Pts',(0.0145733758338476,-0.153715356257692,
-2.14556996630749));
#42485=CARTESIAN_POINT('Ctrl Pts',(0.0589720199772672,-0.13420595585336,
-2.14292086920484));
#42486=CARTESIAN_POINT('Ctrl Pts',(0.103370664120688,-0.114696555449027,
-2.14027177210219));
#42487=CARTESIAN_POINT('Ctrl Pts',(0.137127910337354,-0.070969924891706,
-2.13762267499954));
#42488=CARTESIAN_POINT('Ctrl Pts',(0.144762937513227,-0.0230787705316953,
-2.13497357789689));
#42489=CARTESIAN_POINT('Ctrl Pts',(0.152397964689099,0.0248123838283127,
-2.13232448079424));
#42490=CARTESIAN_POINT('Ctrl Pts',(0.133910772824182,0.0768680619910102,
-2.12967538369159));
#42491=CARTESIAN_POINT('Ctrl Pts',(0.0977794500991502,0.109215918551376,
-2.12702628658894));
#42492=CARTESIAN_POINT('Ctrl Pts',(0.0616481273741167,0.141563775111744,
-2.12437718948629));
#42493=CARTESIAN_POINT('Ctrl Pts',(0.00787267378896704,0.154203810069778,
-2.12172809238364));
#42494=CARTESIAN_POINT('Ctrl Pts',(-0.0388858890808203,0.14133939775274,
-2.11907899528099));
#42495=CARTESIAN_POINT('Ctrl Pts',(-0.0856444519506078,0.128474985435702,
-2.11642989817834));
#42496=CARTESIAN_POINT('Ctrl Pts',(-0.125386124105033,0.0901061258435907,
-2.11378080107569));
#42497=CARTESIAN_POINT('Ctrl Pts',(-0.139885671369288,0.0438284915583091,
-2.11113170397303));
#42498=CARTESIAN_POINT('Ctrl Pts',(-0.144293940285014,0.0297587931742726,
-2.11032630417678));
#42499=CARTESIAN_POINT('Ctrl Pts',(-0.146369002652299,0.0149580626372562,
-2.10952090438053));
#42500=CARTESIAN_POINT('Ctrl Pts',(-0.146249303190328,0.000124626032094787,
-2.10871550458428));
#42501=CARTESIAN_POINT('Origin',(0.,0.,-1.487));
#42502=CARTESIAN_POINT('',(-0.146127240320273,-5.3885368266407E-5,-2.05158449541571));
#42503=CARTESIAN_POINT('',(-0.146144311576588,-7.2996660745207E-5,-2.05871550458428));
#42504=CARTESIAN_POINT('',(-0.14635,-1.79227059055215E-17,-1.487));
#42505=CARTESIAN_POINT('Ctrl Pts',(-0.146127240320273,-5.3885368266407E-5,
-2.05158449541571));
#42506=CARTESIAN_POINT('Ctrl Pts',(-0.14603544661587,0.0277495163116801,
-2.05309095232499));
#42507=CARTESIAN_POINT('Ctrl Pts',(-0.138413074264927,0.0555995514695339,
-2.05459740923428));
#42508=CARTESIAN_POINT('Ctrl Pts',(-0.123579356770016,0.078848466192334,
-2.05610386614356));
#42509=CARTESIAN_POINT('Ctrl Pts',(-0.0974943371487333,0.119731568956415,
-2.05875296324621));
#42510=CARTESIAN_POINT('Ctrl Pts',(-0.0491096386046498,0.146386603816594,
-2.06140206034886));
#42511=CARTESIAN_POINT('Ctrl Pts',(-0.000614122693888632,0.146589770768261,
-2.06405115745151));
#42512=CARTESIAN_POINT('Ctrl Pts',(0.0478813932168725,0.146792937719929,
-2.06670025455416));
#42513=CARTESIAN_POINT('Ctrl Pts',(0.0964877264943104,0.120544236763086,
-2.06934935165682));
#42514=CARTESIAN_POINT('Ctrl Pts',(0.12291437554811,0.0798811262075896,
-2.07199844875947));
#42515=CARTESIAN_POINT('Ctrl Pts',(0.149341024601909,0.0392180156520937,
-2.07464754586212));
#42516=CARTESIAN_POINT('Ctrl Pts',(0.153587989432068,-0.0158595045020563,
-2.07729664296477));
#42517=CARTESIAN_POINT('Ctrl Pts',(0.133707643671456,-0.0600932946708818,
-2.07994574006742));
#42518=CARTESIAN_POINT('Ctrl Pts',(0.113827297910845,-0.104327084839708,
-2.08259483717007));
#42519=CARTESIAN_POINT('Ctrl Pts',(0.0698196415594624,-0.13771714502321,
-2.08524393427272));
#42520=CARTESIAN_POINT('Ctrl Pts',(0.0218662572988801,-0.144951042881084,
-2.08789303137537));
#42521=CARTESIAN_POINT('Ctrl Pts',(-0.0260871269617016,-0.152184940738957,
-2.09054212847802));
#42522=CARTESIAN_POINT('Ctrl Pts',(-0.0779862391314823,-0.133262676271201,
-2.09319122558067));
#42523=CARTESIAN_POINT('Ctrl Pts',(-0.110030533801013,-0.0968618587062973,
-2.09584032268332));
#42524=CARTESIAN_POINT('Ctrl Pts',(-0.133191628133265,-0.0705519405730871,
-2.09775504692745));
#42525=CARTESIAN_POINT('Ctrl Pts',(-0.145980242208416,-0.0351109414354531,
-2.09966977117158));
#42526=CARTESIAN_POINT('Ctrl Pts',(-0.146285624387341,0.00013129064497696,
-2.10158449541571));
#42527=CARTESIAN_POINT('Ctrl Pts',(-0.146249303190328,0.000124626032094787,
-2.10871550458428));
#42528=CARTESIAN_POINT('Ctrl Pts',(-0.145975290735094,-0.0338316367344376,
-2.10687180727788));
#42529=CARTESIAN_POINT('Ctrl Pts',(-0.134200066247532,-0.067959289133989,
-2.10502810997148));
#42530=CARTESIAN_POINT('Ctrl Pts',(-0.112584404396465,-0.0938812527260169,
-2.10318441266508));
#42531=CARTESIAN_POINT('Ctrl Pts',(-0.0815261677853019,-0.131126953746614,
-2.10053531556243));
#42532=CARTESIAN_POINT('Ctrl Pts',(-0.0301522721888892,-0.151431946809354,
-2.09788621845978));
#42533=CARTESIAN_POINT('Ctrl Pts',(0.0179775973830789,-0.145484513674291,
-2.09523712135713));
#42534=CARTESIAN_POINT('Ctrl Pts',(0.0661074669550455,-0.139537080539229,
-2.09258802425448));
#42535=CARTESIAN_POINT('Ctrl Pts',(0.110993310502568,-0.107337221206366,
-2.08993892715183));
#42536=CARTESIAN_POINT('Ctrl Pts',(0.132050815251673,-0.0636515507908622,
-2.08728983004918));
#42537=CARTESIAN_POINT('Ctrl Pts',(0.153108320000778,-0.0199658803753582,
-2.08464073294653));
#42538=CARTESIAN_POINT('Ctrl Pts',(0.150337485951465,0.0352056011227862,
-2.08199163584388));
#42539=CARTESIAN_POINT('Ctrl Pts',(0.12500899691422,0.076561664148669,-2.07934253874123));
#42540=CARTESIAN_POINT('Ctrl Pts',(0.0996805078769755,0.117917727174551,
-2.07669344163858));
#42541=CARTESIAN_POINT('Ctrl Pts',(0.0517943638517992,0.145458371728172,
-2.07404434453593));
#42542=CARTESIAN_POINT('Ctrl Pts',(0.00331079301419913,0.146553663810668,
-2.07139524743328));
#42543=CARTESIAN_POINT('Ctrl Pts',(-0.045172777823401,0.147648955893163,
-2.06874615033063));
#42544=CARTESIAN_POINT('Ctrl Pts',(-0.0942537754734231,0.122298895504535,
-2.06609705322797));
#42545=CARTESIAN_POINT('Ctrl Pts',(-0.1214240208077,0.0821288310984904,
-2.06344795612532));
#42546=CARTESIAN_POINT('Ctrl Pts',(-0.137603353415531,0.0582083686621983,
-2.06187047227831));
#42547=CARTESIAN_POINT('Ctrl Pts',(-0.146013216347422,0.0290327890053112,
-2.0602929884313));
#42548=CARTESIAN_POINT('Ctrl Pts',(-0.146144311576588,-7.2996660745207E-5,
-2.05871550458428));
#42549=CARTESIAN_POINT('Origin',(0.,0.,-1.487));
#42550=CARTESIAN_POINT('',(-0.146483524170368,-0.000107783910021919,-2.00158449541571));
#42551=CARTESIAN_POINT('',(-0.14651679492655,-9.2174979582009E-5,-2.00871550458428));
#42552=CARTESIAN_POINT('',(-0.14635,-1.79227059055215E-17,-1.487));
#42553=CARTESIAN_POINT('Ctrl Pts',(-0.146483524170368,-0.000107783910021919,
-2.00158449541571));
#42554=CARTESIAN_POINT('Ctrl Pts',(-0.146138605468356,0.0416854145126164,
-2.00386303637576));
#42555=CARTESIAN_POINT('Ctrl Pts',(-0.127337547382231,0.0837496555319783,
-2.0061415773358));
#42556=CARTESIAN_POINT('Ctrl Pts',(-0.0957536860156155,0.110996259644177,
-2.00842011829585));
#42557=CARTESIAN_POINT('Ctrl Pts',(-0.0590333824951295,0.142673943423525,
-2.0110692153985));
#42558=CARTESIAN_POINT('Ctrl Pts',(-0.00503449370253807,0.154322546162233,
-2.01371831250115));
#42559=CARTESIAN_POINT('Ctrl Pts',(0.0414794930685156,0.140600105602213,
-2.0163674096038));
#42560=CARTESIAN_POINT('Ctrl Pts',(0.0879934798395713,0.126877665042193,
-2.01901650670646));
#42561=CARTESIAN_POINT('Ctrl Pts',(0.127022564589087,0.0877841811834399,
-2.0216656038091));
#42562=CARTESIAN_POINT('Ctrl Pts',(0.140668300406616,0.041247633887154,
-2.02431470091175));
#42563=CARTESIAN_POINT('Ctrl Pts',(0.154314036224144,-0.00528891340913192,
-2.02696379801441));
#42564=CARTESIAN_POINT('Ctrl Pts',(0.142576423109686,-0.0592685241429521,
-2.02961289511706));
#42565=CARTESIAN_POINT('Ctrl Pts',(0.110838242815177,-0.0959365517944979,
-2.03226199221971));
#42566=CARTESIAN_POINT('Ctrl Pts',(0.0791000625206695,-0.132604579446043,
-2.03491108932236));
#42567=CARTESIAN_POINT('Ctrl Pts',(0.0273613150461139,-0.151961024015315,
-2.03756018642501));
#42568=CARTESIAN_POINT('Ctrl Pts',(-0.0206509962511345,-0.145129164520472,
-2.04020928352766));
#42569=CARTESIAN_POINT('Ctrl Pts',(-0.0686633075483823,-0.138297305025629,
-2.04285838063031));
#42570=CARTESIAN_POINT('Ctrl Pts',(-0.112949182668323,-0.105277141466672,
-2.04550747773296));
#42571=CARTESIAN_POINT('Ctrl Pts',(-0.133199449879051,-0.0612114743532014,
-2.04815657483561));
#42572=CARTESIAN_POINT('Ctrl Pts',(-0.141934036926929,-0.0422045446559245,
-2.04929921502898));
#42573=CARTESIAN_POINT('Ctrl Pts',(-0.146196865395841,-0.0211426294777117,
-2.05044185522234));
#42574=CARTESIAN_POINT('Ctrl Pts',(-0.146127240320273,-5.3885368266407E-5,
-2.05158449541571));
#42575=CARTESIAN_POINT('Ctrl Pts',(-0.146144311576588,-7.2996660745207E-5,
-2.05871550458428));
#42576=CARTESIAN_POINT('Ctrl Pts',(-0.146233366932427,-0.0198450823112631,
-2.05764389132865));
#42577=CARTESIAN_POINT('Ctrl Pts',(-0.142501994378041,-0.0395849599182529,
-2.05657227807301));
#42578=CARTESIAN_POINT('Ctrl Pts',(-0.134790535627584,-0.057623339298778,
-2.05550066481737));
#42579=CARTESIAN_POINT('Ctrl Pts',(-0.115727312094663,-0.102215376866536,
-2.05285156771472));
#42580=CARTESIAN_POINT('Ctrl Pts',(-0.0723413720102935,-0.136409383578594,
-2.05020247061207));
#42581=CARTESIAN_POINT('Ctrl Pts',(-0.0245291836171625,-0.144524243218183,
-2.04755337350942));
#42582=CARTESIAN_POINT('Ctrl Pts',(0.0232830047759706,-0.152639102857773,
-2.04490427640677));
#42583=CARTESIAN_POINT('Ctrl Pts',(0.0755214414778657,-0.134674815424893,
-2.04225517930412));
#42584=CARTESIAN_POINT('Ctrl Pts',(0.108229969381733,-0.0988696690312163,
-2.03960608220147));
#42585=CARTESIAN_POINT('Ctrl Pts',(0.140938497285599,-0.0630645226375404,
-2.03695698509882));
#42586=CARTESIAN_POINT('Ctrl Pts',(0.154117116391439,-0.00941851728306658,
-2.03430788799617));
#42587=CARTESIAN_POINT('Ctrl Pts',(0.141722210356908,0.0374666894489691,
-2.03165879089352));
#42588=CARTESIAN_POINT('Ctrl Pts',(0.129327304322376,0.0843518961810062,
-2.02900969379087));
#42589=CARTESIAN_POINT('Ctrl Pts',(0.0913588731474758,0.124476304290605,
-2.02636059668822));
#42590=CARTESIAN_POINT('Ctrl Pts',(0.0452289559312077,0.139439159751076,
-2.02371149958557));
#42591=CARTESIAN_POINT('Ctrl Pts',(-0.000900961285057872,0.154402015211546,
-2.02106240248292));
#42592=CARTESIAN_POINT('Ctrl Pts',(-0.0551923645426887,0.144203318022889,
-2.01841330538027));
#42593=CARTESIAN_POINT('Ctrl Pts',(-0.0927476215980198,0.113520114581618,
-2.01576420827762));
#42594=CARTESIAN_POINT('Ctrl Pts',(-0.126056565344061,0.0863062122544981,
-2.01341464037984));
#42595=CARTESIAN_POINT('Ctrl Pts',(-0.146200059172505,0.0429782214212413,
-2.01106507248206));
#42596=CARTESIAN_POINT('Ctrl Pts',(-0.14651679492655,-9.2174979582009E-5,
-2.00871550458428));
#42597=CARTESIAN_POINT('Origin',(0.,0.,-1.487));
#42598=CARTESIAN_POINT('',(-0.146467901202366,0.000113550927785495,-1.95158449541571));
#42599=CARTESIAN_POINT('',(-0.146430225588029,0.000124228536857034,-1.95871550458428));
#42600=CARTESIAN_POINT('',(-0.14635,-1.79227059055215E-17,-1.487));
#42601=CARTESIAN_POINT('Ctrl Pts',(-0.146467901202366,0.000113550927785495,
-1.95158449541571));
#42602=CARTESIAN_POINT('Ctrl Pts',(-0.146530905875648,0.00748045608225115,
-1.95198602332387));
#42603=CARTESIAN_POINT('Ctrl Pts',(-0.146023230868662,0.0148386496320622,
-1.95238755123203));
#42604=CARTESIAN_POINT('Ctrl Pts',(-0.144914795699676,0.0221052036384111,
-1.95278907914019));
#42605=CARTESIAN_POINT('Ctrl Pts',(-0.137601848492386,0.0700465964363302,
-1.95543817624284));
#42606=CARTESIAN_POINT('Ctrl Pts',(-0.104139279699996,0.11399914387574,
-1.95808727334549));
#42607=CARTESIAN_POINT('Ctrl Pts',(-0.0598727735695639,0.133806535810708,
-1.96073637044814));
#42608=CARTESIAN_POINT('Ctrl Pts',(-0.0156062674391309,0.153613927745677,
-1.96338546755079));
#42609=CARTESIAN_POINT('Ctrl Pts',(0.0394641760293445,0.149276164176203,
-1.96603456465344));
#42610=CARTESIAN_POINT('Ctrl Pts',(0.0800836625671089,0.122782511093445,
-1.96868366175609));
#42611=CARTESIAN_POINT('Ctrl Pts',(0.120703149104873,0.0962888580106879,
-1.97133275885874));
#42612=CARTESIAN_POINT('Ctrl Pts',(0.146871678711927,0.0476393154146473,
-1.9739818559614));
#42613=CARTESIAN_POINT('Ctrl Pts',(0.146588559060938,-0.000855799633410346,
-1.97663095306405));
#42614=CARTESIAN_POINT('Ctrl Pts',(0.146305439409949,-0.049350914681468,
-1.9792800501667));
#42615=CARTESIAN_POINT('Ctrl Pts',(0.119570670500917,-0.0976916021815428,
-1.98192914726935));
#42616=CARTESIAN_POINT('Ctrl Pts',(0.0786446177780337,-0.123709183713747,
-1.984578244372));
#42617=CARTESIAN_POINT('Ctrl Pts',(0.0377185650551491,-0.149726765245952,
-1.98722734147465));
#42618=CARTESIAN_POINT('Ctrl Pts',(-0.0173987714815884,-0.153421240810284,
-1.9898764385773));
#42619=CARTESIAN_POINT('Ctrl Pts',(-0.0614309927523799,-0.13309835149254,
-1.99252553567995));
#42620=CARTESIAN_POINT('Ctrl Pts',(-0.10546321402317,-0.112775462174795,
-1.9951746327826));
#42621=CARTESIAN_POINT('Ctrl Pts',(-0.138410320028015,-0.0684352079749748,
-1.99782372988525));
#42622=CARTESIAN_POINT('Ctrl Pts',(-0.145163013906248,-0.0204116984650692,
-2.0004728269879));
#42623=CARTESIAN_POINT('Ctrl Pts',(-0.146107581847224,-0.0136941619804954,
-2.0008433831305));
#42624=CARTESIAN_POINT('Ctrl Pts',(-0.146539617848722,-0.00690455722508045,
-2.00121393927311));
#42625=CARTESIAN_POINT('Ctrl Pts',(-0.146483524170368,-0.000107783910021919,
-2.00158449541571));
#42626=CARTESIAN_POINT('Ctrl Pts',(-0.14651679492655,-9.2174979582009E-5,
-2.00871550458428));
#42627=CARTESIAN_POINT('Ctrl Pts',(-0.146557173248306,-0.00558290440251719,
-2.00841597537941));
#42628=CARTESIAN_POINT('Ctrl Pts',(-0.14627533041133,-0.0110694474437864,
-2.00811644617454));
#42629=CARTESIAN_POINT('Ctrl Pts',(-0.145657465336476,-0.0165178848060591,
-2.00781691696966));
#42630=CARTESIAN_POINT('Ctrl Pts',(-0.140192941166569,-0.0647049710585717,
-2.00516781986701));
#42631=CARTESIAN_POINT('Ctrl Pts',(-0.108444781973725,-0.109911433869707,
-2.00251872276436));
#42632=CARTESIAN_POINT('Ctrl Pts',(-0.0649724565608736,-0.131405926864653,
-1.99986962566171));
#42633=CARTESIAN_POINT('Ctrl Pts',(-0.0215001311480229,-0.152900419859598,
-1.99722052855906));
#42634=CARTESIAN_POINT('Ctrl Pts',(0.0336963604848347,-0.150682943038354,
-1.99457143145641));
#42635=CARTESIAN_POINT('Ctrl Pts',(0.0753043193217198,-0.125770414717475,
-1.99192233435376));
#42636=CARTESIAN_POINT('Ctrl Pts',(0.116912278158607,-0.100857886396594,
-1.98927323725111));
#42637=CARTESIAN_POINT('Ctrl Pts',(0.144931704199522,-0.053250306576076,
-1.98662414014846));
#42638=CARTESIAN_POINT('Ctrl Pts',(0.146513097829673,-0.00478015596668234,
-1.98397504304581));
#42639=CARTESIAN_POINT('Ctrl Pts',(0.148094491459823,0.0436899946427065,
-1.98132594594316));
#42640=CARTESIAN_POINT('Ctrl Pts',(0.123237852679217,0.093022716040971,
-1.97867684884051));
#42641=CARTESIAN_POINT('Ctrl Pts',(0.0833422504755588,0.12059439046814,
-1.97602775173786));
#42642=CARTESIAN_POINT('Ctrl Pts',(0.0434466482718983,0.148166064895312,
-1.97337865463521));
#42643=CARTESIAN_POINT('Ctrl Pts',(-0.0114879173548165,0.153976692351384,
-1.97072955753256));
#42644=CARTESIAN_POINT('Ctrl Pts',(-0.0562688646997204,0.135361562461866,
-1.96808046042991));
#42645=CARTESIAN_POINT('Ctrl Pts',(-0.101049812044625,0.116746432572348,
-1.96543136332725));
#42646=CARTESIAN_POINT('Ctrl Pts',(-0.135677141107718,0.0737055453372412,
-1.9627822662246));
#42647=CARTESIAN_POINT('Ctrl Pts',(-0.14427101727684,0.0259771303384112,
-1.96013316912195));
#42648=CARTESIAN_POINT('Ctrl Pts',(-0.145804021795487,0.017463175235828,
-1.95966061427606));
#42649=CARTESIAN_POINT('Ctrl Pts',(-0.146508625607797,0.00880006007651845,
-1.95918805943017));
#42650=CARTESIAN_POINT('Ctrl Pts',(-0.146430225588029,0.000124228536857034,
-1.95871550458428));
#42651=CARTESIAN_POINT('Origin',(0.,0.,-1.487));
#42652=CARTESIAN_POINT('',(-0.146121465979963,4.50978529691337E-5,-1.90158449541571));
#42653=CARTESIAN_POINT('',(-0.146112202146807,2.42034320618872E-5,-1.90871550458428));
#42654=CARTESIAN_POINT('',(-0.14635,-1.79227059055215E-17,-1.487));
#42655=CARTESIAN_POINT('Ctrl Pts',(-0.146121465979963,4.50978529691337E-5,
-1.90158449541571));
#42656=CARTESIAN_POINT('Ctrl Pts',(-0.146181182134258,0.0217075988651919,
-1.90275810737463));
#42657=CARTESIAN_POINT('Ctrl Pts',(-0.141674343543634,0.04334647161387,
-1.90393171933356));
#42658=CARTESIAN_POINT('Ctrl Pts',(-0.132475676519681,0.0627625140607628,
-1.90510533129248));
#42659=CARTESIAN_POINT('Ctrl Pts',(-0.111712287073873,0.106588739074822,
-1.90775442839513));
#42660=CARTESIAN_POINT('Ctrl Pts',(-0.0670438933564559,0.139089578130225,
-1.91040352549778));
#42661=CARTESIAN_POINT('Ctrl Pts',(-0.0189550872725999,0.145360389057895,
-1.91305262260043));
#42662=CARTESIAN_POINT('Ctrl Pts',(0.029133718811256,0.151631199985565,
-1.91570171970308));
#42663=CARTESIAN_POINT('Ctrl Pts',(0.0806429372615497,0.131671982785502,
-1.91835081680573));
#42664=CARTESIAN_POINT('Ctrl Pts',(0.111950825017996,0.0946358854682761,
-1.92099991390838));
#42665=CARTESIAN_POINT('Ctrl Pts',(0.14325871277444,0.0575997881510518,
-1.92364901101104));
#42666=CARTESIAN_POINT('Ctrl Pts',(0.154365269837039,0.00348681071666326,
-1.92629810811369));
#42667=CARTESIAN_POINT('Ctrl Pts',(0.140177112048345,-0.0428872393417926,
-1.92894720521634));
#42668=CARTESIAN_POINT('Ctrl Pts',(0.125988954259651,-0.0892612894002504,
-1.93159630231899));
#42669=CARTESIAN_POINT('Ctrl Pts',(0.0865060816196672,-0.127896412082776,
-1.93424539942164));
#42670=CARTESIAN_POINT('Ctrl Pts',(0.0398350447778369,-0.141074828541885,
-1.93689449652429));
#42671=CARTESIAN_POINT('Ctrl Pts',(-0.00683599206399215,-0.154253245000994,
-1.93954359362694));
#42672=CARTESIAN_POINT('Ctrl Pts',(-0.0606951931076668,-0.141974955236685,
-1.94219269072959));
#42673=CARTESIAN_POINT('Ctrl Pts',(-0.0970431308184098,-0.109870691276316,
-1.94484178783224));
#42674=CARTESIAN_POINT('Ctrl Pts',(-0.127881753155114,-0.082632522234911,
-1.94708935702673));
#42675=CARTESIAN_POINT('Ctrl Pts',(-0.146115229918752,-0.0411230075962279,
-1.94933692622122));
#42676=CARTESIAN_POINT('Ctrl Pts',(-0.146467901202366,0.000113550927785495,
-1.95158449541571));
#42677=CARTESIAN_POINT('Ctrl Pts',(-0.146430225588029,0.000124228536857034,
-1.95871550458428));
#42678=CARTESIAN_POINT('Ctrl Pts',(-0.146069122623071,-0.0398358186890666,
-1.95653896232752));
#42679=CARTESIAN_POINT('Ctrl Pts',(-0.129097100987133,-0.0800656356800447,
-1.95436242007076));
#42680=CARTESIAN_POINT('Ctrl Pts',(-0.0999499468002784,-0.10723313788813,
-1.952185877814));
#42681=CARTESIAN_POINT('Ctrl Pts',(-0.0644745768794416,-0.140299048353297,
-1.94953678071135));
#42682=CARTESIAN_POINT('Ctrl Pts',(-0.0109634137626148,-0.154014926521079,
-1.9468876836087));
#42683=CARTESIAN_POINT('Ctrl Pts',(0.0360437226105418,-0.142090773054014,
-1.94423858650605));
#42684=CARTESIAN_POINT('Ctrl Pts',(0.0830508589836977,-0.13016661958695,
-1.9415894894034));
#42685=CARTESIAN_POINT('Ctrl Pts',(0.123553968613184,-0.0926024344850394,
-1.93894039230075));
#42686=CARTESIAN_POINT('Ctrl Pts',(0.138978627782331,-0.0466248726159469,
-1.9362912951981));
#42687=CARTESIAN_POINT('Ctrl Pts',(0.154403286951479,-0.000647310746854889,
-1.93364219809545));
#42688=CARTESIAN_POINT('Ctrl Pts',(0.144749495660286,0.0537436278894195,
-1.9309931009928));
#42689=CARTESIAN_POINT('Ctrl Pts',(0.114444410528462,0.0916046648676035,
-1.92834400389015));
#42690=CARTESIAN_POINT('Ctrl Pts',(0.0841393253966373,0.129465701845788,
-1.9256949067875));
#42691=CARTESIAN_POINT('Ctrl Pts',(0.033182946424181,0.150796837165882,
-1.92304580968485));
#42692=CARTESIAN_POINT('Ctrl Pts',(-0.0150565113861619,0.145815771408965,
-1.9203967125822));
#42693=CARTESIAN_POINT('Ctrl Pts',(-0.0632959691965042,0.140834705652047,
-1.91774761547955));
#42694=CARTESIAN_POINT('Ctrl Pts',(-0.108818505844733,0.109541438818118,
-1.91509851837689));
#42695=CARTESIAN_POINT('Ctrl Pts',(-0.130747825853863,0.0662868294701219,
-1.91244942127424));
#42696=CARTESIAN_POINT('Ctrl Pts',(-0.141050990895727,0.0459642942183122,
-1.91120478237759));
#42697=CARTESIAN_POINT('Ctrl Pts',(-0.146146070039581,0.0230013517587152,
-1.90996014348094));
#42698=CARTESIAN_POINT('Ctrl Pts',(-0.146112202146807,2.42034320618872E-5,
-1.90871550458428));
#42699=CARTESIAN_POINT('Origin',(0.,0.,-1.487));
#42700=CARTESIAN_POINT('',(-0.146302162622722,-0.00013309729056632,-1.85158449541571));
#42701=CARTESIAN_POINT('',(-0.146341186202789,-0.000134609574743057,-1.85871550458428));
#42702=CARTESIAN_POINT('',(-0.14635,-1.79227059055215E-17,-1.487));
#42703=CARTESIAN_POINT('Ctrl Pts',(-0.146302162622722,-0.00013309729056632,
-1.85158449541571));
#42704=CARTESIAN_POINT('Ctrl Pts',(-0.145984741937988,0.0356689174518258,
-1.8535301914254));
#42705=CARTESIAN_POINT('Ctrl Pts',(-0.132738385200244,0.071681077496235,
-1.85547588743509));
#42706=CARTESIAN_POINT('Ctrl Pts',(-0.108892092441933,0.0981399523343686,
-1.85742158344477));
#42707=CARTESIAN_POINT('Ctrl Pts',(-0.0764249728402753,0.134164145386161,
-1.86007068054742));
#42708=CARTESIAN_POINT('Ctrl Pts',(-0.0243084654917135,0.15247915557962,
-1.86271977765007));
#42709=CARTESIAN_POINT('Ctrl Pts',(0.0235571883881887,0.144685855963249,
-1.86536887475272));
#42710=CARTESIAN_POINT('Ctrl Pts',(0.0714228422680896,0.136892556346878,
-1.86801797185537));
#42711=CARTESIAN_POINT('Ctrl Pts',(0.115037642679331,0.102990946920679,
-1.87066706895803));
#42712=CARTESIAN_POINT('Ctrl Pts',(0.134400167741787,0.0585280526888954,
-1.87331616606068));
#42713=CARTESIAN_POINT('Ctrl Pts',(0.153762692804244,0.0140651584571082,
-1.87596526316333));
#42714=CARTESIAN_POINT('Ctrl Pts',(0.148872942517911,-0.0409590205802653,
-1.87861436026598));
#42715=CARTESIAN_POINT('Ctrl Pts',(0.121973319861668,-0.0813108066772044,
-1.88126345736863));
#42716=CARTESIAN_POINT('Ctrl Pts',(0.0950736972054269,-0.121662592774141,
-1.88391255447128));
#42717=CARTESIAN_POINT('Ctrl Pts',(0.0461642021792778,-0.147341985930645,
-1.88656165157393));
#42718=CARTESIAN_POINT('Ctrl Pts',(-0.00232563591163342,-0.146572608144159,
-1.88921074867658));
#42719=CARTESIAN_POINT('Ctrl Pts',(-0.0508154740025447,-0.145803230357672,
-1.89185984577923));
#42720=CARTESIAN_POINT('Ctrl Pts',(-0.0988856551582181,-0.118585081628195,
-1.89450894288188));
#42721=CARTESIAN_POINT('Ctrl Pts',(-0.124491553148954,-0.0774002017770997,
-1.89715803998453));
#42722=CARTESIAN_POINT('Ctrl Pts',(-0.138753439600492,-0.0544611867045152,
-1.89863352512826));
#42723=CARTESIAN_POINT('Ctrl Pts',(-0.146046389803521,-0.0271893710670532,
-1.90010901027198));
#42724=CARTESIAN_POINT('Ctrl Pts',(-0.146121465979963,4.50978529691337E-5,
-1.90158449541571));
#42725=CARTESIAN_POINT('Ctrl Pts',(-0.146112202146807,2.42034320618872E-5,
-1.90871550458428));
#42726=CARTESIAN_POINT('Ctrl Pts',(-0.146073985407756,-0.0259033524273363,
-1.90731104637829));
#42727=CARTESIAN_POINT('Ctrl Pts',(-0.139505077963029,-0.0518489966240254,
-1.90590658817229));
#42728=CARTESIAN_POINT('Ctrl Pts',(-0.12651918653732,-0.0740394027842464,
-1.90450212996629));
#42729=CARTESIAN_POINT('Ctrl Pts',(-0.102025123841615,-0.115895073828558,
-1.90185303286364));
#42730=CARTESIAN_POINT('Ctrl Pts',(-0.0547008950801745,-0.144390464055115,
-1.89920393576099));
#42731=CARTESIAN_POINT('Ctrl Pts',(-0.00624903828330516,-0.14645780022671,
-1.89655483865834));
#42732=CARTESIAN_POINT('Ctrl Pts',(0.0422028185135615,-0.148525136398304,
-1.89390574155569));
#42733=CARTESIAN_POINT('Ctrl Pts',(0.0917823033458551,-0.124164418514939,
-1.89125664445304));
#42734=CARTESIAN_POINT('Ctrl Pts',(0.11975263458487,-0.0845472899429408,
-1.88860754735039));
#42735=CARTESIAN_POINT('Ctrl Pts',(0.147722965823886,-0.0449301613709413,
-1.88595845024774));
#42736=CARTESIAN_POINT('Ctrl Pts',(0.15408414346962,0.00994337788969538,
-1.88330935314509));
#42737=CARTESIAN_POINT('Ctrl Pts',(0.13591897894051,0.0549087323700171,
-1.88066025604244));
#42738=CARTESIAN_POINT('Ctrl Pts',(0.117753814411401,0.0998740868503387,
-1.87801115893979));
#42739=CARTESIAN_POINT('Ctrl Pts',(0.0750623077074499,0.134931256550348,
-1.87536206183714));
#42740=CARTESIAN_POINT('Ctrl Pts',(0.0274224651070917,0.144003285150594,
-1.87271296473449));
#42741=CARTESIAN_POINT('Ctrl Pts',(-0.0202173774932664,0.153075313750841,
-1.87006386763184));
#42742=CARTESIAN_POINT('Ctrl Pts',(-0.0728055559900301,0.136162201251325,
-1.86741477052919));
#42743=CARTESIAN_POINT('Ctrl Pts',(-0.106225524300139,0.101020174786394,
-1.86476567342654));
#42744=CARTESIAN_POINT('Ctrl Pts',(-0.131667708705355,0.0742670100497515,
-1.86274895047912));
#42745=CARTESIAN_POINT('Ctrl Pts',(-0.146000808165931,0.0369491367817265,
-1.8607322275317));
#42746=CARTESIAN_POINT('Ctrl Pts',(-0.146341186202789,-0.000134609574743057,
-1.85871550458428));
#42747=CARTESIAN_POINT('Origin',(0.,0.,-1.487));
#42748=CARTESIAN_POINT('',(-0.146586453393407,2.34618399145015E-5,-1.80158449541571));
#42749=CARTESIAN_POINT('',(-0.146572905486282,4.68275666195741E-5,-1.80871550458428));
#42750=CARTESIAN_POINT('',(-0.14635,-1.79227059055215E-17,-1.487));
#42751=CARTESIAN_POINT('Ctrl Pts',(-0.146586453393407,2.34618399145015E-5,
-1.80158449541571));
#42752=CARTESIAN_POINT('Ctrl Pts',(-0.146589249888724,0.00128091906965625,
-1.80165317837351));
#42753=CARTESIAN_POINT('Ctrl Pts',(-0.146574472401979,0.00253830888863432,
-1.80172186133131));
#42754=CARTESIAN_POINT('Ctrl Pts',(-0.14654191962176,0.00379523835145167,
-1.80179054428911));
#42755=CARTESIAN_POINT('Ctrl Pts',(-0.145286361059294,0.0522749239213617,
-1.80443964139176));
#42756=CARTESIAN_POINT('Ctrl Pts',(-0.117587569244064,0.100069765364511,
-1.80708873849441));
#42757=CARTESIAN_POINT('Ctrl Pts',(-0.0761480033285232,0.125261405187926,
-1.80973783559706));
#42758=CARTESIAN_POINT('Ctrl Pts',(-0.0347084374129826,0.150453045011341,
-1.81238693269971));
#42759=CARTESIAN_POINT('Ctrl Pts',(0.0204719026028683,0.153041483215024,
-1.81503602980236));
#42760=CARTESIAN_POINT('Ctrl Pts',(0.0640877247140375,0.131839681361691,
-1.81768512690501));
#42761=CARTESIAN_POINT('Ctrl Pts',(0.107703546825207,0.110637879508359,
-1.82033422400766));
#42762=CARTESIAN_POINT('Ctrl Pts',(0.139754851031694,0.0656458375980124,
-1.82298332111031));
#42763=CARTESIAN_POINT('Ctrl Pts',(0.145543148490318,0.0174965701810349,
-1.82563241821297));
#42764=CARTESIAN_POINT('Ctrl Pts',(0.151331445948941,-0.0306526972359428,
-1.82828151531562));
#42765=CARTESIAN_POINT('Ctrl Pts',(0.130856736659701,-0.0819591901595512,
-1.83093061241827));
#42766=CARTESIAN_POINT('Ctrl Pts',(0.0935085694570671,-0.112894133942679,
-1.83357970952092));
#42767=CARTESIAN_POINT('Ctrl Pts',(0.0561604022544324,-0.143829077725807,
-1.83622880662357));
#42768=CARTESIAN_POINT('Ctrl Pts',(0.00193877713840383,-0.154392472368453,
-1.83887790372622));
#42769=CARTESIAN_POINT('Ctrl Pts',(-0.0442906733821896,-0.139740023944204,
-1.84152700082887));
#42770=CARTESIAN_POINT('Ctrl Pts',(-0.0905201239027831,-0.125087575519956,
-1.84417609793152));
#42771=CARTESIAN_POINT('Ctrl Pts',(-0.128757399827941,-0.0852192840288131,
-1.84682519503417));
#42772=CARTESIAN_POINT('Ctrl Pts',(-0.141467171863142,-0.0384184503281782,
-1.84947429213682));
#42773=CARTESIAN_POINT('Ctrl Pts',(-0.144841932090664,-0.0259916662953639,
-1.85017769322978));
#42774=CARTESIAN_POINT('Ctrl Pts',(-0.146416915418359,-0.0130761141722773,
-1.85088109432275));
#42775=CARTESIAN_POINT('Ctrl Pts',(-0.146302162622722,-0.00013309729056632,
-1.85158449541571));
#42776=CARTESIAN_POINT('Ctrl Pts',(-0.146341186202789,-0.000134609574743057,
-1.85871550458428));
#42777=CARTESIAN_POINT('Ctrl Pts',(-0.146447916913517,-0.0117627823017354,
-1.85808313042905));
#42778=CARTESIAN_POINT('Ctrl Pts',(-0.145178839300704,-0.0233679349353573,
-1.85745075627382));
#42779=CARTESIAN_POINT('Ctrl Pts',(-0.14244504878576,-0.0346171316422315,
-1.85681838211858));
#42780=CARTESIAN_POINT('Ctrl Pts',(-0.130992846837817,-0.0817414711755775,
-1.85416928501593));
#42781=CARTESIAN_POINT('Ctrl Pts',(-0.0938366848184793,-0.122619209811925,
-1.85152018791328));
#42782=CARTESIAN_POINT('Ctrl Pts',(-0.0480161012556727,-0.138504121768697,
-1.84887109081063));
#42783=CARTESIAN_POINT('Ctrl Pts',(-0.00219551769286602,-0.154389033725469,
-1.84622199370798));
#42784=CARTESIAN_POINT('Ctrl Pts',(0.0522894874134106,-0.145281119002665,
-1.84357289660533));
#42785=CARTESIAN_POINT('Ctrl Pts',(0.0904524974569562,-0.115357199300748,
-1.84092379950268));
#42786=CARTESIAN_POINT('Ctrl Pts',(0.128615507500503,-0.08543327959883,
-1.83827470240003));
#42787=CARTESIAN_POINT('Ctrl Pts',(0.150456522481318,-0.0346933549178013,
-1.83562560529738));
#42788=CARTESIAN_POINT('Ctrl Pts',(0.145959415974372,0.0135936240617936,
-1.83297650819473));
#42789=CARTESIAN_POINT('Ctrl Pts',(0.141462309467426,0.0618806030413885,
-1.83032741109208));
#42790=CARTESIAN_POINT('Ctrl Pts',(0.110627081472717,0.107714636319548,
-1.82767831398943));
#42791=CARTESIAN_POINT('Ctrl Pts',(0.0675945373608278,0.13007657839015,
-1.82502921688678));
#42792=CARTESIAN_POINT('Ctrl Pts',(0.0245619932489395,0.152438520460751,
-1.82238011978413));
#42793=CARTESIAN_POINT('Ctrl Pts',(-0.0306678669801303,0.151328371323796,
-1.81973102268148));
#42794=CARTESIAN_POINT('Ctrl Pts',(-0.072767041721279,0.127255237086128,
-1.81708192557883));
#42795=CARTESIAN_POINT('Ctrl Pts',(-0.114866216462428,0.103182102848461,
-1.81443282847617));
#42796=CARTESIAN_POINT('Ctrl Pts',(-0.143834705715656,0.0561459835100795,
-1.81178373137352));
#42797=CARTESIAN_POINT('Ctrl Pts',(-0.146387776561852,0.0077172922706412,
-1.80913463427087));
#42798=CARTESIAN_POINT('Ctrl Pts',(-0.146522422158967,0.00516322681681316,
-1.80899492437534));
#42799=CARTESIAN_POINT('Ctrl Pts',(-0.146583596735172,0.00260528810693123,
-1.80885521447981));
#42800=CARTESIAN_POINT('Ctrl Pts',(-0.146572905486282,4.68275666195741E-5,
-1.80871550458428));
#42801=CARTESIAN_POINT('Origin',(0.,0.,-1.487));
#42802=CARTESIAN_POINT('',(-0.146232247576531,0.000120056641797081,-1.75158449541571));
#42803=CARTESIAN_POINT('',(-0.146200518682322,0.000108553130818545,-1.75871550458428));
#42804=CARTESIAN_POINT('',(-0.14635,-1.79227059055215E-17,-1.487));
#42805=CARTESIAN_POINT('Ctrl Pts',(-0.146232247576531,0.000120056641797081,
-1.75158449541571));
#42806=CARTESIAN_POINT('Ctrl Pts',(-0.146351639518327,0.0156094297883246,
-1.75242526242427));
#42807=CARTESIAN_POINT('Ctrl Pts',(-0.144086148722195,0.031064779006721,
-1.75326602943284));
#42808=CARTESIAN_POINT('Ctrl Pts',(-0.139288885238194,0.0456896540770004,
-1.7541067964414));
#42809=CARTESIAN_POINT('Ctrl Pts',(-0.124173619455077,0.091769856773679,
-1.75675589354405));
#42810=CARTESIAN_POINT('Ctrl Pts',(-0.0839239177960128,0.129605441253845,
-1.7594049906467));
#42811=CARTESIAN_POINT('Ctrl Pts',(-0.036997992974151,0.141845290920986,
-1.76205408774935));
#42812=CARTESIAN_POINT('Ctrl Pts',(0.00992793184771074,0.154085140588127,
-1.764703184852));
#42813=CARTESIAN_POINT('Ctrl Pts',(0.0635300798323712,0.140729255442244,
-1.76735228195465));
#42814=CARTESIAN_POINT('Ctrl Pts',(0.0992269060589921,0.107902544708336,
-1.7700013790573));
#42815=CARTESIAN_POINT('Ctrl Pts',(0.134923732285611,0.0750758339744305,
-1.77265047615995));
#42816=CARTESIAN_POINT('Ctrl Pts',(0.152715236754193,0.0227782976525062,
-1.77529957326261));
#42817=CARTESIAN_POINT('Ctrl Pts',(0.144442368330655,-0.0250068045060932,
-1.77794867036526));
#42818=CARTESIAN_POINT('Ctrl Pts',(0.136169499907116,-0.0727919066646952,
-1.78059776746791));
#42819=CARTESIAN_POINT('Ctrl Pts',(0.101832258591451,-0.11606457465997,
-1.78324686457056));
#42820=CARTESIAN_POINT('Ctrl Pts',(0.057177446920383,-0.1349802859837,-1.78589596167321));
#42821=CARTESIAN_POINT('Ctrl Pts',(0.0125226352493163,-0.153895997307429,
-1.78854505877586));
#42822=CARTESIAN_POINT('Ctrl Pts',(-0.0424497467771537,-0.148454751959616,
-1.79119415587851));
#42823=CARTESIAN_POINT('Ctrl Pts',(-0.0825297751355384,-0.121151864437375,
-1.79384325298116));
#42824=CARTESIAN_POINT('Ctrl Pts',(-0.121570651364079,-0.0945568569961039,
-1.79642366712601));
#42825=CARTESIAN_POINT('Ctrl Pts',(-0.146481389250798,-0.0472191224353378,
-1.79900408127086));
#42826=CARTESIAN_POINT('Ctrl Pts',(-0.146586453393407,2.34618399145015E-5,
-1.80158449541571));
#42827=CARTESIAN_POINT('Ctrl Pts',(-0.146572905486282,4.68275666195741E-5,
-1.80871550458428));
#42828=CARTESIAN_POINT('Ctrl Pts',(-0.146380875543874,-0.0459067401848022,
-1.80620611737716));
#42829=CARTESIAN_POINT('Ctrl Pts',(-0.123004041028004,-0.0920286568909353,
-1.80369673017004));
#42830=CARTESIAN_POINT('Ctrl Pts',(-0.0857438283361303,-0.118898837794897,
-1.80118734296292));
#42831=CARTESIAN_POINT('Ctrl Pts',(-0.0464091568250557,-0.147265013480497,
-1.79853824586027));
#42832=CARTESIAN_POINT('Ctrl Pts',(0.00839783863625381,-0.154176101711202,
-1.79588914875762));
#42833=CARTESIAN_POINT('Ctrl Pts',(0.053543079068469,-0.136462729016317,
-1.79324005165497));
#42834=CARTESIAN_POINT('Ctrl Pts',(0.0986883195006868,-0.118749356321431,
-1.79059095455232));
#42835=CARTESIAN_POINT('Ctrl Pts',(0.134171804903809,-0.0764115227009509,
-1.78794185744967));
#42836=CARTESIAN_POINT('Ctrl Pts',(0.143721073759422,-0.0288650425974362,
-1.78529276034702));
#42837=CARTESIAN_POINT('Ctrl Pts',(0.153270342615035,0.0186814375060771,
-1.78264366324437));
#42838=CARTESIAN_POINT('Ctrl Pts',(0.13688539492314,0.0714365640926248,
-1.77999456614172));
#42839=CARTESIAN_POINT('Ctrl Pts',(0.102080245380109,0.105207229931454,
-1.77734546903907));
#42840=CARTESIAN_POINT('Ctrl Pts',(0.0672750958370787,0.138977895770283,
-1.77469637193642));
#42841=CARTESIAN_POINT('Ctrl Pts',(0.0140497444429127,0.153764100861393,
-1.77204727483377));
#42842=CARTESIAN_POINT('Ctrl Pts',(-0.0331870599851328,0.142785001930372,
-1.76939817773112));
#42843=CARTESIAN_POINT('Ctrl Pts',(-0.0804238644131796,0.131805902999351,
-1.76674908062846));
#42844=CARTESIAN_POINT('Ctrl Pts',(-0.121672121875106,0.0950615000461977,
-1.76409998352581));
#42845=CARTESIAN_POINT('Ctrl Pts',(-0.138015689420879,0.0494025019649056,
-1.76145088642316));
#42846=CARTESIAN_POINT('Ctrl Pts',(-0.143640989427498,0.0336871104820155,
-1.76053909247687));
#42847=CARTESIAN_POINT('Ctrl Pts',(-0.146315903748105,0.0169156330188866,
-1.75962729853058));
#42848=CARTESIAN_POINT('Ctrl Pts',(-0.146200518682322,0.000108553130818545,
-1.75871550458428));
#42849=CARTESIAN_POINT('Origin',(0.,0.,-1.487));
#42850=CARTESIAN_POINT('',(-0.146154722497813,-8.18537555021537E-5,-1.70158449541571));
#42851=CARTESIAN_POINT('',(-0.146179203325735,-9.80254664548016E-5,-1.70871550458428));
#42852=CARTESIAN_POINT('',(-0.14635,-1.79227059055215E-17,-1.487));
#42853=CARTESIAN_POINT('Ctrl Pts',(-0.146154722497813,-8.18537555021537E-5,
-1.70158449541571));
#42854=CARTESIAN_POINT('Ctrl Pts',(-0.146003790237749,0.029671180203538,
-1.70319734647504));
#42855=CARTESIAN_POINT('Ctrl Pts',(-0.137184906065914,0.0595064104567512,
-1.70481019753436));
#42856=CARTESIAN_POINT('Ctrl Pts',(-0.120318227416389,0.0837404453770858,
-1.70642304859369));
#42857=CARTESIAN_POINT('Ctrl Pts',(-0.092614820283167,0.123544686023934,
-1.70907214569634));
#42858=CARTESIAN_POINT('Ctrl Pts',(-0.0432001993188249,0.14823810967376,
-1.71172124279899));
#42859=CARTESIAN_POINT('Ctrl Pts',(0.00526445918704815,0.146496496579415,
-1.71437033990164));
#42860=CARTESIAN_POINT('Ctrl Pts',(0.0537291176929198,0.14475488348507,
-1.71701943700429));
#42861=CARTESIAN_POINT('Ctrl Pts',(0.101243813740321,0.116578233646556,
-1.71966853410694));
#42862=CARTESIAN_POINT('Ctrl Pts',(0.126018662423459,0.0748881483385505,
-1.72231763120959));
#42863=CARTESIAN_POINT('Ctrl Pts',(0.150793511106598,0.0331980630305453,
-1.72496672831224));
#42864=CARTESIAN_POINT('Ctrl Pts',(0.152828512425473,-0.0220054577469498,
-1.7276158254149));
#42865=CARTESIAN_POINT('Ctrl Pts',(0.131190429966719,-0.0654064914647002,
-1.73026492251755));
#42866=CARTESIAN_POINT('Ctrl Pts',(0.109552347507966,-0.108807525182449,
-1.7329140196202));
#42867=CARTESIAN_POINT('Ctrl Pts',(0.0642411812715823,-0.140406071840456,
-1.73556311672285));
#42868=CARTESIAN_POINT('Ctrl Pts',(0.0160362938415837,-0.145711273827391,
-1.7382122138255));
#42869=CARTESIAN_POINT('Ctrl Pts',(-0.0321685935884163,-0.151016475814326,
-1.74086131092815));
#42870=CARTESIAN_POINT('Ctrl Pts',(-0.083267202212033,-0.130028333130192,
-1.7435104080308));
#42871=CARTESIAN_POINT('Ctrl Pts',(-0.113826091570257,-0.0923718513315293,
-1.74615950513345));
#42872=CARTESIAN_POINT('Ctrl Pts',(-0.134686240189591,-0.0666667349710097,
-1.74796783522754));
#42873=CARTESIAN_POINT('Ctrl Pts',(-0.145975458193573,-0.0331946420964979,
-1.74977616532162));
#42874=CARTESIAN_POINT('Ctrl Pts',(-0.146232247576531,0.000120056641797081,
-1.75158449541571));
#42875=CARTESIAN_POINT('Ctrl Pts',(-0.146200518682322,0.000108553130818545,
-1.75871550458428));
#42876=CARTESIAN_POINT('Ctrl Pts',(-0.145980667651508,-0.0319151217985716,
-1.75697820142793));
#42877=CARTESIAN_POINT('Ctrl Pts',(-0.135630836057442,-0.0640680487624917,
-1.75524089827157));
#42878=CARTESIAN_POINT('Ctrl Pts',(-0.116258389119244,-0.0892912352143908,
-1.75350359511521));
#42879=CARTESIAN_POINT('Ctrl Pts',(-0.0867186436422094,-0.127752381102974,
-1.75085449801256));
#42880=CARTESIAN_POINT('Ctrl Pts',(-0.0362002750585158,-0.150101079670706,
-1.74820540090991));
#42881=CARTESIAN_POINT('Ctrl Pts',(0.0121293699235867,-0.146088384589501,
-1.74555630380726));
#42882=CARTESIAN_POINT('Ctrl Pts',(0.0604590149056865,-0.142075689508295,
-1.74290720670461));
#42883=CARTESIAN_POINT('Ctrl Pts',(0.106599936286197,-0.111701600778155,
-1.74025810960196));
#42884=CARTESIAN_POINT('Ctrl Pts',(0.129392251966206,-0.068895448745377,
-1.73760901249931));
#42885=CARTESIAN_POINT('Ctrl Pts',(0.152184567646216,-0.0260892967125986,
-1.73495991539666));
#42886=CARTESIAN_POINT('Ctrl Pts',(0.151628277625726,0.0291489186228149,
-1.73231081829401));
#42887=CARTESIAN_POINT('Ctrl Pts',(0.127978492355377,0.0714873640663704,
-1.72966172119136));
#42888=CARTESIAN_POINT('Ctrl Pts',(0.104328707085028,0.113825809509926,
-1.72701262408871));
#42889=CARTESIAN_POINT('Ctrl Pts',(0.0575854265648198,0.143264485061621,
-1.72436352698606));
#42890=CARTESIAN_POINT('Ctrl Pts',(0.00918477029846232,0.146303033875848,
-1.72171442988341));
#42891=CARTESIAN_POINT('Ctrl Pts',(-0.0392158859678952,0.149341582690075,
-1.71906533278076));
#42892=CARTESIAN_POINT('Ctrl Pts',(-0.089273917980403,0.125980004766836,
-1.7164162356781));
#42893=CARTESIAN_POINT('Ctrl Pts',(-0.118033085945904,0.086931745345414,
-1.71376713857545));
#42894=CARTESIAN_POINT('Ctrl Pts',(-0.136313627683054,0.062111022542423,
-1.7120832605784));
#42895=CARTESIAN_POINT('Ctrl Pts',(-0.145988554068708,0.030952236506723,
-1.71039938258134));
#42896=CARTESIAN_POINT('Ctrl Pts',(-0.146179203325735,-9.80254664548015E-5,
-1.70871550458428));
#42897=CARTESIAN_POINT('Origin',(0.,0.,-1.487));
#42898=CARTESIAN_POINT('',(-0.14653173368382,-8.32536397529643E-5,-1.65158449541571));
#42899=CARTESIAN_POINT('',(-0.146557652869009,-6.33180884534729E-5,-1.65871550458428));
#42900=CARTESIAN_POINT('',(-0.14635,-1.79227059055215E-17,-1.487));
#42901=CARTESIAN_POINT('Ctrl Pts',(-0.14653173368382,-8.32536397529643E-5,
-1.65158449541571));
#42902=CARTESIAN_POINT('Ctrl Pts',(-0.146234877222684,0.0436237564073687,
-1.6539694305258));
#42903=CARTESIAN_POINT('Ctrl Pts',(-0.125401469120029,0.0875762997777429,
-1.65635436563589));
#42904=CARTESIAN_POINT('Ctrl Pts',(-0.0912258453865786,0.114746604194105,
-1.65873930074598));
#42905=CARTESIAN_POINT('Ctrl Pts',(-0.0532648352817327,0.144926366487419,
-1.66138839784863));
#42906=CARTESIAN_POINT('Ctrl Pts',(0.00115771916799673,0.154400304621344,
-1.66403749495128));
#42907=CARTESIAN_POINT('Ctrl Pts',(0.0470840407613024,0.138823741291476,
-1.66668659205393));
#42908=CARTESIAN_POINT('Ctrl Pts',(0.0930103623546093,0.123247177961607,
-1.66933568915658));
#42909=CARTESIAN_POINT('Ctrl Pts',(0.130440451091492,0.0826201131679442,
-1.67198478625923));
#42910=CARTESIAN_POINT('Ctrl Pts',(0.142209147696246,0.0355738155401125,
-1.67463388336189));
#42911=CARTESIAN_POINT('Ctrl Pts',(0.153977844300999,-0.0114724820877164,
-1.67728298046454));
#42912=CARTESIAN_POINT('Ctrl Pts',(0.140085148773626,-0.0649380125497132,
-1.67993207756719));
#42913=CARTESIAN_POINT('Ctrl Pts',(0.106902147572739,-0.100303882701074,
-1.68258117466984));
#42914=CARTESIAN_POINT('Ctrl Pts',(0.0737191463718505,-0.135669752852438,
-1.68523027177249));
#42915=CARTESIAN_POINT('Ctrl Pts',(0.0212458394974457,-0.152935962693163,
-1.68787936887514));
#42916=CARTESIAN_POINT('Ctrl Pts',(-0.0264539062358995,-0.144184357284127,
-1.69052846597779));
#42917=CARTESIAN_POINT('Ctrl Pts',(-0.0741536519692447,-0.135432751875091,
-1.69317756308044));
#42918=CARTESIAN_POINT('Ctrl Pts',(-0.11707983656153,-0.100663331216293,
-1.69582666018309));
#42919=CARTESIAN_POINT('Ctrl Pts',(-0.135546832206621,-0.055821092064959,
-1.69847575728574));
#42920=CARTESIAN_POINT('Ctrl Pts',(-0.142770558037638,-0.0382801748793176,
-1.69951200332906));
#42921=CARTESIAN_POINT('Ctrl Pts',(-0.146251695467758,-0.0191979795369924,
-1.70054824937239));
#42922=CARTESIAN_POINT('Ctrl Pts',(-0.146154722497813,-8.18537555021537E-5,
-1.70158449541571));
#42923=CARTESIAN_POINT('Ctrl Pts',(-0.146179203325735,-9.80254664548015E-5,
-1.70871550458428));
#42924=CARTESIAN_POINT('Ctrl Pts',(-0.146288485771181,-0.0178964088069292,
-1.70775028547869));
#42925=CARTESIAN_POINT('Ctrl Pts',(-0.143281500139797,-0.0356591341771629,
-1.7067850663731));
#42926=CARTESIAN_POINT('Ctrl Pts',(-0.136992758016216,-0.052172042109003,
-1.7058198472675));
#42927=CARTESIAN_POINT('Ctrl Pts',(-0.119732958202532,-0.0974926292223889,
-1.70317075016485));
#42928=CARTESIAN_POINT('Ctrl Pts',(-0.0777530546566726,-0.133398862529558,
-1.7005216530622));
#42929=CARTESIAN_POINT('Ctrl Pts',(-0.0303047177609532,-0.143424411479155,
-1.69787255595955));
#42930=CARTESIAN_POINT('Ctrl Pts',(0.0171436191347676,-0.153449960428753,
-1.6952234588569));
#42931=CARTESIAN_POINT('Ctrl Pts',(0.0700603893803513,-0.137594825020773,
-1.69257436175425));
#42932=CARTESIAN_POINT('Ctrl Pts',(0.104178357169689,-0.103130051993285,
-1.6899252646516));
#42933=CARTESIAN_POINT('Ctrl Pts',(0.138296324959027,-0.0686652789657974,
-1.68727616754895));
#42934=CARTESIAN_POINT('Ctrl Pts',(0.153615490292124,-0.0155908683188006,
-1.6846270704463));
#42935=CARTESIAN_POINT('Ctrl Pts',(0.143110598306188,0.0317536514303153,
-1.68197797334365));
#42936=CARTESIAN_POINT('Ctrl Pts',(0.132605706320252,0.079098171179434,
-1.679328876241));
#42937=CARTESIAN_POINT('Ctrl Pts',(0.0962767570152818,0.120712800030669,
-1.67667977913835));
#42938=CARTESIAN_POINT('Ctrl Pts',(0.0507839353436132,0.137513379849849,
-1.67403068203569));
#42939=CARTESIAN_POINT('Ctrl Pts',(0.00529111367194721,0.154313959669027,
-1.67138158493304));
#42940=CARTESIAN_POINT('Ctrl Pts',(-0.0493655803664143,0.146300490456153,
-1.6687324878304));
#42941=CARTESIAN_POINT('Ctrl Pts',(-0.0881209949026922,0.117147889370969,
-1.66608339072774));
#42942=CARTESIAN_POINT('Ctrl Pts',(-0.124050907457956,0.0901206876165238,
-1.66362742867992));
#42943=CARTESIAN_POINT('Ctrl Pts',(-0.146313617841786,0.0449243323049988,
-1.6611714666321));
#42944=CARTESIAN_POINT('Ctrl Pts',(-0.146557652869009,-6.33180884534729E-5,
-1.65871550458428));
#42945=CARTESIAN_POINT('Origin',(0.,0.,-1.487));
#42946=CARTESIAN_POINT('',(-0.146410789716796,0.000128174727319227,-1.60158449541571));
#42947=CARTESIAN_POINT('',(-0.14637109517831,0.000133274683421165,-1.60871550458428));
#42948=CARTESIAN_POINT('',(-0.14635,-1.79227059055215E-17,-1.487));
#42949=CARTESIAN_POINT('Ctrl Pts',(-0.146410789716796,0.000128174727319227,
-1.60158449541571));
#42950=CARTESIAN_POINT('Ctrl Pts',(-0.146496395207264,0.00945652267731366,
-1.60209241747391));
#42951=CARTESIAN_POINT('Ctrl Pts',(-0.145681450775993,0.0187699689983965,
-1.60260033953212));
#42952=CARTESIAN_POINT('Ctrl Pts',(-0.143911848766203,0.0278983480741794,
-1.60310826159032));
#42953=CARTESIAN_POINT('Ctrl Pts',(-0.134682386329468,0.0755079412607435,
-1.60575735869297));
#42954=CARTESIAN_POINT('Ctrl Pts',(-0.0994842823287073,0.118083326301294,
-1.60840645579562));
#42955=CARTESIAN_POINT('Ctrl Pts',(-0.0544591245016121,0.13609974944537,
-1.61105555289827));
#42956=CARTESIAN_POINT('Ctrl Pts',(-0.00943396667451821,0.154116172589446,
-1.61370465000092));
#42957=CARTESIAN_POINT('Ctrl Pts',(0.0454182449789114,0.147573633837048,
-1.61635374710357));
#42958=CARTESIAN_POINT('Ctrl Pts',(0.0849426956711816,0.119472492619379,
-1.61900284420622));
#42959=CARTESIAN_POINT('Ctrl Pts',(0.124467146363453,0.0913713514017089,
-1.62165194130887));
#42960=CARTESIAN_POINT('Ctrl Pts',(0.148663836094565,0.0417116077187646,
-1.62430103841153));
#42961=CARTESIAN_POINT('Ctrl Pts',(0.146436343584327,-0.00673315069097555,
-1.62695013551418));
#42962=CARTESIAN_POINT('Ctrl Pts',(0.14420885107409,-0.0551779091007144,
-1.62959923261683));
#42963=CARTESIAN_POINT('Ctrl Pts',(0.115557176322507,-0.102407682237246,
-1.63224832971948));
#42964=CARTESIAN_POINT('Ctrl Pts',(0.0736207634832826,-0.126763248714733,
-1.63489742682213));
#42965=CARTESIAN_POINT('Ctrl Pts',(0.0316843506440586,-0.151118815192219,
-1.63754652392478));
#42966=CARTESIAN_POINT('Ctrl Pts',(-0.0235368002828062,-0.152600175010656,
-1.64019562102743));
#42967=CARTESIAN_POINT('Ctrl Pts',(-0.0667186817131846,-0.130527987615796,
-1.64284471813008));
#42968=CARTESIAN_POINT('Ctrl Pts',(-0.109900563143564,-0.108455800220934,
-1.64549381523273));
#42969=CARTESIAN_POINT('Ctrl Pts',(-0.141043175077458,-0.0628300656127732,
-1.64814291233538));
#42970=CARTESIAN_POINT('Ctrl Pts',(-0.145864748164422,-0.0145744050823413,
-1.65079200943803));
#42971=CARTESIAN_POINT('Ctrl Pts',(-0.146345544565827,-0.00976245937251802,
-1.65105617143059));
#42972=CARTESIAN_POINT('Ctrl Pts',(-0.146564614324448,-0.0049243626552666,
-1.65132033342315));
#42973=CARTESIAN_POINT('Ctrl Pts',(-0.14653173368382,-8.32536397529643E-5,
-1.65158449541571));
#42974=CARTESIAN_POINT('Ctrl Pts',(-0.146557652869009,-6.33180884534729E-5,
-1.65871550458428));
#42975=CARTESIAN_POINT('Ctrl Pts',(-0.146576843604633,-0.00360111393230097,
-1.65852236952945));
#42976=CARTESIAN_POINT('Ctrl Pts',(-0.14645986789498,-0.00713761911690831,
-1.65832923447462));
#42977=CARTESIAN_POINT('Ctrl Pts',(-0.146202664286797,-0.0106638961995758,
-1.65813609941979));
#42978=CARTESIAN_POINT('Ctrl Pts',(-0.142674784100431,-0.0590313477274492,
-1.65548700231714));
#42979=CARTESIAN_POINT('Ctrl Pts',(-0.112764888693505,-0.105474517825706,
-1.65283790521449));
#42980=CARTESIAN_POINT('Ctrl Pts',(-0.0701894328195342,-0.12869491538979,
-1.65018880811184));
#42981=CARTESIAN_POINT('Ctrl Pts',(-0.0276139769455624,-0.151915312953875,
-1.64753971100919));
#42982=CARTESIAN_POINT('Ctrl Pts',(0.0276270393954554,-0.151912937983787,
-1.64489061390654));
#42983=CARTESIAN_POINT('Ctrl Pts',(0.0702004984887575,-0.128688879623078,
-1.64224151680389));
#42984=CARTESIAN_POINT('Ctrl Pts',(0.112773957582058,-0.10546482126237,
-1.63959241970124));
#42985=CARTESIAN_POINT('Ctrl Pts',(0.142679859427646,-0.0590190795110429,
-1.63694332259859));
#42986=CARTESIAN_POINT('Ctrl Pts',(0.146203580689421,-0.0106513248145528,
-1.63429422549594));
#42987=CARTESIAN_POINT('Ctrl Pts',(0.149727301951196,0.0377164298819386,
-1.63164512839329));
#42988=CARTESIAN_POINT('Ctrl Pts',(0.126868842629159,0.0880061975235912,
-1.62899603129064));
#42989=CARTESIAN_POINT('Ctrl Pts',(0.0881109215279091,0.117155466087655,
-1.62634693418799));
#42990=CARTESIAN_POINT('Ctrl Pts',(0.0493530004266599,0.146304734651718,
-1.62369783708534));
#42991=CARTESIAN_POINT('Ctrl Pts',(-0.00530438245380212,0.154313504138191,
-1.62104873998269));
#42992=CARTESIAN_POINT('Ctrl Pts',(-0.0507957593468502,0.137509012646772,
-1.61839964288004));
#42993=CARTESIAN_POINT('Ctrl Pts',(-0.0962871362398984,0.120704521155352,
-1.61575054577738));
#42994=CARTESIAN_POINT('Ctrl Pts',(-0.132612507145534,0.079086768686041,
-1.61310144867473));
#42995=CARTESIAN_POINT('Ctrl Pts',(-0.143113328138643,0.0317413458409419,
-1.61045235157208));
#42996=CARTESIAN_POINT('Ctrl Pts',(-0.145408238266455,0.0213942034161637,
-1.60987340257615));
#42997=CARTESIAN_POINT('Ctrl Pts',(-0.146469709565528,0.0107734945182561,
-1.60929445358022));
#42998=CARTESIAN_POINT('Ctrl Pts',(-0.14637109517831,0.000133274683421165,
-1.60871550458428));
#42999=CARTESIAN_POINT('Origin',(0.,0.,-1.487));
#43000=CARTESIAN_POINT('',(-0.146109700211217,1.35404246933285E-5,-1.55158449541571));
#43001=CARTESIAN_POINT('',(-0.146108968460049,-8.05953396676445E-6,-1.55871550458429));
#43002=CARTESIAN_POINT('',(-0.14635,-1.79227059055215E-17,-1.487));
#43003=CARTESIAN_POINT('Ctrl Pts',(-0.146109700211217,1.35404246933285E-5,
-1.55158449541571));
#43004=CARTESIAN_POINT('Ctrl Pts',(-0.146129167206823,0.023644608817299,
-1.55286450152468));
#43005=CARTESIAN_POINT('Ctrl Pts',(-0.14072606949062,0.0472672806948128,
-1.55414450763364));
#43006=CARTESIAN_POINT('Ctrl Pts',(-0.129852420916273,0.0680241635211907,
-1.55542451374261));
#43007=CARTESIAN_POINT('Ctrl Pts',(-0.107348347903067,0.110982550805601,
-1.55807361084526));
#43008=CARTESIAN_POINT('Ctrl Pts',(-0.0614126325066573,0.141666096683144,
-1.56072270794791));
#43009=CARTESIAN_POINT('Ctrl Pts',(-0.0131110508935279,0.14600355606985,
-1.56337180505056));
#43010=CARTESIAN_POINT('Ctrl Pts',(0.0351905307196015,0.150341015456556,
-1.56602090215321));
#43011=CARTESIAN_POINT('Ctrl Pts',(0.085857978549451,0.128332388352425,
-1.56866999925586));
#43012=CARTESIAN_POINT('Ctrl Pts',(0.115655579258376,0.0900706668510009,
-1.57131909635851));
#43013=CARTESIAN_POINT('Ctrl Pts',(0.145453179967302,0.0518089453495764,
-1.57396819346116));
#43014=CARTESIAN_POINT('Ctrl Pts',(0.154380933555303,-0.0027058705491417,
-1.57661729056382));
#43015=CARTESIAN_POINT('Ctrl Pts',(0.138344638873419,-0.0484736932320802,
-1.57926638766647));
#43016=CARTESIAN_POINT('Ctrl Pts',(0.122308344191535,-0.0942415159150187,
-1.58191548476912));
#43017=CARTESIAN_POINT('Ctrl Pts',(0.081308001239765,-0.131262345382178,
-1.58456458187177));
#43018=CARTESIAN_POINT('Ctrl Pts',(0.034146061224487,-0.14255870560379,
-1.58721367897442));
#43019=CARTESIAN_POINT('Ctrl Pts',(-0.0130158787907924,-0.153855065825403,
-1.58986277607707));
#43020=CARTESIAN_POINT('Ctrl Pts',(-0.0663394158695805,-0.139426956801469,
-1.59251187317972));
#43021=CARTESIAN_POINT('Ctrl Pts',(-0.101370773972617,-0.105891001623212,
-1.59516097028237));
#43022=CARTESIAN_POINT('Ctrl Pts',(-0.129685428678273,-0.0787850302160007,
-1.59730214532682));
#43023=CARTESIAN_POINT('Ctrl Pts',(-0.146049914781562,-0.0391960198294007,
-1.59944332037126));
#43024=CARTESIAN_POINT('Ctrl Pts',(-0.146410789716796,0.000128174727319227,
-1.60158449541571));
#43025=CARTESIAN_POINT('Ctrl Pts',(-0.14637109517831,0.000133274683421165,
-1.60871550458428));
#43026=CARTESIAN_POINT('Ctrl Pts',(-0.146018479682941,-0.0379129627241524,
-1.60664535647757));
#43027=CARTESIAN_POINT('Ctrl Pts',(-0.130833434658462,-0.0762086598056477,
-1.60457520837085));
#43028=CARTESIAN_POINT('Ctrl Pts',(-0.104169489069799,-0.103139009466109,
-1.60250506026413));
#43029=CARTESIAN_POINT('Ctrl Pts',(-0.0700485579272628,-0.137600848707174,
-1.59985596316148));
#43030=CARTESIAN_POINT('Ctrl Pts',(-0.017130424561609,-0.153451433968415,
-1.59720686605883));
#43031=CARTESIAN_POINT('Ctrl Pts',(0.0303170501043716,-0.143421805175092,
-1.59455776895618));
#43032=CARTESIAN_POINT('Ctrl Pts',(0.0777645247703496,-0.13339217638177,
-1.59190867185353));
#43033=CARTESIAN_POINT('Ctrl Pts',(0.119741340736654,-0.0974823335338879,
-1.58925957475088));
#43034=CARTESIAN_POINT('Ctrl Pts',(0.136997243561903,-0.052160262491227,
-1.58661047764823));
#43035=CARTESIAN_POINT('Ctrl Pts',(0.154253146387154,-0.00683819144856339,
-1.58396138054558));
#43036=CARTESIAN_POINT('Ctrl Pts',(0.146788136071344,0.0478961077888828,
-1.58131228344293));
#43037=CARTESIAN_POINT('Ctrl Pts',(0.118025610618323,0.0869418941873539,
-1.57866318634028));
#43038=CARTESIAN_POINT('Ctrl Pts',(0.0892630851653034,0.125987680585823,
-1.57601408923763));
#43039=CARTESIAN_POINT('Ctrl Pts',(0.0392030445750755,0.149344954145322,
-1.57336499213497));
#43040=CARTESIAN_POINT('Ctrl Pts',(-0.00919735024045918,0.146302243575645,
-1.57071589503232));
#43041=CARTESIAN_POINT('Ctrl Pts',(-0.0575977450559952,0.143259533005969,
-1.56806679792967));
#43042=CARTESIAN_POINT('Ctrl Pts',(-0.104338494096836,0.113816838307116,
-1.56541770082703));
#43043=CARTESIAN_POINT('Ctrl Pts',(-0.127984638776814,0.0714763594755748,
-1.56276860372438));
#43044=CARTESIAN_POINT('Ctrl Pts',(-0.14004411476116,0.0498828187717894,
-1.56141757067768));
#43045=CARTESIAN_POINT('Ctrl Pts',(-0.146096741734407,0.0249345965739106,
-1.56006653763098));
#43046=CARTESIAN_POINT('Ctrl Pts',(-0.146108968460049,-8.05953396676445E-6,
-1.55871550458429));
#43047=CARTESIAN_POINT('Origin',(0.,0.,-1.487));
#43048=CARTESIAN_POINT('',(-0.146360964522871,-0.000133965814129389,-1.50158449541571));
#43049=CARTESIAN_POINT('',(-0.146400754326123,-0.000129830579301018,-1.50871550458428));
#43050=CARTESIAN_POINT('',(-0.14635,-1.79227059055215E-17,-1.487));
#43051=CARTESIAN_POINT('Ctrl Pts',(-0.146360964522871,-0.000133965814129389,
-1.50158449541571));
#43052=CARTESIAN_POINT('Ctrl Pts',(-0.146011950827357,0.0375870817956262,
-1.50363658557544));
#43053=CARTESIAN_POINT('Ctrl Pts',(-0.131118218928743,0.0755527203925127,
-1.50568867573517));
#43054=CARTESIAN_POINT('Ctrl Pts',(-0.104869208528632,0.102427472599654,
-1.5077407658949));
#43055=CARTESIAN_POINT('Ctrl Pts',(-0.0709836713514958,0.137120796315871,
-1.51038986299755));
#43056=CARTESIAN_POINT('Ctrl Pts',(-0.0181746687979467,0.153331261636109,
-1.5130389601002));
#43057=CARTESIAN_POINT('Ctrl Pts',(0.0293399847849844,0.143624870177109,
-1.51568805720285));
#43058=CARTESIAN_POINT('Ctrl Pts',(0.0768546383679142,0.13391847871811,
-1.5183371543055));
#43059=CARTESIAN_POINT('Ctrl Pts',(0.119074942980225,0.0982952304798761,
-1.52098625140815));
#43060=CARTESIAN_POINT('Ctrl Pts',(0.136638982105141,0.0530916811736593,
-1.52363534851081));
#43061=CARTESIAN_POINT('Ctrl Pts',(0.154203021230057,0.00788813186744377,
-1.52628444561345));
#43062=CARTESIAN_POINT('Ctrl Pts',(0.147110794867578,-0.0468957185067564,
-1.5289335427161));
#43063=CARTESIAN_POINT('Ctrl Pts',(0.118614745083421,-0.0861364051337745,
-1.53158263981876));
#43064=CARTESIAN_POINT('Ctrl Pts',(0.0901186952992629,-0.125377091760793,
-1.53423173692141));
#43065=CARTESIAN_POINT('Ctrl Pts',(0.0402188220934277,-0.149074614640631,
-1.53688083402406));
#43066=CARTESIAN_POINT('Ctrl Pts',(-0.00820116518900179,-0.146361466684771,
-1.53952993112671));
#43067=CARTESIAN_POINT('Ctrl Pts',(-0.056621152471434,-0.14364831872891,
-1.54217902822936));
#43068=CARTESIAN_POINT('Ctrl Pts',(-0.103561253830459,-0.114524499937346,
-1.54482812533201));
#43069=CARTESIAN_POINT('Ctrl Pts',(-0.12749508919497,-0.0723459761959237,
-1.54747722243466));
#43070=CARTESIAN_POINT('Ctrl Pts',(-0.139864435116293,-0.0505475162891599,
-1.54884631342834));
#43071=CARTESIAN_POINT('Ctrl Pts',(-0.146088878366562,-0.0252621849650469,
-1.55021540442203));
#43072=CARTESIAN_POINT('Ctrl Pts',(-0.146109700211217,1.35404246933285E-5,
-1.55158449541571));
#43073=CARTESIAN_POINT('Ctrl Pts',(-0.146108968460049,-8.05953396676445E-6,
-1.55871550458429));
#43074=CARTESIAN_POINT('Ctrl Pts',(-0.146120715821164,-0.0239728066826975,
-1.55741744052833));
#43075=CARTESIAN_POINT('Ctrl Pts',(-0.140556421379631,-0.0479324156370611,
-1.55611937647238));
#43076=CARTESIAN_POINT('Ctrl Pts',(-0.129386327461104,-0.0689065743803954,
-1.55482131241642));
#43077=CARTESIAN_POINT('Ctrl Pts',(-0.106590331146305,-0.111710766440592,
-1.55217221531377));
#43078=CARTESIAN_POINT('Ctrl Pts',(-0.0604467981975962,-0.142080887596758,
-1.54952311821112));
#43079=CARTESIAN_POINT('Ctrl Pts',(-0.0121168083595676,-0.146089427002404,
-1.54687402110847));
#43080=CARTESIAN_POINT('Ctrl Pts',(0.0362131814784611,-0.150097966408049,
-1.54422492400582));
#43081=CARTESIAN_POINT('Ctrl Pts',(0.0867296282058091,-0.127744924063173,
-1.54157582690317));
#43082=CARTESIAN_POINT('Ctrl Pts',(0.116266066463203,-0.0892812383196336,
-1.53892672980052));
#43083=CARTESIAN_POINT('Ctrl Pts',(0.145802504720596,-0.0508175525760944,
-1.53627763269787));
#43084=CARTESIAN_POINT('Ctrl Pts',(0.154358934508036,0.00375677656610807,
-1.53362853559522));
#43085=CARTESIAN_POINT('Ctrl Pts',(0.13801144099953,0.0494143691647103,
-1.53097943849257));
#43086=CARTESIAN_POINT('Ctrl Pts',(0.121663947491025,0.0950719617633139,
-1.52833034138992));
#43087=CARTESIAN_POINT('Ctrl Pts',(0.080412530686573,0.131812817818317,
-1.52568124428727));
#43088=CARTESIAN_POINT('Ctrl Pts',(0.0331747823871046,0.142787855016739,
-1.52303214718461));
#43089=CARTESIAN_POINT('Ctrl Pts',(-0.0140629659123612,0.153762892215161,
-1.52038305008196));
#43090=CARTESIAN_POINT('Ctrl Pts',(-0.0672870457068432,0.138972110557006,
-1.51773395297932));
#43091=CARTESIAN_POINT('Ctrl Pts',(-0.102089291325209,0.105198452096168,
-1.51508485587667));
#43092=CARTESIAN_POINT('Ctrl Pts',(-0.129981527751131,0.0781305761582737,
-1.51296173877921));
#43093=CARTESIAN_POINT('Ctrl Pts',(-0.146041032707425,0.0388695992739819,
-1.51083862168174));
#43094=CARTESIAN_POINT('Ctrl Pts',(-0.146400754326123,-0.000129830579301018,
-1.50871550458428));
#43095=CARTESIAN_POINT('Origin',(0.,0.,-1.487));
#43096=CARTESIAN_POINT('',(-0.146563252594768,5.78712481600838E-5,-1.45158449541571));
#43097=CARTESIAN_POINT('',(-0.146538870035492,7.8428438803138E-5,-1.45871550458428));
#43098=CARTESIAN_POINT('',(-0.14635,-1.79227059055215E-17,-1.487));
#43099=CARTESIAN_POINT('Ctrl Pts',(-0.146563252594768,5.78712481600838E-5,
-1.45158449541571));
#43100=CARTESIAN_POINT('Ctrl Pts',(-0.146579365056784,0.00326456151995294,
-1.45175957252355));
#43101=CARTESIAN_POINT('Ctrl Pts',(-0.146483262220459,0.00647026841391055,
-1.4519346496314));
#43102=CARTESIAN_POINT('Ctrl Pts',(-0.146271873409478,0.00966835507499523,
-1.45210972673924));
#43103=CARTESIAN_POINT('Ctrl Pts',(-0.143073342810017,0.0580587026896339,
-1.45475882384189));
#43104=CARTESIAN_POINT('Ctrl Pts',(-0.113480308324777,0.104704412530463,
-1.45740792094454));
#43105=CARTESIAN_POINT('Ctrl Pts',(-0.0710639146539858,0.128214110278961,
-1.46005701804719));
#43106=CARTESIAN_POINT('Ctrl Pts',(-0.0286475209831971,0.151723808027457,
-1.46270611514984));
#43107=CARTESIAN_POINT('Ctrl Pts',(0.0265922318731414,0.152097493683626,
-1.46535521225249));
#43108=CARTESIAN_POINT('Ctrl Pts',(0.0693228056249136,0.129163797795145,
-1.46800430935514));
#43109=CARTESIAN_POINT('Ctrl Pts',(0.112053379376688,0.106230101906662,
-1.47065340645779));
#43110=CARTESIAN_POINT('Ctrl Pts',(0.142274774023895,0.0599890244735269,
-1.47330250356044));
#43111=CARTESIAN_POINT('Ctrl Pts',(0.146127683586795,0.0116463784127105,
-1.4759516006631));
#43112=CARTESIAN_POINT('Ctrl Pts',(0.149980593149695,-0.0366962676481046,
-1.47860069776575));
#43113=CARTESIAN_POINT('Ctrl Pts',(0.12746501762829,-0.0871404823366008,
-1.4812497948684));
#43114=CARTESIAN_POINT('Ctrl Pts',(0.0889064318758686,-0.116552925367303,
-1.48389889197105));
#43115=CARTESIAN_POINT('Ctrl Pts',(0.0503478461234483,-0.145965368398004,
-1.4865479890737));
#43116=CARTESIAN_POINT('Ctrl Pts',(-0.00425374985998689,-0.154346039770913,
-1.48919708617635));
#43117=CARTESIAN_POINT('Ctrl Pts',(-0.0498584717623352,-0.13785162615689,
-1.491846183279));
#43118=CARTESIAN_POINT('Ctrl Pts',(-0.0954631936646862,-0.121357212542867,
-1.49449528038165));
#43119=CARTESIAN_POINT('Ctrl Pts',(-0.132071041485949,-0.0799877139419083,
-1.4971443774843));
#43120=CARTESIAN_POINT('Ctrl Pts',(-0.142893929496219,-0.0327148735853313,
-1.49979347458695));
#43121=CARTESIAN_POINT('Ctrl Pts',(-0.145333001766583,-0.022061351720772,
-1.50039048152987));
#43122=CARTESIAN_POINT('Ctrl Pts',(-0.146462501776685,-0.0111080096252457,
-1.50098748847279));
#43123=CARTESIAN_POINT('Ctrl Pts',(-0.146360964522871,-0.000133965814129389,
-1.50158449541571));
#43124=CARTESIAN_POINT('Ctrl Pts',(-0.146400754326123,-0.000129830579301018,
-1.50871550458428));
#43125=CARTESIAN_POINT('Ctrl Pts',(-0.146489871586351,-0.00979153051154047,
-1.50818952457909));
#43126=CARTESIAN_POINT('Ctrl Pts',(-0.145615416708744,-0.0194371780291451,
-1.5076635445739));
#43127=CARTESIAN_POINT('Ctrl Pts',(-0.143718591245809,-0.0288774004549093,
-1.50713756456871));
#43128=CARTESIAN_POINT('Ctrl Pts',(-0.134165234105791,-0.0764230592816198,
-1.50448846746606));
#43129=CARTESIAN_POINT('Ctrl Pts',(-0.0986781083835066,-0.118757841671515,
-1.50183937036341));
#43130=CARTESIAN_POINT('Ctrl Pts',(-0.0535313450205615,-0.136467332453605,
-1.49919027326076));
#43131=CARTESIAN_POINT('Ctrl Pts',(-0.00838458165761895,-0.154176823235693,
-1.49654117615811));
#43132=CARTESIAN_POINT('Ctrl Pts',(0.0464218193459839,-0.147261022409979,
-1.49389207905546));
#43133=CARTESIAN_POINT('Ctrl Pts',(0.0857540516247829,-0.11889146460805,
-1.49124298195281));
#43134=CARTESIAN_POINT('Ctrl Pts',(0.125086283903585,-0.0905219068061183,
-1.48859388485016));
#43135=CARTESIAN_POINT('Ctrl Pts',(0.148944347457581,-0.0406985920279711,
-1.48594478774751));
#43136=CARTESIAN_POINT('Ctrl Pts',(0.146387112443533,0.00772987950473067,
-1.48329569064486));
#43137=CARTESIAN_POINT('Ctrl Pts',(0.143829877429484,0.0561583510374297,
-1.48064659354221));
#43138=CARTESIAN_POINT('Ctrl Pts',(0.114857343847392,0.103191979324682,
-1.47799749643956));
#43139=CARTESIAN_POINT('Ctrl Pts',(0.0727560993153952,0.127261493544282,
-1.47534839933691));
#43140=CARTESIAN_POINT('Ctrl Pts',(0.0306548547833984,0.151331007763883,
-1.47269930223425));
#43141=CARTESIAN_POINT('Ctrl Pts',(-0.0245751006985043,0.152436407915832,
-1.4700502051316));
#43142=CARTESIAN_POINT('Ctrl Pts',(-0.067605721842972,0.13007076574236,
-1.46740110802895));
#43143=CARTESIAN_POINT('Ctrl Pts',(-0.11063634298744,0.107705123568887,
-1.4647520109263));
#43144=CARTESIAN_POINT('Ctrl Pts',(-0.141467629794474,0.0618684390699918,
-1.46210291382365));
#43145=CARTESIAN_POINT('Ctrl Pts',(-0.14596058429274,0.0135810735818327,
-1.459453816721));
#43146=CARTESIAN_POINT('Ctrl Pts',(-0.146377984726076,0.00909512401630342,
-1.45920771267543));
#43147=CARTESIAN_POINT('Ctrl Pts',(-0.146568069149991,0.00458802356634012,
-1.45896160862986));
#43148=CARTESIAN_POINT('Ctrl Pts',(-0.146538870035492,7.8428438803138E-5,
-1.45871550458428));
#43149=CARTESIAN_POINT('Origin',(0.,0.,-1.487));
#43150=CARTESIAN_POINT('',(-0.146186144827487,0.00010175201331792,-1.40158449541571));
#43151=CARTESIAN_POINT('',(-0.14616050398721,8.61805021221069E-5,-1.40871550458428));
#43152=CARTESIAN_POINT('',(-0.14635,-1.79227059055215E-17,-1.487));
#43153=CARTESIAN_POINT('Ctrl Pts',(-0.146186144827487,0.00010175201331792,
-1.40158449541571));
#43154=CARTESIAN_POINT('Ctrl Pts',(-0.146297791485825,0.0175650700753052,
-1.40253165657432));
#43155=CARTESIAN_POINT('Ctrl Pts',(-0.143405387297582,0.0349926282668302,
-1.40347881773292));
#43156=CARTESIAN_POINT('Ctrl Pts',(-0.137344752713405,0.0512382371151499,
-1.40442597889153));
#43157=CARTESIAN_POINT('Ctrl Pts',(-0.12039387865013,0.0966752727661706,
-1.40707507599418));
#43158=CARTESIAN_POINT('Ctrl Pts',(-0.078659384026827,0.132866458089903,
-1.40972417309683));
#43159=CARTESIAN_POINT('Ctrl Pts',(-0.0312803965259292,0.143214785667386,
-1.41237327019948));
#43160=CARTESIAN_POINT('Ctrl Pts',(0.0160985909749686,0.153563113244869,
-1.41502236730213));
#43161=CARTESIAN_POINT('Ctrl Pts',(0.0691220713534613,0.138068583076103,
-1.41767146440478));
#43162=CARTESIAN_POINT('Ctrl Pts',(0.103473872333095,0.103836871028401,
-1.42032056150743));
#43163=CARTESIAN_POINT('Ctrl Pts',(0.137825673312729,0.0696051589807,-1.42296965861008));
#43164=CARTESIAN_POINT('Ctrl Pts',(0.153505794893504,0.0166362650540631,
-1.42561875571273));
#43165=CARTESIAN_POINT('Ctrl Pts',(0.143323450372017,-0.0307786714143838,
-1.42826785281539));
#43166=CARTESIAN_POINT('Ctrl Pts',(0.133141105850529,-0.078193607882832,
-1.43091694991804));
#43167=CARTESIAN_POINT('Ctrl Pts',(0.0970962952267766,-0.12005458689309,
-1.43356604702069));
#43168=CARTESIAN_POINT('Ctrl Pts',(0.0517188995750107,-0.137164475967083,
-1.43621514412334));
#43169=CARTESIAN_POINT('Ctrl Pts',(0.00634150392324483,-0.154274365041076,
-1.43886424122599));
#43170=CARTESIAN_POINT('Ctrl Pts',(-0.0483684767565346,-0.146633164178805,
-1.44151333832864));
#43171=CARTESIAN_POINT('Ctrl Pts',(-0.0873214537395813,-0.117745071053445,
-1.44416243543129));
#43172=CARTESIAN_POINT('Ctrl Pts',(-0.12370005376028,-0.0907661732499322,
-1.4466364554261));
#43173=CARTESIAN_POINT('Ctrl Pts',(-0.146335566898538,-0.0452559675928817,
-1.4491104754209));
#43174=CARTESIAN_POINT('Ctrl Pts',(-0.146563252594768,5.78712481600838E-5,
-1.45158449541571));
#43175=CARTESIAN_POINT('Ctrl Pts',(-0.146538870035492,7.8428438803138E-5,
-1.45871550458428));
#43176=CARTESIAN_POINT('Ctrl Pts',(-0.146253765947706,-0.0439538659368936,
-1.45631251152721));
#43177=CARTESIAN_POINT('Ctrl Pts',(-0.125062536189296,-0.0882239986986389,
-1.45390951847013));
#43178=CARTESIAN_POINT('Ctrl Pts',(-0.0904425780473909,-0.11536497650004,
-1.45150652541305));
#43179=CARTESIAN_POINT('Ctrl Pts',(-0.0522769951142755,-0.145285614616334,
-1.4488574283104));
#43180=CARTESIAN_POINT('Ctrl Pts',(0.00220879294145686,-0.154388844371495,
-1.44620833120775));
#43181=CARTESIAN_POINT('Ctrl Pts',(0.0480280104588239,-0.138499992556246,
-1.4435592341051));
#43182=CARTESIAN_POINT('Ctrl Pts',(0.0938472279761883,-0.122611140740998,
-1.44091013700245));
#43183=CARTESIAN_POINT('Ctrl Pts',(0.130999874955191,-0.081730207355346,
-1.4382610398998));
#43184=CARTESIAN_POINT('Ctrl Pts',(0.142448024839166,-0.0346048832700464,
-1.43561194279715));
#43185=CARTESIAN_POINT('Ctrl Pts',(0.153896174723141,0.0125204408152545,
-1.4329628456945));
#43186=CARTESIAN_POINT('Ctrl Pts',(0.139639827512083,0.0658901556002054,
-1.43031374859185));
#43187=CARTESIAN_POINT('Ctrl Pts',(0.106216837612053,0.101029308294217,
-1.4276646514892));
#43188=CARTESIAN_POINT('Ctrl Pts',(0.0727938477120221,0.136168460988228,
-1.42501555438655));
#43189=CARTESIAN_POINT('Ctrl Pts',(0.0202042151230188,0.153077051591303,
-1.4223664572839));
#43190=CARTESIAN_POINT('Ctrl Pts',(-0.0274348472360513,0.144000926677045,
-1.41971736018125));
#43191=CARTESIAN_POINT('Ctrl Pts',(-0.0750739095951214,0.134924801762786,
-1.41706826307859));
#43192=CARTESIAN_POINT('Ctrl Pts',(-0.117762401724257,0.0998639613311952,
-1.41441916597594));
#43193=CARTESIAN_POINT('Ctrl Pts',(-0.135923699806529,0.0548970450718224,
-1.41177006887329));
#43194=CARTESIAN_POINT('Ctrl Pts',(-0.142904046998363,0.0376138813786416,
-1.41075188077696));
#43195=CARTESIAN_POINT('Ctrl Pts',(-0.146261062082397,0.0188673214836565,
-1.40973369268062));
#43196=CARTESIAN_POINT('Ctrl Pts',(-0.14616050398721,8.61805021221068E-5,
-1.40871550458428));
#43197=CARTESIAN_POINT('Origin',(0.,0.,-1.487));
#43198=CARTESIAN_POINT('',(-0.146193053794332,-0.000105164914211059,-1.35158449541571));
#43199=CARTESIAN_POINT('',(-0.146223843614078,-0.00011741876304885,-1.35871550458429));
#43200=CARTESIAN_POINT('',(-0.14635,-1.79227059055215E-17,-1.487));
#43201=CARTESIAN_POINT('Ctrl Pts',(-0.146193053794332,-0.000105164914211059,
-1.35158449541571));
#43202=CARTESIAN_POINT('Ctrl Pts',(-0.145982970582079,0.0315897173710793,
-1.35330374062508));
#43203=CARTESIAN_POINT('Ctrl Pts',(-0.135864273539381,0.0634067802567858,
-1.35502298583445));
#43204=CARTESIAN_POINT('Ctrl Pts',(-0.11686355797358,0.0884977223341386,
-1.35674223104382));
#43205=CARTESIAN_POINT('Ctrl Pts',(-0.0875863261515443,0.127159073023167,
-1.35939132814647));
#43206=CARTESIAN_POINT('Ctrl Pts',(-0.0372212695608701,0.149851164403594,
-1.36204042524912));
#43207=CARTESIAN_POINT('Ctrl Pts',(0.0111345728257042,0.146167572766889,
-1.36468952235177));
#43208=CARTESIAN_POINT('Ctrl Pts',(0.0594904152122772,0.142483981130183,
-1.36733861945442));
#43209=CARTESIAN_POINT('Ctrl Pts',(0.105837043394752,0.112424706476348,
-1.36998771655707));
#43210=CARTESIAN_POINT('Ctrl Pts',(0.128920239670456,0.0697747077664019,
-1.37263681365972));
#43211=CARTESIAN_POINT('Ctrl Pts',(0.152003435946159,0.0271247090564568,
-1.37528591076238));
#43212=CARTESIAN_POINT('Ctrl Pts',(0.151823200315095,-0.0281160137095958,
-1.37793500786503));
#43213=CARTESIAN_POINT('Ctrl Pts',(0.128462187492193,-0.0706144774482909,
-1.38058410496768));
#43214=CARTESIAN_POINT('Ctrl Pts',(0.10510117466929,-0.113112941186989,
-1.38323320207033));
#43215=CARTESIAN_POINT('Ctrl Pts',(0.0585593846545423,-0.142869145898326,
-1.38588229917298));
#43216=CARTESIAN_POINT('Ctrl Pts',(0.0101805349100076,-0.146237118234464,
-1.38853139627563));
#43217=CARTESIAN_POINT('Ctrl Pts',(-0.0381983148345271,-0.149605090570603,
-1.39118049337828));
#43218=CARTESIAN_POINT('Ctrl Pts',(-0.0884142243088482,-0.126584830531547,
-1.39382959048093));
#43219=CARTESIAN_POINT('Ctrl Pts',(-0.117438552294387,-0.0877332575228631,
-1.39647868758358));
#43220=CARTESIAN_POINT('Ctrl Pts',(-0.136085489396421,-0.06277271963999,
-1.39818062352762));
#43221=CARTESIAN_POINT('Ctrl Pts',(-0.145985529062017,-0.0312777534086356,
-1.39988255947167));
#43222=CARTESIAN_POINT('Ctrl Pts',(-0.146186144827487,0.00010175201331792,
-1.40158449541571));
#43223=CARTESIAN_POINT('Ctrl Pts',(-0.14616050398721,8.61805021221068E-5,
-1.40871550458428));
#43224=CARTESIAN_POINT('Ctrl Pts',(-0.145999432468413,-0.029996995765469,
-1.40708459557797));
#43225=CARTESIAN_POINT('Ctrl Pts',(-0.136967315343511,-0.0601688962277433,
-1.40545368657166));
#43226=CARTESIAN_POINT('Ctrl Pts',(-0.119745364280119,-0.0845575866503699,
-1.40382277756534));
#43227=CARTESIAN_POINT('Ctrl Pts',(-0.0917716266360291,-0.124172310026032,
-1.40117368046269));
#43228=CARTESIAN_POINT('Ctrl Pts',(-0.0421900473124433,-0.148528764690202,
-1.39852458336004));
#43229=CARTESIAN_POINT('Ctrl Pts',(0.00626163154385964,-0.146457262357051,
-1.39587548625739));
#43230=CARTESIAN_POINT('Ctrl Pts',(0.0547133104001626,-0.1443857600239,
-1.39322638915474));
#43231=CARTESIAN_POINT('Ctrl Pts',(0.102035088789183,-0.115886300693427,
-1.39057729205209));
#43232=CARTESIAN_POINT('Ctrl Pts',(0.126525552403112,-0.0740285236635203,
-1.38792819494944));
#43233=CARTESIAN_POINT('Ctrl Pts',(0.151016016017042,-0.032170746633614,
-1.38527909784679));
#43234=CARTESIAN_POINT('Ctrl Pts',(0.152675164855881,0.0230453480957256,
-1.38263000074414));
#43235=CARTESIAN_POINT('Ctrl Pts',(0.130742125647836,0.0662980716748126,
-1.37998090364149));
#43236=CARTESIAN_POINT('Ctrl Pts',(0.10880908643979,0.109550795253901,-1.37733180653884));
#43237=CARTESIAN_POINT('Ctrl Pts',(0.0632838591848581,0.140840147682736,
-1.37468270943619));
#43238=CARTESIAN_POINT('Ctrl Pts',(0.0150439732521744,0.145817065515326,
-1.37203361233353));
#43239=CARTESIAN_POINT('Ctrl Pts',(-0.0331959126805066,0.150793983347916,
-1.36938451523088));
#43240=CARTESIAN_POINT('Ctrl Pts',(-0.0841504572909391,0.129458466584265,
-1.36673541812823));
#43241=CARTESIAN_POINT('Ctrl Pts',(-0.114452286801109,0.0915948239406019,
-1.36408632102558));
#43242=CARTESIAN_POINT('Ctrl Pts',(-0.134930404165678,0.0660063980784996,
-1.36229604887848));
#43243=CARTESIAN_POINT('Ctrl Pts',(-0.145976180189185,0.0328693799721589,
-1.36050577673138));
#43244=CARTESIAN_POINT('Ctrl Pts',(-0.146223843614078,-0.00011741876304885,
-1.35871550458429));
#43245=CARTESIAN_POINT('Origin',(0.,0.,-1.487));
#43246=CARTESIAN_POINT('',(-0.146568201272772,-5.25249794677829E-5,-1.30158449541571));
#43247=CARTESIAN_POINT('',(-0.146583801498189,-2.95221421093228E-5,-1.30871550458428));
#43248=CARTESIAN_POINT('',(-0.14635,-1.79227059055215E-17,-1.487));
#43249=CARTESIAN_POINT('Ctrl Pts',(-0.146568201272772,-5.25249794677829E-5,
-1.30158449541571));
#43250=CARTESIAN_POINT('Ctrl Pts',(-0.146357355089256,0.0455742536737809,
-1.30407582467584));
#43251=CARTESIAN_POINT('Ctrl Pts',(-0.123360881151597,0.0913843415984147,
-1.30656715393598));
#43252=CARTESIAN_POINT('Ctrl Pts',(-0.0865512617525035,0.118312370991474,
-1.30905848319611));
#43253=CARTESIAN_POINT('Ctrl Pts',(-0.0474106079416224,0.146945665589161,
-1.31170758029876));
#43254=CARTESIAN_POINT('Ctrl Pts',(0.00734806976815248,0.154229699641535,
-1.31435667740141));
#43255=CARTESIAN_POINT('Ctrl Pts',(0.0526128505576494,0.136824069508157,
-1.31700577450406));
#43256=CARTESIAN_POINT('Ctrl Pts',(0.0978776313471463,0.119418439374779,
-1.31965487160671));
#43257=CARTESIAN_POINT('Ctrl Pts',(0.133648515216364,0.0773231450556503,
-1.32230396870936));
#43258=CARTESIAN_POINT('Ctrl Pts',(0.143521241855794,0.0298427742803053,
-1.32495306581201));
#43259=CARTESIAN_POINT('Ctrl Pts',(0.153393968495224,-0.0176375964950385,
-1.32760216291466));
#43260=CARTESIAN_POINT('Ctrl Pts',(0.137368537904866,-0.0705030437266001,
-1.33025126001732));
#43261=CARTESIAN_POINT('Ctrl Pts',(0.102794092922157,-0.104509867959372,
-1.33290035711997));
#43262=CARTESIAN_POINT('Ctrl Pts',(0.0682196479394476,-0.138516692192145,
-1.33554945422262));
#43263=CARTESIAN_POINT('Ctrl Pts',(0.0150961885643901,-0.15366489342613,
-1.33819855132527));
#43264=CARTESIAN_POINT('Ctrl Pts',(-0.0322142633050966,-0.14300761965813,
-1.34084764842792));
#43265=CARTESIAN_POINT('Ctrl Pts',(-0.0795247151745847,-0.13235034589013,
-1.34349674553057));
#43266=CARTESIAN_POINT('Ctrl Pts',(-0.1210221595385,-0.095887597120137,
-1.34614584263322));
#43267=CARTESIAN_POINT('Ctrl Pts',(-0.137676178193757,-0.0503409177363263,
-1.34879493973587));
#43268=CARTESIAN_POINT('Ctrl Pts',(-0.143521856995724,-0.0343537098626333,
-1.34972479162915));
#43269=CARTESIAN_POINT('Ctrl Pts',(-0.146306677070172,-0.0172473073728051,
-1.35065464352243));
#43270=CARTESIAN_POINT('Ctrl Pts',(-0.146193053794332,-0.000105164914211059,
-1.35158449541571));
#43271=CARTESIAN_POINT('Ctrl Pts',(-0.146223843614078,-0.00011741876304885,
-1.35871550458429));
#43272=CARTESIAN_POINT('Ctrl Pts',(-0.146342652103738,-0.0159417648008479,
-1.35785667962873));
#43273=CARTESIAN_POINT('Ctrl Pts',(-0.143976502592481,-0.0317315410168582,
-1.35699785467318));
#43274=CARTESIAN_POINT('Ctrl Pts',(-0.138974618193963,-0.0466368226249961,
-1.35613902971763));
#43275=CARTESIAN_POINT('Ctrl Pts',(-0.123546005666741,-0.0926130580232472,
-1.35348993261498));
#43276=CARTESIAN_POINT('Ctrl Pts',(-0.0830396662023916,-0.130173760296071,
-1.35084083551233));
#43277=CARTESIAN_POINT('Ctrl Pts',(-0.0360315046957431,-0.142093871775224,
-1.34819173840968));
#43278=CARTESIAN_POINT('Ctrl Pts',(0.0109766568109053,-0.154013983254376,
-1.34554264130703));
#43279=CARTESIAN_POINT('Ctrl Pts',(0.0644866403598532,-0.140293503939857,
-1.34289354420438));
#43280=CARTESIAN_POINT('Ctrl Pts',(0.0999591669524664,-0.107224543220673,
-1.34024444710173));
#43281=CARTESIAN_POINT('Ctrl Pts',(0.135431693545081,-0.0741555825014888,
-1.33759534999908));
#43282=CARTESIAN_POINT('Ctrl Pts',(0.152866763181359,-0.021738140377639,
-1.33494625289643));
#43283=CARTESIAN_POINT('Ctrl Pts',(0.144268783080492,0.0259895354938695,
-1.33229715579378));
#43284=CARTESIAN_POINT('Ctrl Pts',(0.135670802979624,0.0737172113653767,
-1.32964805869113));
#43285=CARTESIAN_POINT('Ctrl Pts',(0.101039773141612,0.116755120984543,
-1.32699896158848));
#43286=CARTESIAN_POINT('Ctrl Pts',(0.0562572253263671,0.135366400281944,
-1.32434986448583));
#43287=CARTESIAN_POINT('Ctrl Pts',(0.0114746775111209,0.153977679579345,
-1.32170076738318));
#43288=CARTESIAN_POINT('Ctrl Pts',(-0.0434593882813584,0.14816232855498,
-1.31905167028053));
#43289=CARTESIAN_POINT('Ctrl Pts',(-0.0833526195664562,0.120587223776496,
-1.31640257317787));
#43290=CARTESIAN_POINT('Ctrl Pts',(-0.121939603914395,0.0939150264587117,
-1.31384021698001));
#43291=CARTESIAN_POINT('Ctrl Pts',(-0.146454609180979,0.046884730027936,
-1.31127786078215));
#43292=CARTESIAN_POINT('Ctrl Pts',(-0.146583801498189,-2.95221421093228E-5,
-1.30871550458428));
#43293=CARTESIAN_POINT('Origin',(0.,0.,-1.487));
#43294=CARTESIAN_POINT('',(-0.146351269115874,0.000134398057797393,-1.25158449541571));
#43295=CARTESIAN_POINT('',(-0.146311958104459,0.000133832465902105,-1.25871550458429));
#43296=CARTESIAN_POINT('',(-0.14635,-1.79227059055215E-17,-1.487));
#43297=CARTESIAN_POINT('Ctrl Pts',(-0.146351269115874,0.000134398057797393,
-1.25158449541571));
#43298=CARTESIAN_POINT('Ctrl Pts',(-0.146455439504307,0.0114285307963374,
-1.25219881162396));
#43299=CARTESIAN_POINT('Ctrl Pts',(-0.145258679634911,0.0227008231077745,
-1.2528131278322));
#43300=CARTESIAN_POINT('Ctrl Pts',(-0.142677409791644,0.0336466161110121,
-1.25342744404045));
#43301=CARTESIAN_POINT('Ctrl Pts',(-0.131546278346365,0.0808478264027943,
-1.2560765411431));
#43302=CARTESIAN_POINT('Ctrl Pts',(-0.0946692576923265,0.121977563628807,
-1.25872563824575));
#43303=CARTESIAN_POINT('Ctrl Pts',(-0.0489578742111441,0.138174037334444,
-1.2613747353484));
#43304=CARTESIAN_POINT('Ctrl Pts',(-0.00324649072996173,0.154370511040082,
-1.26402383245105));
#43305=CARTESIAN_POINT('Ctrl Pts',(0.0512992555783647,0.145633721225344,
-1.2666729295537));
#43306=CARTESIAN_POINT('Ctrl Pts',(0.0896650926458139,0.115970294478337,
-1.26932202665635));
#43307=CARTESIAN_POINT('Ctrl Pts',(0.128030929713264,0.0863068677313288,
-1.271971123759));
#43308=CARTESIAN_POINT('Ctrl Pts',(0.150216857539836,0.0357168040520492,
-1.27462022086165));
#43309=CARTESIAN_POINT('Ctrl Pts',(0.14604857524424,-0.0125996710156281,
-1.27726931796431));
#43310=CARTESIAN_POINT('Ctrl Pts',(0.141880292948645,-0.060916146083304,
-1.27991841506696));
#43311=CARTESIAN_POINT('Ctrl Pts',(0.111357800530883,-0.106959032539378,
-1.28256751216961));
#43312=CARTESIAN_POINT('Ctrl Pts',(0.0684784851605484,-0.129613406369446,
-1.28521660927226));
#43313=CARTESIAN_POINT('Ctrl Pts',(0.0255991697902121,-0.152267780199515,
-1.28786570637491));
#43314=CARTESIAN_POINT('Ctrl Pts',(-0.0296369685326984,-0.151533641403577,
-1.29051480347756));
#43315=CARTESIAN_POINT('Ctrl Pts',(-0.071899049116112,-0.127747660553035,
-1.29316390058021));
#43316=CARTESIAN_POINT('Ctrl Pts',(-0.114161129699523,-0.103961679702495,
-1.29581299768286));
#43317=CARTESIAN_POINT('Ctrl Pts',(-0.143449152543439,-0.0571238567973552,
-1.29846209478551));
#43318=CARTESIAN_POINT('Ctrl Pts',(-0.146331849009405,-0.00871366777328614,
-1.30111119188816));
#43319=CARTESIAN_POINT('Ctrl Pts',(-0.146503528938243,-0.00583058316663799,
-1.30126895973068));
#43320=CARTESIAN_POINT('Ctrl Pts',(-0.146581553481172,-0.00294192163382165,
-1.30142672757319));
#43321=CARTESIAN_POINT('Ctrl Pts',(-0.146568201272772,-5.25249794677829E-5,
-1.30158449541571));
#43322=CARTESIAN_POINT('Ctrl Pts',(-0.146583801498189,-2.95221421093228E-5,
-1.30871550458428));
#43323=CARTESIAN_POINT('Ctrl Pts',(-0.146588174917659,-0.00161766382360389,
-1.3086287636795));
#43324=CARTESIAN_POINT('Ctrl Pts',(-0.146564603207359,-0.0032056725231908,
-1.30854202277471));
#43325=CARTESIAN_POINT('Ctrl Pts',(-0.146512686262755,-0.00479275398747684,
-1.30845528186992));
#43326=CARTESIAN_POINT('Ctrl Pts',(-0.144927124896243,-0.0532627684403694,
-1.30580618476727));
#43327=CARTESIAN_POINT('Ctrl Pts',(-0.116903605385501,-0.100867938813553,
-1.30315708766462));
#43328=CARTESIAN_POINT('Ctrl Pts',(-0.0752935045800234,-0.125776889350831,
-1.30050799056197));
#43329=CARTESIAN_POINT('Ctrl Pts',(-0.0336834037745442,-0.150685839888109,
-1.29785889345932));
#43330=CARTESIAN_POINT('Ctrl Pts',(0.0215132783256708,-0.152898570589479,
-1.29520979635667));
#43331=CARTESIAN_POINT('Ctrl Pts',(0.0649837553577353,-0.13140033967353,
-1.29256069925402));
#43332=CARTESIAN_POINT('Ctrl Pts',(0.108454232389799,-0.109902108757581,
-1.28991160215137));
#43333=CARTESIAN_POINT('Ctrl Pts',(0.140198504353711,-0.0646929162243153,
-1.28726250504872));
#43334=CARTESIAN_POINT('Ctrl Pts',(0.145658885100711,-0.0165053602787354,
-1.28461340794607));
#43335=CARTESIAN_POINT('Ctrl Pts',(0.151119265847712,0.0316821956668444,
-1.28196431084342));
#43336=CARTESIAN_POINT('Ctrl Pts',(0.130295755377799,0.0828481150247396,
-1.27931521374077));
#43337=CARTESIAN_POINT('Ctrl Pts',(0.092737860143069,0.113528089135675,
-1.27666611663812));
#43338=CARTESIAN_POINT('Ctrl Pts',(0.05517996490834,0.144208063246609,-1.27401701953547));
#43339=CARTESIAN_POINT('Ctrl Pts',(0.00088768490879558,0.154402092110587,
-1.27136792243281));
#43340=CARTESIAN_POINT('Ctrl Pts',(-0.0452409455446037,0.139435270189946,
-1.26871882533016));
#43341=CARTESIAN_POINT('Ctrl Pts',(-0.0913695759980056,0.124468448269304,
-1.26606972822751));
#43342=CARTESIAN_POINT('Ctrl Pts',(-0.12933455690526,0.0843407755640405,
-1.26342063112486));
#43343=CARTESIAN_POINT('Ctrl Pts',(-0.14172543143435,0.0374545032200476,
-1.26077153402221));
#43344=CARTESIAN_POINT('Ctrl Pts',(-0.144931052293872,0.0253246400454748,
-1.26008619087624));
#43345=CARTESIAN_POINT('Ctrl Pts',(-0.146424999918828,0.0127424242477569,
-1.25940084773026));
#43346=CARTESIAN_POINT('Ctrl Pts',(-0.146311958104459,0.000133832465902105,
-1.25871550458429));
#43347=CARTESIAN_POINT('Origin',(0.,0.,-1.487));
#43348=CARTESIAN_POINT('',(-0.146110748319233,-1.87736639323394E-5,-1.20158449541571));
#43349=CARTESIAN_POINT('',(-0.146118579951279,-3.98722473775574E-5,-1.20871550458429));
#43350=CARTESIAN_POINT('',(-0.14635,-1.79227059055215E-17,-1.487));
#43351=CARTESIAN_POINT('Ctrl Pts',(-0.146110748319233,-1.87736639323394E-5,
-1.20158449541571));
#43352=CARTESIAN_POINT('Ctrl Pts',(-0.146081502410529,0.0255760520854927,
-1.20297089567472));
#43353=CARTESIAN_POINT('Ctrl Pts',(-0.139689794215594,0.0511845413353593,
-1.20435729593373));
#43354=CARTESIAN_POINT('Ctrl Pts',(-0.127020288822047,0.0731763914670449,
-1.20574369619274));
#43355=CARTESIAN_POINT('Ctrl Pts',(-0.102811731580409,0.115197839520859,
-1.20839279329539));
#43356=CARTESIAN_POINT('Ctrl Pts',(-0.0556825852416403,0.144014735640639,
-1.21104189039804));
#43357=CARTESIAN_POINT('Ctrl Pts',(-0.00724592449332075,0.146411866386614,
-1.21369098750069));
#43358=CARTESIAN_POINT('Ctrl Pts',(0.0411907362549988,0.148808997132589,
-1.21634008460334));
#43359=CARTESIAN_POINT('Ctrl Pts',(0.090934911412867,0.124786362504761,
-1.21898918170599));
#43360=CARTESIAN_POINT('Ctrl Pts',(0.119174293597701,0.0853605634122892,
-1.22163827880864));
#43361=CARTESIAN_POINT('Ctrl Pts',(0.147413675782537,0.0459347643198159,
-1.22428737591129));
#43362=CARTESIAN_POINT('Ctrl Pts',(0.154148264994333,-0.00889419923730254,
-1.22693647301394));
#43363=CARTESIAN_POINT('Ctrl Pts',(0.136289628894883,-0.0539821738749891,
-1.2295855701166));
#43364=CARTESIAN_POINT('Ctrl Pts',(0.118430992795435,-0.0990701485126745,
-1.23223466721925));
#43365=CARTESIAN_POINT('Ctrl Pts',(0.0759791313847414,-0.13441713423093,
-1.2348837643219));
#43366=CARTESIAN_POINT('Ctrl Pts',(0.0284021513987267,-0.143813267247839,
-1.23753286142455));
#43367=CARTESIAN_POINT('Ctrl Pts',(-0.0191748285872881,-0.153209400264748,
-1.2401819585272));
#43368=CARTESIAN_POINT('Ctrl Pts',(-0.0718769271486259,-0.136654680580311,
-1.24283105562985));
#43369=CARTESIAN_POINT('Ctrl Pts',(-0.105535355311034,-0.101740979059317,
-1.2454801527325));
#43370=CARTESIAN_POINT('Ctrl Pts',(-0.131388513540689,-0.0749236409040759,
-1.2475149336269));
#43371=CARTESIAN_POINT('Ctrl Pts',(-0.146006228706228,-0.0372748143425158,
-1.24954971452131));
#43372=CARTESIAN_POINT('Ctrl Pts',(-0.146351269115874,0.000134398057797393,
-1.25158449541571));
#43373=CARTESIAN_POINT('Ctrl Pts',(-0.146311958104459,0.000133832465902105,
-1.25871550458429));
#43374=CARTESIAN_POINT('Ctrl Pts',(-0.1459880527564,-0.0359943058909224,
-1.25675175062761));
#43375=CARTESIAN_POINT('Ctrl Pts',(-0.132470313237583,-0.0723389984778341,
-1.25478799667094));
#43376=CARTESIAN_POINT('Ctrl Pts',(-0.108221467599082,-0.0988789749007037,
-1.25282424271426));
#43377=CARTESIAN_POINT('Ctrl Pts',(-0.0755098610837993,-0.134681308694744,
-1.25017514561161));
#43378=CARTESIAN_POINT('Ctrl Pts',(-0.023269879902309,-0.152641104300106,
-1.24752604850896));
#43379=CARTESIAN_POINT('Ctrl Pts',(0.0245416105517876,-0.144522133523684,
-1.24487695140631));
#43380=CARTESIAN_POINT('Ctrl Pts',(0.0723531010058841,-0.136403162747262,
-1.24222785430366));
#43381=CARTESIAN_POINT('Ctrl Pts',(0.115736100732587,-0.102205425589056,
-1.23957875720101));
#43382=CARTESIAN_POINT('Ctrl Pts',(0.134795489915285,-0.0576117490205896,
-1.23692966009836));
#43383=CARTESIAN_POINT('Ctrl Pts',(0.153854879097983,-0.0130180724521228,
-1.23428056299571));
#43384=CARTESIAN_POINT('Ctrl Pts',(0.148590657736676,0.0419715435266052,
-1.23163146589306));
#43385=CARTESIAN_POINT('Ctrl Pts',(0.121416958449766,0.0821392715302546,
-1.22898236879041));
#43386=CARTESIAN_POINT('Ctrl Pts',(0.0942432591628547,0.122306999533906,
-1.22633327168776));
#43387=CARTESIAN_POINT('Ctrl Pts',(0.0451600819503379,0.147652839562477,
-1.2236841745851));
#43388=CARTESIAN_POINT('Ctrl Pts',(-0.00332339452852188,0.146553378587874,
-1.22103507748245));
#43389=CARTESIAN_POINT('Ctrl Pts',(-0.0518068710073776,0.145453917613272,
-1.2183859803798));
#43390=CARTESIAN_POINT('Ctrl Pts',(-0.0996906467525764,0.1179091556355,
-1.21573688327715));
#43391=CARTESIAN_POINT('Ctrl Pts',(-0.12501557966413,0.0765509148734009,
-1.2130877861745));
#43392=CARTESIAN_POINT('Ctrl Pts',(-0.138948344130923,0.0537972661544986,
-1.21163035897776));
#43393=CARTESIAN_POINT('Ctrl Pts',(-0.146053088318131,0.0268626089518478,
-1.21017293178102));
#43394=CARTESIAN_POINT('Ctrl Pts',(-0.146118579951279,-3.98722473775574E-5,
-1.20871550458429));
#43395=CARTESIAN_POINT('Origin',(0.,0.,-1.487));
#43396=CARTESIAN_POINT('',(-0.146420343877387,-0.000126359191821662,-1.15158449541571));
#43397=CARTESIAN_POINT('',(-0.146458539542634,-0.000116607055467748,-1.15871550458429));
#43398=CARTESIAN_POINT('',(-0.14635,-1.79227059055215E-17,-1.487));
#43399=CARTESIAN_POINT('Ctrl Pts',(-0.146420343877387,-0.000126359191821662,
-1.15158449541571));
#43400=CARTESIAN_POINT('Ctrl Pts',(-0.146059012458362,0.0395090623243778,
-1.15374297972548));
#43401=CARTESIAN_POINT('Ctrl Pts',(-0.129398885067076,0.0794119747695151,
-1.15590146403526));
#43402=CARTESIAN_POINT('Ctrl Pts',(-0.100677635328534,0.106550231277221,
-1.15805994834503));
#43403=CARTESIAN_POINT('Ctrl Pts',(-0.0654281877775973,0.139856879076344,
-1.16070904544768));
#43404=CARTESIAN_POINT('Ctrl Pts',(-0.0120116369076935,0.153936723882358,
-1.16335814255033));
#43405=CARTESIAN_POINT('Ctrl Pts',(0.0350755858116793,0.142332853974555,
-1.16600723965298));
#43406=CARTESIAN_POINT('Ctrl Pts',(0.0821628085310534,0.130728984066752,
-1.16865633675563));
#43407=CARTESIAN_POINT('Ctrl Pts',(0.122920703099893,0.0934413994451258,
-1.17130543385828));
#43408=CARTESIAN_POINT('Ctrl Pts',(0.13865800333033,0.047569908061934,-1.17395453096093));
#43409=CARTESIAN_POINT('Ctrl Pts',(0.154395303560766,0.00169841667874217,
-1.17660362806358));
#43410=CARTESIAN_POINT('Ctrl Pts',(0.145112009452802,-0.0527569814660171,
-1.17925272516623));
#43411=CARTESIAN_POINT('Ctrl Pts',(0.115065370383711,-0.0908234472976769,
-1.18190182226889));
#43412=CARTESIAN_POINT('Ctrl Pts',(0.0850187313146192,-0.128889913129339,
-1.18455091937154));
#43413=CARTESIAN_POINT('Ctrl Pts',(0.0342087472843984,-0.1505674466479,
-1.18720001647419));
#43414=CARTESIAN_POINT('Ctrl Pts',(-0.0140635023318603,-0.145914892806514,
-1.18984911357684));
#43415=CARTESIAN_POINT('Ctrl Pts',(-0.062335751948115,-0.141262338965128,
-1.19249821067949));
#43416=CARTESIAN_POINT('Ctrl Pts',(-0.108070267150408,-0.1102796977638,
-1.19514730778214));
#43417=CARTESIAN_POINT('Ctrl Pts',(-0.130293540679301,-0.0671753771692121,
-1.19779640488479));
#43418=CARTESIAN_POINT('Ctrl Pts',(-0.140886303516203,-0.0466296261253513,
-1.19905910172843));
#43419=CARTESIAN_POINT('Ctrl Pts',(-0.146137384722659,-0.0233298668906606,
-1.20032179857207));
#43420=CARTESIAN_POINT('Ctrl Pts',(-0.146110748319233,-1.87736639323394E-5,
-1.20158449541571));
#43421=CARTESIAN_POINT('Ctrl Pts',(-0.146118579951279,-3.98722473775574E-5,
-1.20871550458429));
#43422=CARTESIAN_POINT('Ctrl Pts',(-0.146172129389966,-0.0220367701447063,
-1.20752383467837));
#43423=CARTESIAN_POINT('Ctrl Pts',(-0.141519539811635,-0.0440121565613824,
-1.20633216477246));
#43424=CARTESIAN_POINT('Ctrl Pts',(-0.132045341637239,-0.0636629050438161,
-1.20514049486655));
#43425=CARTESIAN_POINT('Ctrl Pts',(-0.110984080620887,-0.107346764652504,
-1.2024913977639));
#43426=CARTESIAN_POINT('Ctrl Pts',(-0.0660954685102728,-0.139542764323454,
-1.19984230066125));
#43427=CARTESIAN_POINT('Ctrl Pts',(-0.0179650877217393,-0.145486058953644,
-1.1971932035586));
#43428=CARTESIAN_POINT('Ctrl Pts',(0.0301652930667956,-0.151429353583835,
-1.19454410645595));
#43429=CARTESIAN_POINT('Ctrl Pts',(0.0815374425332507,-0.131119943173266,
-1.1918950093533));
#43430=CARTESIAN_POINT('Ctrl Pts',(0.112592476430099,-0.0938715717246213,
-1.18924591225065));
#43431=CARTESIAN_POINT('Ctrl Pts',(0.143647510326947,-0.0566232002759764,
-1.186596815148));
#43432=CARTESIAN_POINT('Ctrl Pts',(0.154385428654186,-0.00243586778925729,
-1.18394771804535));
#43433=CARTESIAN_POINT('Ctrl Pts',(0.139881902226487,0.0438405195705144,
-1.1812986209427));
#43434=CARTESIAN_POINT('Ctrl Pts',(0.125378375798787,0.090116906930286,
-1.17864952384005));
#43435=CARTESIAN_POINT('Ctrl Pts',(0.0856334046161455,0.12848234916311,
-1.1760004267374));
#43436=CARTESIAN_POINT('Ctrl Pts',(0.0388737357630849,0.141342740862539,
-1.17335132963475));
#43437=CARTESIAN_POINT('Ctrl Pts',(-0.00788593308997566,0.154203132561969,
-1.17070223253209));
#43438=CARTESIAN_POINT('Ctrl Pts',(-0.061660299613454,0.141558473728007,
-1.16805313542944));
#43439=CARTESIAN_POINT('Ctrl Pts',(-0.0977888407502427,0.109207510508375,
-1.16540403832679));
#43440=CARTESIAN_POINT('Ctrl Pts',(-0.128195045467967,0.0819805597508731,
-1.16317452707929));
#43441=CARTESIAN_POINT('Ctrl Pts',(-0.146102529657357,0.0407954298906481,
-1.16094501583179));
#43442=CARTESIAN_POINT('Ctrl Pts',(-0.146458539542634,-0.000116607055467748,
-1.15871550458429));
#43443=CARTESIAN_POINT('Origin',(0.,0.,-1.487));
#43444=CARTESIAN_POINT('',(-0.146524574873171,8.77098538252519E-5,-1.10158449541571));
#43445=CARTESIAN_POINT('',(-0.1464923466868,0.000104122940576147,-1.10871550458429));
#43446=CARTESIAN_POINT('',(-0.14635,-1.79227059055215E-17,-1.487));
#43447=CARTESIAN_POINT('Ctrl Pts',(-0.146524574873171,8.77098538252519E-5,
-1.10158449541571));
#43448=CARTESIAN_POINT('Ctrl Pts',(-0.146561083382481,0.00524669631098321,
-1.1018659666736));
#43449=CARTESIAN_POINT('Ctrl Pts',(-0.146312285983159,0.0104021223371573,
-1.10214743793148));
#43450=CARTESIAN_POINT('Ctrl Pts',(-0.145766538895233,0.0155259195888394,
-1.10242890918937));
#43451=CARTESIAN_POINT('Ctrl Pts',(-0.140630181313775,0.063749090067944,
-1.10507800629202));
#43452=CARTESIAN_POINT('Ctrl Pts',(-0.10919050657635,0.109170635495247,
-1.10772710339467));
#43453=CARTESIAN_POINT('Ctrl Pts',(-0.0658655148174998,0.13096057421377,
-1.11037620049732));
#43454=CARTESIAN_POINT('Ctrl Pts',(-0.0225405230586548,0.15275051293229,
-1.11302529759997));
#43455=CARTESIAN_POINT('Ctrl Pts',(0.0326697857216125,0.150908844942036,
-1.11567439470262));
#43456=CARTESIAN_POINT('Ctrl Pts',(0.0744463760666706,0.126280145435118,
-1.11832349180527));
#43457=CARTESIAN_POINT('Ctrl Pts',(0.116222966411732,0.101651445928197,
-1.12097258890792));
#43458=CARTESIAN_POINT('Ctrl Pts',(0.144565838321582,0.0542357149046093,
-1.12362168601057));
#43459=CARTESIAN_POINT('Ctrl Pts',(0.146477162320489,0.0057774526490098,
-1.12627078311322));
#43460=CARTESIAN_POINT('Ctrl Pts',(0.148388486319397,-0.0426808096065883,
-1.12891988021587));
#43461=CARTESIAN_POINT('Ctrl Pts',(0.123868262407364,-0.0921816030941977,
-1.13156897731853));
#43462=CARTESIAN_POINT('Ctrl Pts',(0.0841612822247374,-0.120024233448344,
-1.13421807442118));
#43463=CARTESIAN_POINT('Ctrl Pts',(0.0444543020421122,-0.14786686380249,
-1.13686717152383));
#43464=CARTESIAN_POINT('Ctrl Pts',(-0.010439434411105,-0.154051331023175,
-1.13951626862648));
#43465=CARTESIAN_POINT('Ctrl Pts',(-0.0553460693842255,-0.135741484610605,
-1.14216536572913));
#43466=CARTESIAN_POINT('Ctrl Pts',(-0.10025270435735,-0.117431638198033,
-1.14481446283178));
#43467=CARTESIAN_POINT('Ctrl Pts',(-0.135172237850375,-0.0746274781522026,
-1.14746355993443));
#43468=CARTESIAN_POINT('Ctrl Pts',(-0.144090832480906,-0.0269586727331693,
-1.15011265703708));
#43469=CARTESIAN_POINT('Ctrl Pts',(-0.14574255623835,-0.0181304097992216,
-1.15060326982996));
#43470=CARTESIAN_POINT('Ctrl Pts',(-0.146502472719297,-0.00913529419259381,
-1.15109388262283));
#43471=CARTESIAN_POINT('Ctrl Pts',(-0.146420343877387,-0.000126359191821662,
-1.15158449541571));
#43472=CARTESIAN_POINT('Ctrl Pts',(-0.146458539542634,-0.000116607055467748,
-1.15871550458429));
#43473=CARTESIAN_POINT('Ctrl Pts',(-0.146525539299788,-0.00781610264093099,
-1.15829591872914));
#43474=CARTESIAN_POINT('Ctrl Pts',(-0.14597090336011,-0.0155059258592174,
-1.15787633287399));
#43475=CARTESIAN_POINT('Ctrl Pts',(-0.1447609525327,-0.0230912179959941,
-1.15745674701884));
#43476=CARTESIAN_POINT('Ctrl Pts',(-0.137121807428272,-0.0709817156754305,
-1.15480764991619));
#43477=CARTESIAN_POINT('Ctrl Pts',(-0.10336080146932,-0.114705443429,-1.15215855281354));
#43478=CARTESIAN_POINT('Ctrl Pts',(-0.0589604799596247,-0.134211026110539,
-1.14950945571089));
#43479=CARTESIAN_POINT('Ctrl Pts',(-0.0145601584499285,-0.153716608792078,
-1.14686035860824));
#43480=CARTESIAN_POINT('Ctrl Pts',(0.0404794786105083,-0.149004046401583,
-1.14421126150559));
#43481=CARTESIAN_POINT('Ctrl Pts',(0.0809176645416876,-0.122234484871627,
-1.14156216440294));
#43482=CARTESIAN_POINT('Ctrl Pts',(0.121355850472866,-0.0954649233416712,
-1.13891306730029));
#43483=CARTESIAN_POINT('Ctrl Pts',(0.147192585274786,-0.0466383626722524,
-1.13626397019764));
#43484=CARTESIAN_POINT('Ctrl Pts',(0.14657933524087,0.00185370090836365,
-1.13361487309499));
#43485=CARTESIAN_POINT('Ctrl Pts',(0.145966085206954,0.0503457644889783,
-1.13096577599234));
#43486=CARTESIAN_POINT('Ctrl Pts',(0.118902850337209,0.0985033309807881,
-1.12831667888969));
#43487=CARTESIAN_POINT('Ctrl Pts',(0.077800628113376,0.124241699891289,
-1.12566758178703));
#43488=CARTESIAN_POINT('Ctrl Pts',(0.0366984058895428,0.149980068801791,
-1.12301848468438));
#43489=CARTESIAN_POINT('Ctrl Pts',(-0.0184428036883855,0.153299240130978,
-1.12036938758173));
#43490=CARTESIAN_POINT('Ctrl Pts',(-0.0623356535421235,0.132677066685202,
-1.11772029047908));
#43491=CARTESIAN_POINT('Ctrl Pts',(-0.106228503395864,0.112054893239424,
-1.11507119337643));
#43492=CARTESIAN_POINT('Ctrl Pts',(-0.13887299352542,0.0674913750186834,
-1.11242209627378));
#43493=CARTESIAN_POINT('Ctrl Pts',(-0.145298604451477,0.0194230088082777,
-1.10977299917113));
#43494=CARTESIAN_POINT('Ctrl Pts',(-0.146153618884468,0.0130268626125056,
-1.10942050097552));
#43495=CARTESIAN_POINT('Ctrl Pts',(-0.146544404427699,0.00656865992383821,
-1.1090680027799));
#43496=CARTESIAN_POINT('Ctrl Pts',(-0.1464923466868,0.000104122940576147,
-1.10871550458429));
#43497=CARTESIAN_POINT('Origin',(0.,0.,-1.487));
#43498=CARTESIAN_POINT('',(-0.146149474112214,7.75799253666179E-5,-1.05158449541571));
#43499=CARTESIAN_POINT('',(-0.146131080621407,5.8892630247073E-5,-1.05871550458429));
#43500=CARTESIAN_POINT('',(-0.14635,-1.79227059055215E-17,-1.487));
#43501=CARTESIAN_POINT('Ctrl Pts',(-0.146149474112214,7.75799253666179E-5,
-1.05158449541571));
#43502=CARTESIAN_POINT('Ctrl Pts',(-0.146242719876307,0.0195147651561755,
-1.05263805072436));
#43503=CARTESIAN_POINT('Ctrl Pts',(-0.142640298356387,0.0389187871975207,
-1.05369160603301));
#43504=CARTESIAN_POINT('Ctrl Pts',(-0.135179691770213,0.0567043999481941,
-1.05474516134166));
#43505=CARTESIAN_POINT('Ctrl Pts',(-0.11642047606583,0.101425179977368,
-1.05739425844431));
#43506=CARTESIAN_POINT('Ctrl Pts',(-0.0732683212642689,0.135913750150424,
-1.06004335554696));
#43507=CARTESIAN_POINT('Ctrl Pts',(-0.0255124834227526,0.144353909646322,
-1.06269245264961));
#43508=CARTESIAN_POINT('Ctrl Pts',(0.022243354418761,0.152794069142219,
-1.06534154975226));
#43509=CARTESIAN_POINT('Ctrl Pts',(0.0746028753002338,0.135185817960959,
-1.06799064685491));
#43510=CARTESIAN_POINT('Ctrl Pts',(0.107554393814019,0.0996041686470673,
-1.07063974395756));
#43511=CARTESIAN_POINT('Ctrl Pts',(0.140505912327805,0.0640225193331759,
-1.07328884106021));
#43512=CARTESIAN_POINT('Ctrl Pts',(0.154049428473909,0.0104674718866523,
-1.07593793816287));
#43513=CARTESIAN_POINT('Ctrl Pts',(0.141973986851311,-0.0365010287268484,
-1.07858703526552));
#43514=CARTESIAN_POINT('Ctrl Pts',(0.129898545228714,-0.083469529340349,
-1.08123613236817));
#43515=CARTESIAN_POINT('Ctrl Pts',(0.0922041458374203,-0.123851483120823,
-1.08388522947082));
#43516=CARTESIAN_POINT('Ctrl Pts',(0.0461771588461381,-0.139128027519523,
-1.08653432657347));
#43517=CARTESIAN_POINT('Ctrl Pts',(0.00015017185485576,-0.154404571918223,
-1.08918342367612));
#43518=CARTESIAN_POINT('Ctrl Pts',(-0.0542094027364084,-0.144575706935147,
-1.09183252077877));
#43519=CARTESIAN_POINT('Ctrl Pts',(-0.0919726698192958,-0.114148876678158,
-1.09448161788142));
#43520=CARTESIAN_POINT('Ctrl Pts',(-0.125723522907594,-0.0869549510124533,
-1.09684924372618));
#43521=CARTESIAN_POINT('Ctrl Pts',(-0.146217479609366,-0.0433076611709086,
-1.09921686957095));
#43522=CARTESIAN_POINT('Ctrl Pts',(-0.146524574873171,8.77098538252519E-5,
-1.10158449541571));
#43523=CARTESIAN_POINT('Ctrl Pts',(-0.1464923466868,0.000104122940576147,
-1.10871550458429));
#43524=CARTESIAN_POINT('Ctrl Pts',(-0.146153179700024,-0.0420136772493715,
-1.10641890567725));
#43525=CARTESIAN_POINT('Ctrl Pts',(-0.127016232218379,-0.0844003551295632,
-1.10412230677021));
#43526=CARTESIAN_POINT('Ctrl Pts',(-0.0949958446926328,-0.111645542758528,
-1.10182570786318));
#43527=CARTESIAN_POINT('Ctrl Pts',(-0.0580607422851733,-0.143072513914862,
-1.09917661076053));
#43528=CARTESIAN_POINT('Ctrl Pts',(-0.00398380574769549,-0.154353242027462,
-1.09652751365788));
#43529=CARTESIAN_POINT('Ctrl Pts',(0.0424356855129829,-0.140314469395556,
-1.09387841655523));
#43530=CARTESIAN_POINT('Ctrl Pts',(0.0888551767736612,-0.126275696763649,
-1.09122931945258));
#43531=CARTESIAN_POINT('Ctrl Pts',(0.12761722275754,-0.086917423387236,
-1.08858022234993));
#43532=CARTESIAN_POINT('Ctrl Pts',(0.140945838538626,-0.0402890596236343,
-1.08593112524728));
#43533=CARTESIAN_POINT('Ctrl Pts',(0.154274454319711,0.00633930413996739,
-1.08328202814463));
#43534=CARTESIAN_POINT('Ctrl Pts',(0.142169639898003,0.0602377582907576,
-1.08063293104198));
#43535=CARTESIAN_POINT('Ctrl Pts',(0.110182572803752,0.096688874112066,
-1.07798383393933));
#43536=CARTESIAN_POINT('Ctrl Pts',(0.0781955057095002,0.133139989933375,
-1.07533473683668));
#43537=CARTESIAN_POINT('Ctrl Pts',(0.0263261859427038,0.152143767425202,
-1.07268563973402));
#43538=CARTESIAN_POINT('Ctrl Pts',(-0.0216385036607916,0.144985216094728,
-1.07003654263137));
#43539=CARTESIAN_POINT('Ctrl Pts',(-0.0696031932642857,0.137826664764254,
-1.06738744552872));
#43540=CARTESIAN_POINT('Ctrl Pts',(-0.113663252704479,0.104505784611482,
-1.06473834842607));
#43541=CARTESIAN_POINT('Ctrl Pts',(-0.133613067634466,0.0603032825310584,
-1.06208925132342));
#43542=CARTESIAN_POINT('Ctrl Pts',(-0.142082069267649,0.0415386441810969,
-1.06096466907704));
#43543=CARTESIAN_POINT('Ctrl Pts',(-0.146206085659769,0.0208129935048418,
-1.05984008683066));
#43544=CARTESIAN_POINT('Ctrl Pts',(-0.146131080621407,5.8892630247073E-5,
-1.05871550458429));
#43545=CARTESIAN_POINT('Origin',(0.,0.,-1.487));
#43546=CARTESIAN_POINT('',(-0.14624049998758,-0.000122393304379964,-1.00158449541571));
#43547=CARTESIAN_POINT('',(-0.146276158903947,-0.000129924306316357,-1.00871550458429));
#43548=CARTESIAN_POINT('',(-0.14635,-1.79227059055215E-17,-1.487));
#43549=CARTESIAN_POINT('Ctrl Pts',(-0.14624049998758,-0.000122393304379964,
-1.00158449541571));
#43550=CARTESIAN_POINT('Ctrl Pts',(-0.145975166651522,0.0335064020248649,
-1.00341013477512));
#43551=CARTESIAN_POINT('Ctrl Pts',(-0.134449619835993,0.0672994560490952,
-1.00523577413454));
#43552=CARTESIAN_POINT('Ctrl Pts',(-0.113220905513423,0.0931126446584736,
-1.00706141349395));
#43553=CARTESIAN_POINT('Ctrl Pts',(-0.0824169434302395,0.130568915965678,
-1.0097105105966));
#43554=CARTESIAN_POINT('Ctrl Pts',(-0.0311824668478037,0.151223173297353,
-1.01235960769925));
#43555=CARTESIAN_POINT('Ctrl Pts',(0.0169867757432259,0.145603528427109,
-1.0150087048019));
#43556=CARTESIAN_POINT('Ctrl Pts',(0.0651560183342582,0.139983883556864,
-1.01765780190455));
#43557=CARTESIAN_POINT('Ctrl Pts',(0.110260026933884,0.108090336484698,
-1.0203068990072));
#43558=CARTESIAN_POINT('Ctrl Pts',(0.131614439903856,0.0645490298096645,
-1.02295599610985));
#43559=CARTESIAN_POINT('Ctrl Pts',(0.152968852873826,0.0210077231346337,
-1.0256050932125));
#43560=CARTESIAN_POINT('Ctrl Pts',(0.150573670214146,-0.0341813431432621,
-1.02825419031516));
#43561=CARTESIAN_POINT('Ctrl Pts',(0.125527304812286,-0.0757088752203993,
-1.03090328741781));
#43562=CARTESIAN_POINT('Ctrl Pts',(0.100480939410427,-0.117236407297537,
-1.03355238452046));
#43563=CARTESIAN_POINT('Ctrl Pts',(0.0527833912663882,-0.145102405173915,
-1.03620148162311));
#43564=CARTESIAN_POINT('Ctrl Pts',(0.00430839989247441,-0.146527730245647,
-1.03885057872576));
#43565=CARTESIAN_POINT('Ctrl Pts',(-0.044166591481438,-0.147953055317379,
-1.04149967582841));
#43566=CARTESIAN_POINT('Ctrl Pts',(-0.0934190260852259,-0.122937707584465,
-1.04414877293106));
#43567=CARTESIAN_POINT('Ctrl Pts',(-0.120862105083515,-0.0829535387753645,
-1.04679787003371));
#43568=CARTESIAN_POINT('Ctrl Pts',(-0.137390974279754,-0.0588712156436504,
-1.04839341182771));
#43569=CARTESIAN_POINT('Ctrl Pts',(-0.146008259396191,-0.0293587877137046,
-1.04998895362171));
#43570=CARTESIAN_POINT('Ctrl Pts',(-0.146149474112214,7.75799253666179E-5,
-1.05158449541571));
#43571=CARTESIAN_POINT('Ctrl Pts',(-0.146131080621407,5.8892630247073E-5,
-1.05871550458429));
#43572=CARTESIAN_POINT('Ctrl Pts',(-0.146029401712954,-0.0280759416282176,
-1.05719098972801));
#43573=CARTESIAN_POINT('Ctrl Pts',(-0.138211069888345,-0.0562630595698258,
-1.05566647487174));
#43574=CARTESIAN_POINT('Ctrl Pts',(-0.123039720841311,-0.0796879214310764,
-1.05414196001547));
#43575=CARTESIAN_POINT('Ctrl Pts',(-0.0966769886983866,-0.120392499304715,
-1.05149286291282));
#43576=CARTESIAN_POINT('Ctrl Pts',(-0.0481119539927562,-0.146717531043917,
-1.04884376581017));
#43577=CARTESIAN_POINT('Ctrl Pts',(0.00038382090199534,-0.146590553611849,
-1.04619466870752));
#43578=CARTESIAN_POINT('Ctrl Pts',(0.0488795957967455,-0.14646357617978,
-1.04354557160487));
#43579=CARTESIAN_POINT('Ctrl Pts',(0.0973061108806183,-0.119884589576444,
-1.04089647450222));
#43580=CARTESIAN_POINT('Ctrl Pts',(0.123455327844505,-0.0790425186435681,
-1.03824737739957));
#43581=CARTESIAN_POINT('Ctrl Pts',(0.149604544808393,-0.0382004477106907,
-1.03559828029692));
#43582=CARTESIAN_POINT('Ctrl Pts',(0.153476463652296,0.0169047075517241,
-1.03294918319427));
#43583=CARTESIAN_POINT('Ctrl Pts',(0.133295451298627,0.0610021343053538,
-1.03030008609162));
#43584=CARTESIAN_POINT('Ctrl Pts',(0.113114438944959,0.105099561058982,
-1.02765098898896));
#43585=CARTESIAN_POINT('Ctrl Pts',(0.0688804953937197,0.138189259303824,
-1.02500189188631));
#43586=CARTESIAN_POINT('Ctrl Pts',(0.0208789769470806,0.145096540442412,
-1.02235279478366));
#43587=CARTESIAN_POINT('Ctrl Pts',(-0.0271225414995586,0.152003821581,-1.01970369768101));
#43588=CARTESIAN_POINT('Ctrl Pts',(-0.078891634841599,0.132728685613335,
-1.01705460057836));
#43589=CARTESIAN_POINT('Ctrl Pts',(-0.110687383333389,0.0961105660035381,
-1.01440550347571));
#43590=CARTESIAN_POINT('Ctrl Pts',(-0.133452092296473,0.0698931981089703,
-1.01250883717857));
#43591=CARTESIAN_POINT('Ctrl Pts',(-0.145978287949379,0.0347856633350198,
-1.01061217088143));
#43592=CARTESIAN_POINT('Ctrl Pts',(-0.146276158903947,-0.000129924306316357,
-1.00871550458429));
#43593=CARTESIAN_POINT('Origin',(0.,0.,-1.487));
#43594=CARTESIAN_POINT('',(-0.146588451745324,-1.75972019087617E-5,-0.951584495415713));
#43595=CARTESIAN_POINT('',(-0.146590666816024,6.75222312525112E-6,-0.958715504584286));
#43596=CARTESIAN_POINT('',(-0.14635,-1.79227059055215E-17,-1.487));
#43597=CARTESIAN_POINT('Ctrl Pts',(-0.146588451745324,-1.75972019087617E-5,
-0.951584495415713));
#43598=CARTESIAN_POINT('Ctrl Pts',(-0.146507854065706,0.0475401451251456,
-0.954182218825889));
#43599=CARTESIAN_POINT('Ctrl Pts',(-0.121214084826491,0.0951714550570576,
-0.956779942236065));
#43600=CARTESIAN_POINT('Ctrl Pts',(-0.0817374545005452,0.121687824256767,
-0.959377665646241));
#43601=CARTESIAN_POINT('Ctrl Pts',(-0.0414801173994512,0.148728592548183,
-0.962026762748892));
#43602=CARTESIAN_POINT('Ctrl Pts',(0.0135266004960519,0.153811005652573,
-0.964675859851542));
#43603=CARTESIAN_POINT('Ctrl Pts',(0.05805702898926,0.134604306860943,-0.967324956954193));
#43604=CARTESIAN_POINT('Ctrl Pts',(0.102587457482468,0.115397608069312,
-0.969974054056843));
#43605=CARTESIAN_POINT('Ctrl Pts',(0.13664159657338,0.071901797381661,-0.972623151159494));
#43606=CARTESIAN_POINT('Ctrl Pts',(0.144602472292162,0.0240637288791464,
-0.975272248262145));
#43607=CARTESIAN_POINT('Ctrl Pts',(0.152563348010944,-0.0237743396233668,
-0.977921345364795));
#43608=CARTESIAN_POINT('Ctrl Pts',(0.134430960357596,-0.0759546659407451,
-0.980570442467445));
#43609=CARTESIAN_POINT('Ctrl Pts',(0.0985206869500141,-0.108547741954736,
-0.983219539570096));
#43610=CARTESIAN_POINT('Ctrl Pts',(0.0626104135424317,-0.141140817968727,
-0.985868636672746));
#43611=CARTESIAN_POINT('Ctrl Pts',(0.00892225438061556,-0.154146643679333,
-0.988517733775397));
#43612=CARTESIAN_POINT('Ctrl Pts',(-0.0379228015308373,-0.141600844505346,
-0.991166830878048));
#43613=CARTESIAN_POINT('Ctrl Pts',(-0.0847678574422902,-0.12905504533136,
-0.993815927980698));
#43614=CARTESIAN_POINT('Ctrl Pts',(-0.124769810103378,-0.0909576212727806,
-0.996465025083348));
#43615=CARTESIAN_POINT('Ctrl Pts',(-0.139584062641958,-0.0447797666021233,
-0.999114122185999));
#43616=CARTESIAN_POINT('Ctrl Pts',(-0.144188994243358,-0.0304256261077581,
-0.999937579929236));
#43617=CARTESIAN_POINT('Ctrl Pts',(-0.146360179040833,-0.0152907187279361,
-1.00076103767247));
#43618=CARTESIAN_POINT('Ctrl Pts',(-0.14624049998758,-0.000122393304379964,
-1.00158449541571));
#43619=CARTESIAN_POINT('Ctrl Pts',(-0.146276158903947,-0.000129924306316357,
-1.00871550458429));
#43620=CARTESIAN_POINT('Ctrl Pts',(-0.146394327968595,-0.0139813665834068,
-1.00796307377878));
#43621=CARTESIAN_POINT('Ctrl Pts',(-0.144587995579233,-0.0278026000996961,
-1.00721064297327));
#43622=CARTESIAN_POINT('Ctrl Pts',(-0.140732928203323,-0.0410265846254768,
-1.00645821216776));
#43623=CARTESIAN_POINT('Ctrl Pts',(-0.127160320939926,-0.0875845123927666,
-1.00380911506511));
#43624=CARTESIAN_POINT('Ctrl Pts',(-0.0881927027715921,-0.126739264675417,
-1.00116001796246));
#43625=CARTESIAN_POINT('Ctrl Pts',(-0.0417003324934901,-0.140534764370406,
-0.99851092085981));
#43626=CARTESIAN_POINT('Ctrl Pts',(0.00479203778461458,-0.154330264065396,
-0.99586182375716));
#43627=CARTESIAN_POINT('Ctrl Pts',(0.0588091601724866,-0.142766511172721,
-0.993212726654508));
#43628=CARTESIAN_POINT('Ctrl Pts',(0.0955791855857983,-0.111146556444492,
-0.990563629551857));
#43629=CARTESIAN_POINT('Ctrl Pts',(0.132349210999107,-0.0795266017162653,
-0.987914532449207));
#43630=CARTESIAN_POINT('Ctrl Pts',(0.151872139437857,-0.027850445152484,
-0.985265435346556));
#43631=CARTESIAN_POINT('Ctrl Pts',(0.145194901660481,0.0201836136139252,
-0.982616338243906));
#43632=CARTESIAN_POINT('Ctrl Pts',(0.138517663883105,0.0682176723803358,
-0.979967241141256));
#43633=CARTESIAN_POINT('Ctrl Pts',(0.105640259889603,0.112609633349376,
-0.977318144038606));
#43634=CARTESIAN_POINT('Ctrl Pts',(0.0616400217185707,0.133001674610688,
-0.974669046935955));
#43635=CARTESIAN_POINT('Ctrl Pts',(0.0176397835475385,0.153393715871999,
-0.972019949833305));
#43636=CARTESIAN_POINT('Ctrl Pts',(-0.037483288801022,0.149785837425582,
-0.969370852730653));
#43637=CARTESIAN_POINT('Ctrl Pts',(-0.0784501658468312,0.12383258539382,
-0.966721755628003));
#43638=CARTESIAN_POINT('Ctrl Pts',(-0.11941704289264,0.0978793333620585,
-0.964072658525352));
#43639=CARTESIAN_POINT('Ctrl Pts',(-0.146227724635697,0.0495807077449533,
-0.961423561422702));
#43640=CARTESIAN_POINT('Ctrl Pts',(-0.146587032572823,0.00108609769685721,
-0.958774464320051));
#43641=CARTESIAN_POINT('Ctrl Pts',(-0.146589698223321,0.000726323619918058,
-0.958754811074796));
#43642=CARTESIAN_POINT('Ctrl Pts',(-0.146590908009088,0.000366538756135779,
-0.958735157829541));
#43643=CARTESIAN_POINT('Ctrl Pts',(-0.146590666816024,6.75222312525112E-6,
-0.958715504584286));
#43644=CARTESIAN_POINT('Origin',(0.,0.,-1.487));
#43645=CARTESIAN_POINT('',(-0.146292875288708,0.000132171896627023,-0.901584495415713));
#43646=CARTESIAN_POINT('',(-0.14625608928872,0.000126173321545744,-0.908715504584286));
#43647=CARTESIAN_POINT('',(-0.14635,-1.79227059055215E-17,-1.487));
#43648=CARTESIAN_POINT('Ctrl Pts',(-0.146292875288708,0.000132171896627023,
-0.901584495415713));
#43649=CARTESIAN_POINT('Ctrl Pts',(-0.146409043898152,0.013395829194403,
-0.902305205774001));
#43650=CARTESIAN_POINT('Ctrl Pts',(-0.144754282125947,0.0266310140695942,
-0.90302591613229));
#43651=CARTESIAN_POINT('Ctrl Pts',(-0.141213464455431,0.0393407612670267,
-0.903746626490579));
#43652=CARTESIAN_POINT('Ctrl Pts',(-0.128198569187039,0.086057662292393,
-0.90639572359323));
#43653=CARTESIAN_POINT('Ctrl Pts',(-0.0897019510869531,0.125675591711476,
-0.909044820695881));
#43654=CARTESIAN_POINT('Ctrl Pts',(-0.0433778718351044,0.140026062844143,
-0.911693917798532));
#43655=CARTESIAN_POINT('Ctrl Pts',(0.00294620741674562,0.15437653397681,
-0.914343014901182));
#43656=CARTESIAN_POINT('Ctrl Pts',(0.0570977478203569,0.143459546823063,
-0.916992112003832));
#43657=CARTESIAN_POINT('Ctrl Pts',(0.0942432571928315,0.112281550195303,
-0.919641209106482));
#43658=CARTESIAN_POINT('Ctrl Pts',(0.131388766565305,0.0811035535675439,
-0.922290306209133));
#43659=CARTESIAN_POINT('Ctrl Pts',(0.15152824490664,0.0296645474657715,
-0.924939403311784));
#43660=CARTESIAN_POINT('Ctrl Pts',(0.145425877792544,-0.0184459239086174,
-0.927588500414435));
#43661=CARTESIAN_POINT('Ctrl Pts',(0.139323510678449,-0.0665563952830063,
-0.930237597517086));
#43662=CARTESIAN_POINT('Ctrl Pts',(0.106979298108923,-0.111338331930014,
-0.932886694619735));
#43663=CARTESIAN_POINT('Ctrl Pts',(0.0632260545158511,-0.132255072004567,
-0.935535791722385));
#43664=CARTESIAN_POINT('Ctrl Pts',(0.0194728109227757,-0.153171812079122,
-0.938184888825036));
#43665=CARTESIAN_POINT('Ctrl Pts',(-0.0356894636938444,-0.15022335558122,
-0.940833985927687));
#43666=CARTESIAN_POINT('Ctrl Pts',(-0.0769637619862466,-0.124761842650303,
-0.943483083030338));
#43667=CARTESIAN_POINT('Ctrl Pts',(-0.118238060278645,-0.0993003297193876,
-0.946132180132989));
#43668=CARTESIAN_POINT('Ctrl Pts',(-0.145624382246826,-0.0513257603554585,
-0.948781277235639));
#43669=CARTESIAN_POINT('Ctrl Pts',(-0.146563565077574,-0.00283891393427424,
-0.95143037433829));
#43670=CARTESIAN_POINT('Ctrl Pts',(-0.146581778562416,-0.00189861305417535,
-0.951481748030764));
#43671=CARTESIAN_POINT('Ctrl Pts',(-0.146590045679609,-0.000958119514449902,
-0.951533121723238));
#43672=CARTESIAN_POINT('Ctrl Pts',(-0.146588451745324,-1.75972019087617E-5,
-0.951584495415713));
#43673=CARTESIAN_POINT('Ctrl Pts',(-0.146590666816024,6.75222312525112E-6,
-0.958715504584286));
#43674=CARTESIAN_POINT('Ctrl Pts',(-0.146558397152076,-0.0481297502687534,
-0.956086060726891));
#43675=CARTESIAN_POINT('Ctrl Pts',(-0.120553234067385,-0.0962961323745566,
-0.953456616869495));
#43676=CARTESIAN_POINT('Ctrl Pts',(-0.0802764615941904,-0.122656542592026,
-0.9508271730121));
#43677=CARTESIAN_POINT('Ctrl Pts',(-0.0396986485472351,-0.149213978353728,
-0.948178075909449));
#43678=CARTESIAN_POINT('Ctrl Pts',(0.0153649116778716,-0.153638255398045,
-0.945528978806799));
#43679=CARTESIAN_POINT('Ctrl Pts',(0.059662481416401,-0.133900433300086,
-0.942879881704148));
#43680=CARTESIAN_POINT('Ctrl Pts',(0.10396005115493,-0.114162611202126,
-0.940230784601498));
#43681=CARTESIAN_POINT('Ctrl Pts',(0.137491630406883,-0.0702626899618913,
-0.937581687498847));
#43682=CARTESIAN_POINT('Ctrl Pts',(0.144879887243613,-0.0223328457432308,
-0.934932590396196));
#43683=CARTESIAN_POINT('Ctrl Pts',(0.152268144080344,0.0255969984754297,
-0.932283493293546));
#43684=CARTESIAN_POINT('Ctrl Pts',(0.133513078501854,0.0775567656725155,
-0.929634396190896));
#43685=CARTESIAN_POINT('Ctrl Pts',(0.0972156235741606,0.10971809449585,
-0.926985299088245));
#43686=CARTESIAN_POINT('Ctrl Pts',(0.0609181686464652,0.141879423319186,
-0.924336201985595));
#43687=CARTESIAN_POINT('Ctrl Pts',(0.00707832436956497,0.154242313768768,
-0.921687104882944));
#43688=CARTESIAN_POINT('Ctrl Pts',(-0.0396133585905054,0.141137236574524,
-0.919038007780294));
#43689=CARTESIAN_POINT('Ctrl Pts',(-0.0863050415505731,0.12803215938028,
-0.916388910677643));
#43690=CARTESIAN_POINT('Ctrl Pts',(-0.125848563193812,0.0894591145422132,
-0.913739813574992));
#43691=CARTESIAN_POINT('Ctrl Pts',(-0.140109559690632,0.043107412471758,
-0.911090716472341));
#43692=CARTESIAN_POINT('Ctrl Pts',(-0.144371752568961,0.0292542504920058,
-0.910298979176323));
#43693=CARTESIAN_POINT('Ctrl Pts',(-0.14637561806891,0.0147062704712071,
-0.909507241880305));
#43694=CARTESIAN_POINT('Ctrl Pts',(-0.14625608928872,0.000126173321545744,
-0.908715504584286));
#43695=CARTESIAN_POINT('Origin',(0.,0.,-1.487));
#43696=CARTESIAN_POINT('',(-0.146124565373613,-5.00382259003701E-5,-0.851584495415712));
#43697=CARTESIAN_POINT('',(-0.146140623441789,-6.94491364294977E-5,-0.858715504584287));
#43698=CARTESIAN_POINT('',(-0.14635,-1.79227059055215E-17,-1.487));
#43699=CARTESIAN_POINT('Ctrl Pts',(-0.146124565373613,-5.00382259003701E-5,
-0.851584495415712));
#43700=CARTESIAN_POINT('Ctrl Pts',(-0.146040186260976,0.0275024656860341,
-0.853077289824765));
#43701=CARTESIAN_POINT('Ctrl Pts',(-0.138564166815548,0.0550974423910985,
-0.854570084233817));
#43702=CARTESIAN_POINT('Ctrl Pts',(-0.123983835914978,0.0782109101876611,
-0.85606287864287));
#43703=CARTESIAN_POINT('Ctrl Pts',(-0.0981097355632086,0.119227824640698,
-0.858711975745521));
#43704=CARTESIAN_POINT('Ctrl Pts',(-0.0498629687339267,0.14613171705648,
-0.861361072848171));
#43705=CARTESIAN_POINT('Ctrl Pts',(-0.00136914252851839,0.146584663213145,
-0.864010169950822));
#43706=CARTESIAN_POINT('Ctrl Pts',(0.0471246836768899,0.14703760936981,
-0.866659267053472));
#43707=CARTESIAN_POINT('Ctrl Pts',(0.0958655692584217,0.121039609267357,
-0.869308364156122));
#43708=CARTESIAN_POINT('Ctrl Pts',(0.12250130794355,0.0805131516753259,
-0.871957461258773));
#43709=CARTESIAN_POINT('Ctrl Pts',(0.149137046628681,0.0399866940832921,
-0.874606558361424));
#43710=CARTESIAN_POINT('Ctrl Pts',(0.153667638417403,-0.0150682209983281,
-0.877255655464076));
#43711=CARTESIAN_POINT('Ctrl Pts',(0.134015387736689,-0.0594038205030583,
-0.879904752566726));
#43712=CARTESIAN_POINT('Ctrl Pts',(0.114363137055977,-0.103739420007784,
-0.882553849669376));
#43713=CARTESIAN_POINT('Ctrl Pts',(0.0705280439058388,-0.137355703935627,
-0.885202946772025));
#43714=CARTESIAN_POINT('Ctrl Pts',(0.0226125547719502,-0.144836495425912,
-0.887852043874676));
#43715=CARTESIAN_POINT('Ctrl Pts',(-0.0253029343619412,-0.152317286916197,
-0.890501140977326));
#43716=CARTESIAN_POINT('Ctrl Pts',(-0.0772988194795806,-0.13366258596892,
-0.893150238079978));
#43717=CARTESIAN_POINT('Ctrl Pts',(-0.109530175820052,-0.0974272991794556,
-0.895799335182629));
#43718=CARTESIAN_POINT('Ctrl Pts',(-0.132992705848706,-0.0710501434862831,
-0.897727721926991));
#43719=CARTESIAN_POINT('Ctrl Pts',(-0.145982045835535,-0.0353570653824267,
-0.899656108671351));
#43720=CARTESIAN_POINT('Ctrl Pts',(-0.146292875288708,0.000132171896627023,
-0.901584495415713));
#43721=CARTESIAN_POINT('Ctrl Pts',(-0.14625608928872,0.000126173321545744,
-0.908715504584286));
#43722=CARTESIAN_POINT('Ctrl Pts',(-0.145975683208097,-0.0340777053624083,
-0.906858144777654));
#43723=CARTESIAN_POINT('Ctrl Pts',(-0.134009421342487,-0.0684583369648513,
-0.905000784971022));
#43724=CARTESIAN_POINT('Ctrl Pts',(-0.112099364503826,-0.0944598867485631,
-0.90314342516439));
#43725=CARTESIAN_POINT('Ctrl Pts',(-0.0808497014697991,-0.131545124595585,
-0.90049432806174));
#43726=CARTESIAN_POINT('Ctrl Pts',(-0.0293719040513464,-0.151585240986786,
-0.897845230959089));
#43727=CARTESIAN_POINT('Ctrl Pts',(0.0187266941418953,-0.145389988146464,
-0.895196133856439));
#43728=CARTESIAN_POINT('Ctrl Pts',(0.0668252923351411,-0.139194735306142,
-0.892547036753788));
#43729=CARTESIAN_POINT('Ctrl Pts',(0.111544691303172,-0.106764113234289,
-0.889897939651137));
#43730=CARTESIAN_POINT('Ctrl Pts',(0.132376908513643,-0.0629705631155036,
-0.887248842548487));
#43731=CARTESIAN_POINT('Ctrl Pts',(0.153209125724114,-0.0191770129967208,
-0.884599745445836));
#43732=CARTESIAN_POINT('Ctrl Pts',(0.150154161177028,0.0359794651689932,
-0.881950648343186));
#43733=CARTESIAN_POINT('Ctrl Pts',(0.12461299880809,0.0772045222429877,
-0.879301551240535));
#43734=CARTESIAN_POINT('Ctrl Pts',(0.0990718364391528,0.118429579316982,
-0.876652454137885));
#43735=CARTESIAN_POINT('Ctrl Pts',(0.0510444762483626,0.145723215299258,
-0.874003357035234));
#43736=CARTESIAN_POINT('Ctrl Pts',(0.00255590709058795,0.146568772477828,
-0.871354259932583));
#43737=CARTESIAN_POINT('Ctrl Pts',(-0.0459326620671895,0.147414329656398,
-0.868705162829933));
#43738=CARTESIAN_POINT('Ctrl Pts',(-0.094882440191953,0.121811808031259,
-0.866056065727283));
#43739=CARTESIAN_POINT('Ctrl Pts',(-0.121845424450247,0.0815023328945396,
-0.863406968624632));
#43740=CARTESIAN_POINT('Ctrl Pts',(-0.137762277899623,0.0577067469821571,
-0.86184314727785));
#43741=CARTESIAN_POINT('Ctrl Pts',(-0.146017161763102,0.0287860741111531,
-0.860279325931069));
#43742=CARTESIAN_POINT('Ctrl Pts',(-0.146140623441789,-6.94491364294977E-5,
-0.858715504584287));
#43743=CARTESIAN_POINT('Origin',(0.,0.,-1.487));
#43744=CARTESIAN_POINT('',(-0.146476704385463,-0.000110408673293372,-0.801584495415713));
#43745=CARTESIAN_POINT('',(-0.146510711569069,-9.54240844848774E-5,-0.808715504584287));
#43746=CARTESIAN_POINT('',(-0.14635,-1.79227059055215E-17,-1.487));
#43747=CARTESIAN_POINT('Ctrl Pts',(-0.146476704385463,-0.000110408673293372,
-0.801584495415713));
#43748=CARTESIAN_POINT('Ctrl Pts',(-0.146128043182839,0.0414372295960993,
-0.803849373875529));
#43749=CARTESIAN_POINT('Ctrl Pts',(-0.127578682884935,0.0832570258228007,
-0.806114252335345));
#43750=CARTESIAN_POINT('Ctrl Pts',(-0.0963241152735199,0.11050159662805,
-0.808379130795161));
#43751=CARTESIAN_POINT('Ctrl Pts',(-0.0597674584934802,0.142367992491521,
-0.811028227897811));
#43752=CARTESIAN_POINT('Ctrl Pts',(-0.00582928347880528,0.154294568390982,
-0.813677325000461));
#43753=CARTESIAN_POINT('Ctrl Pts',(0.0407547653621746,0.140811885651917,
-0.816326422103112));
#43754=CARTESIAN_POINT('Ctrl Pts',(0.0873388142031571,0.127329202912852,
-0.818975519205763));
#43755=CARTESIAN_POINT('Ctrl Pts',(0.126568736870447,0.0884372615352578,
-0.821624616308414));
#43756=CARTESIAN_POINT('Ctrl Pts',(0.140453983683775,0.0419716155030087,
-0.824273713411064));
#43757=CARTESIAN_POINT('Ctrl Pts',(0.154339230497103,-0.00449403052923781,
-0.826922810513715));
#43758=CARTESIAN_POINT('Ctrl Pts',(0.142879801456478,-0.0585333812161332,
-0.829571907616364));
#43759=CARTESIAN_POINT('Ctrl Pts',(0.111330905174243,-0.0953643937413661,
-0.832221004719015));
#43760=CARTESIAN_POINT('Ctrl Pts',(0.0797820088920082,-0.132195406266599,
-0.834870101821665));
#43761=CARTESIAN_POINT('Ctrl Pts',(0.0281436453681626,-0.151818080630163,
-0.837519198924316));
#43762=CARTESIAN_POINT('Ctrl Pts',(-0.0199032173703552,-0.145233604853983,
-0.840168296026967));
#43763=CARTESIAN_POINT('Ctrl Pts',(-0.0679500801088757,-0.138649129077803,
-0.842817393129618));
#43764=CARTESIAN_POINT('Ctrl Pts',(-0.112405442062071,-0.105857503161875,
-0.845466490232268));
#43765=CARTESIAN_POINT('Ctrl Pts',(-0.132882406101538,-0.0618967219587649,
-0.848115587334919));
#43766=CARTESIAN_POINT('Ctrl Pts',(-0.141820382988776,-0.0427083087945367,
-0.849271890028517));
#43767=CARTESIAN_POINT('Ctrl Pts',(-0.146189924538032,-0.0213919151082998,
-0.850428192722114));
#43768=CARTESIAN_POINT('Ctrl Pts',(-0.146124565373613,-5.00382259003701E-5,
-0.851584495415712));
#43769=CARTESIAN_POINT('Ctrl Pts',(-0.146140623441789,-6.94491364294977E-5,
-0.858715504584287));
#43770=CARTESIAN_POINT('Ctrl Pts',(-0.146226304563187,-0.0200948822640432,
-0.857630228828418));
#43771=CARTESIAN_POINT('Ctrl Pts',(-0.142395717371333,-0.0400889379277852,
-0.856544953072549));
#43772=CARTESIAN_POINT('Ctrl Pts',(-0.134491951859747,-0.0583168295749055,
-0.85545967731668));
#43773=CARTESIAN_POINT('Ctrl Pts',(-0.11519930461913,-0.102810088259337,
-0.85281058021403));
#43774=CARTESIAN_POINT('Ctrl Pts',(-0.0716378197460715,-0.136780176979901,
-0.85016148311138));
#43775=CARTESIAN_POINT('Ctrl Pts',(-0.0237844690128919,-0.144648666639164,
-0.847512386008729));
#43776=CARTESIAN_POINT('Ctrl Pts',(0.0240688817202849,-0.152517156298425,
-0.844863288906079));
#43777=CARTESIAN_POINT('Ctrl Pts',(0.0762140983135795,-0.134284046896388,
-0.842214191803427));
#43778=CARTESIAN_POINT('Ctrl Pts',(0.108737773706116,-0.0983109062929979,
-0.839565094700777));
#43779=CARTESIAN_POINT('Ctrl Pts',(0.141261449098654,-0.0623377656896056,
-0.836915997598127));
#43780=CARTESIAN_POINT('Ctrl Pts',(0.154163583290429,-0.00862459388485129,
-0.834266900495477));
#43781=CARTESIAN_POINT('Ctrl Pts',(0.141527353856701,0.0381961495053259,
-0.831617803392826));
#43782=CARTESIAN_POINT('Ctrl Pts',(0.128891124422972,0.0850168928955057,
-0.828968706290175));
#43783=CARTESIAN_POINT('Ctrl Pts',(0.0907165313637413,0.124945207871112,
-0.826319609187524));
#43784=CARTESIAN_POINT('Ctrl Pts',(0.0445101580791478,0.139670267252849,
-0.823670512084873));
#43785=CARTESIAN_POINT('Ctrl Pts',(-0.00169621520544052,0.154395326634585,
-0.821021414982223));
#43786=CARTESIAN_POINT('Ctrl Pts',(-0.0559343687153863,0.143917130422458,
-0.818372317879574));
#43787=CARTESIAN_POINT('Ctrl Pts',(-0.0933310901438021,0.113040901178656,
-0.815723220776923));
#43788=CARTESIAN_POINT('Ctrl Pts',(-0.126306553122389,0.0858150397807172,
-0.813387315379378));
#43789=CARTESIAN_POINT('Ctrl Pts',(-0.14618737006938,0.0427291837577693,
-0.811051409981832));
#43790=CARTESIAN_POINT('Ctrl Pts',(-0.146510711569069,-9.54240844848774E-5,
-0.808715504584287));
#43791=CARTESIAN_POINT('Origin',(0.,0.,-1.487));
#43792=CARTESIAN_POINT('',(-0.146474864373602,0.000111087822697115,-0.751584495415713));
#43793=CARTESIAN_POINT('',(-0.146437634202152,0.000122457214444137,-0.758715504584287));
#43794=CARTESIAN_POINT('',(-0.14635,-1.79227059055215E-17,-1.487));
#43795=CARTESIAN_POINT('Ctrl Pts',(-0.146474864373602,0.000111087822697115,
-0.751584495415713));
#43796=CARTESIAN_POINT('Ctrl Pts',(-0.146534826115463,0.0072264447354974,
-0.751972360823642));
#43797=CARTESIAN_POINT('Ctrl Pts',(-0.146061280249954,0.0143337876220666,
-0.752360226231571));
#43798=CARTESIAN_POINT('Ctrl Pts',(-0.145026728944115,0.0213585096002675,
-0.7527480916395));
#43799=CARTESIAN_POINT('Ctrl Pts',(-0.137960806562755,0.0693369326794158,
-0.75539718874215));
#43800=CARTESIAN_POINT('Ctrl Pts',(-0.104725064437985,0.113461250034078,
-0.7580462858448));
#43801=CARTESIAN_POINT('Ctrl Pts',(-0.0605611658003746,0.133496379117466,
-0.76069538294745));
#43802=CARTESIAN_POINT('Ctrl Pts',(-0.0163972671627661,0.153531508200852,
-0.763344480050101));
#43803=CARTESIAN_POINT('Ctrl Pts',(0.0386947879876798,0.149477449012966,
-0.765993577152752));
#43804=CARTESIAN_POINT('Ctrl Pts',(0.0794501944261966,0.12319336283345,
-0.768642674255402));
#43805=CARTESIAN_POINT('Ctrl Pts',(0.120205600864716,0.0969092766539328,
-0.771291771358053));
#43806=CARTESIAN_POINT('Ctrl Pts',(0.146624358591304,0.0483951634827755,
-0.773940868460703));
#43807=CARTESIAN_POINT('Ctrl Pts',(0.146591022530981,-0.000100766542003826,
-0.776589965563353));
#43808=CARTESIAN_POINT('Ctrl Pts',(0.146557686470658,-0.0485966965667832,
-0.779239062666004));
#43809=CARTESIAN_POINT('Ctrl Pts',(0.12007225662343,-0.0970744434451872,
-0.781888159768655));
#43810=CARTESIAN_POINT('Ctrl Pts',(0.079280753401082,-0.12330247434959,
-0.784537256871306));
#43811=CARTESIAN_POINT('Ctrl Pts',(0.0384892501787335,-0.149530505253994,
-0.787186353973957));
#43812=CARTESIAN_POINT('Ctrl Pts',(-0.0166083264187326,-0.153508820184394,
-0.789835451076606));
#43813=CARTESIAN_POINT('Ctrl Pts',(-0.0607446390721617,-0.133412993612194,
-0.792484548179257));
#43814=CARTESIAN_POINT('Ctrl Pts',(-0.104880951725593,-0.113317167039993,
-0.795133645281907));
#43815=CARTESIAN_POINT('Ctrl Pts',(-0.138056000434984,-0.0691471989651908,
-0.797782742384558));
#43816=CARTESIAN_POINT('Ctrl Pts',(-0.145055955516975,-0.021159107014046,
-0.800431839487209));
#43817=CARTESIAN_POINT('Ctrl Pts',(-0.146071212088286,-0.0141990301096382,
-0.800816058130044));
#43818=CARTESIAN_POINT('Ctrl Pts',(-0.146535851989388,-0.00715863553052973,
-0.801200276772879));
#43819=CARTESIAN_POINT('Ctrl Pts',(-0.146476704385463,-0.000110408673293372,
-0.801584495415713));
#43820=CARTESIAN_POINT('Ctrl Pts',(-0.146510711569069,-9.54240844848774E-5,
-0.808715504584287));
#43821=CARTESIAN_POINT('Ctrl Pts',(-0.146554064298903,-0.00583722851058804,
-0.808402312879181));
#43822=CARTESIAN_POINT('Ctrl Pts',(-0.146245838134586,-0.0115743365561838,
-0.808089121174076));
#43823=CARTESIAN_POINT('Ctrl Pts',(-0.145570455937086,-0.0172678917352987,
-0.807775929468971));
#43824=CARTESIAN_POINT('Ctrl Pts',(-0.139857810955068,-0.0654261931299693,
-0.80512683236632));
#43825=CARTESIAN_POINT('Ctrl Pts',(-0.107877231644147,-0.110468533643833,
-0.80247773526367));
#43826=CARTESIAN_POINT('Ctrl Pts',(-0.0642947729383683,-0.131738832162414,
-0.799828638161019));
#43827=CARTESIAN_POINT('Ctrl Pts',(-0.0207123142325892,-0.153009130680996,
-0.797179541058369));
#43828=CARTESIAN_POINT('Ctrl Pts',(0.0344720238680508,-0.150507387204297,
-0.794530443955718));
#43829=CARTESIAN_POINT('Ctrl Pts',(0.0759511158667185,-0.125380882614988,
-0.791881346853068));
#43830=CARTESIAN_POINT('Ctrl Pts',(0.117430207865391,-0.100254378025676,
-0.789232249750417));
#43831=CARTESIAN_POINT('Ctrl Pts',(0.145204053762091,-0.0525031123237477,
-0.786583152647766));
#43832=CARTESIAN_POINT('Ctrl Pts',(0.146535775162883,-0.00402545949255462,
-0.783934055545115));
#43833=CARTESIAN_POINT('Ctrl Pts',(0.147867496563675,0.0444521933386329,
-0.781284958442465));
#43834=CARTESIAN_POINT('Ctrl Pts',(0.122757093468571,0.0936562332990816,
-0.778635861339814));
#43835=CARTESIAN_POINT('Ctrl Pts',(0.0827200092855296,0.121022054975591,
-0.775986764237164));
#43836=CARTESIAN_POINT('Ctrl Pts',(0.0426829251024876,0.148387876652101,
-0.773337667134513));
#43837=CARTESIAN_POINT('Ctrl Pts',(-0.012280840168493,0.153915480044665,
-0.770688570031864));
#43838=CARTESIAN_POINT('Ctrl Pts',(-0.0569653140836648,0.135069947501517,
-0.768039472929213));
#43839=CARTESIAN_POINT('Ctrl Pts',(-0.101649787998837,0.116224414958369,
-0.765390375826563));
#43840=CARTESIAN_POINT('Ctrl Pts',(-0.136054970558202,0.0730057464795088,
-0.762741278723911));
#43841=CARTESIAN_POINT('Ctrl Pts',(-0.144402901877865,0.0252337007980361,
-0.760092181621261));
#43842=CARTESIAN_POINT('Ctrl Pts',(-0.145848980158966,0.0169583431006113,
-0.759633289275603));
#43843=CARTESIAN_POINT('Ctrl Pts',(-0.146513152571914,0.00854635117719349,
-0.759174396929945));
#43844=CARTESIAN_POINT('Ctrl Pts',(-0.146437634202152,0.000122457214444137,
-0.758715504584287));
#43845=CARTESIAN_POINT('Origin',(0.,0.,-1.487));
#43846=CARTESIAN_POINT('',(-0.146123885372185,4.90033357487263E-5,-0.701584495415714));
#43847=CARTESIAN_POINT('',(-0.146113547113789,2.8286021952426E-5,-0.708715504584287));
#43848=CARTESIAN_POINT('',(-0.14635,-1.79227059055215E-17,-1.487));
#43849=CARTESIAN_POINT('Ctrl Pts',(-0.146123885372185,4.90033357487263E-5,
-0.701584495415714));
#43850=CARTESIAN_POINT('Ctrl Pts',(-0.14618807769588,0.0214584373064795,
-0.702744444874405));
#43851=CARTESIAN_POINT('Ctrl Pts',(-0.141789805581938,0.0428427648591023,
-0.703904394333097));
#43852=CARTESIAN_POINT('Ctrl Pts',(-0.132797185057065,0.0620793498797645,
-0.705064343791789));
#43853=CARTESIAN_POINT('Ctrl Pts',(-0.112259803191701,0.106011937857001,
-0.70771344089444));
#43854=CARTESIAN_POINT('Ctrl Pts',(-0.0677594014011252,0.138742415657928,
-0.71036253799709));
#43855=CARTESIAN_POINT('Ctrl Pts',(-0.0197035317469352,0.145260830499044,
-0.713011635099741));
#43856=CARTESIAN_POINT('Ctrl Pts',(0.0283523379072549,0.151779245340161,
-0.715660732202392));
#43857=CARTESIAN_POINT('Ctrl Pts',(0.0799636754250591,0.132085597221468,
-0.718309829305043));
#43858=CARTESIAN_POINT('Ctrl Pts',(0.111461906704158,0.095211246155316,
-0.720958926407693));
#43859=CARTESIAN_POINT('Ctrl Pts',(0.142960137983255,0.0583368950891666,
-0.723608023510343));
#43860=CARTESIAN_POINT('Ctrl Pts',(0.154345263023649,0.0042818410755612,
-0.726257120612994));
#43861=CARTESIAN_POINT('Ctrl Pts',(0.140396148472813,-0.0421646716407751,
-0.728906217715644));
#43862=CARTESIAN_POINT('Ctrl Pts',(0.126447033921977,-0.0886111843571114,
-0.731555314818295));
#43863=CARTESIAN_POINT('Ctrl Pts',(0.0871636797799121,-0.127449155776179,
-0.734204411920946));
#43864=CARTESIAN_POINT('Ctrl Pts',(0.0405611390023424,-0.140867782134196,
-0.736853509023596));
#43865=CARTESIAN_POINT('Ctrl Pts',(-0.00604140177522741,-0.154286408492213,
-0.739502606126247));
#43866=CARTESIAN_POINT('Ctrl Pts',(-0.0599631291883016,-0.14228568978918,
-0.742151703228897));
#43867=CARTESIAN_POINT('Ctrl Pts',(-0.0964759415758636,-0.110369066035847,
-0.744800800331547));
#43868=CARTESIAN_POINT('Ctrl Pts',(-0.127642760093604,-0.0831254889139159,
-0.747062032026269));
#43869=CARTESIAN_POINT('Ctrl Pts',(-0.146125291072154,-0.0413710094243759,
-0.749323263720991));
#43870=CARTESIAN_POINT('Ctrl Pts',(-0.146474864373602,0.000111087822697115,
-0.751584495415713));
#43871=CARTESIAN_POINT('Ctrl Pts',(-0.146437634202152,0.000122457214444137,
-0.758715504584287));
#43872=CARTESIAN_POINT('Ctrl Pts',(-0.146077199572424,-0.0400831657474447,
-0.756525299827295));
#43873=CARTESIAN_POINT('Ctrl Pts',(-0.128866838266126,-0.0805599134748815,
-0.754335095070302));
#43874=CARTESIAN_POINT('Ctrl Pts',(-0.0993963040313856,-0.107746519533642,
-0.75214489031331));
#43875=CARTESIAN_POINT('Ctrl Pts',(-0.0637510947852846,-0.140629271299759,
-0.74949579321066));
#43876=CARTESIAN_POINT('Ctrl Pts',(-0.0101699962131163,-0.154069351947909,
-0.746846696108008));
#43877=CARTESIAN_POINT('Ctrl Pts',(0.036775099867708,-0.141903240824279,
-0.744197599005358));
#43878=CARTESIAN_POINT('Ctrl Pts',(0.0837201959485351,-0.129737129700647,
-0.741548501902707));
#43879=CARTESIAN_POINT('Ctrl Pts',(0.124029289538022,-0.0919648268052367,
-0.738899404800057));
#43880=CARTESIAN_POINT('Ctrl Pts',(0.139216931227097,-0.0459084282721892,
-0.736250307697407));
#43881=CARTESIAN_POINT('Ctrl Pts',(0.154404572916172,0.000147970260858429,
-0.733601210594756));
#43882=CARTESIAN_POINT('Ctrl Pts',(0.144470762704835,0.054488464431539,
-0.730952113492105));
#43883=CARTESIAN_POINT('Ctrl Pts',(0.113971071799202,0.0921929092699334,
-0.728303016389454));
#43884=CARTESIAN_POINT('Ctrl Pts',(0.0834713808935699,0.129897354108328,
-0.725653919286804));
#43885=CARTESIAN_POINT('Ctrl Pts',(0.0324058092936452,0.150965749614433,
-0.723004822184153));
#43886=CARTESIAN_POINT('Ctrl Pts',(-0.0158073530740039,0.145736286886646,
-0.720355725081503));
#43887=CARTESIAN_POINT('Ctrl Pts',(-0.0640205154416559,0.140506824158859,
-0.717706627978853));
#43888=CARTESIAN_POINT('Ctrl Pts',(-0.109381268577035,0.108979503197173,
-0.715057530876202));
#43889=CARTESIAN_POINT('Ctrl Pts',(-0.13108750971441,0.0656125180402923,
-0.712408433773551));
#43890=CARTESIAN_POINT('Ctrl Pts',(-0.141173916312492,0.0454608463410335,
-0.71117745737713));
#43891=CARTESIAN_POINT('Ctrl Pts',(-0.146152713380701,0.0227526906323401,
-0.709946480980708));
#43892=CARTESIAN_POINT('Ctrl Pts',(-0.146113547113789,2.8286021952426E-5,
-0.708715504584287));
#43893=CARTESIAN_POINT('Origin',(0.,0.,-1.487));
#43894=CARTESIAN_POINT('',(-0.146294822930562,-0.000132384695170809,-0.651584495415713));
#43895=CARTESIAN_POINT('',(-0.146333590452415,-0.000134607837447892,-0.658715504584287));
#43896=CARTESIAN_POINT('',(-0.14635,-1.79227059055215E-17,-1.487));
#43897=CARTESIAN_POINT('Ctrl Pts',(-0.146294822930562,-0.000132384695170809,
-0.651584495415713));
#43898=CARTESIAN_POINT('Ctrl Pts',(-0.145982575394241,0.0354227639412815,
-0.653516528925169));
#43899=CARTESIAN_POINT('Ctrl Pts',(-0.132939339037653,0.0711830937012871,
-0.655448562434624));
#43900=CARTESIAN_POINT('Ctrl Pts',(-0.109396129491268,0.0975777889322379,
-0.65738059594408));
#43901=CARTESIAN_POINT('Ctrl Pts',(-0.077114987424532,0.133768729886137,
-0.660029693046731));
#43902=CARTESIAN_POINT('Ctrl Pts',(-0.0250935050063507,0.152351929385001,
-0.662678790149382));
#43903=CARTESIAN_POINT('Ctrl Pts',(0.0228116542714107,0.14480527086393,
-0.665327887252032));
#43904=CARTESIAN_POINT('Ctrl Pts',(0.0707168135491666,0.137258612342861,
-0.667976984354682));
#43905=CARTESIAN_POINT('Ctrl Pts',(0.114505649686507,0.103582095801863,
-0.670626081457333));
#43906=CARTESIAN_POINT('Ctrl Pts',(0.134096929318507,0.0592195203283678,
-0.673275178559983));
#43907=CARTESIAN_POINT('Ctrl Pts',(0.153688208950508,0.01485694485487,-0.675924275662634));
#43908=CARTESIAN_POINT('Ctrl Pts',(0.14908193207717,-0.0401916895511217,
-0.678573372765284));
#43909=CARTESIAN_POINT('Ctrl Pts',(0.122390502886327,-0.0806814900941138,
-0.681222469867935));
#43910=CARTESIAN_POINT('Ctrl Pts',(0.0956990736954827,-0.121171290637108,
-0.683871566970585));
#43911=CARTESIAN_POINT('Ctrl Pts',(0.0469224921871279,-0.147102257317095,
-0.686520664073236));
#43912=CARTESIAN_POINT('Ctrl Pts',(-0.00157066548063597,-0.146582642391664,
-0.689169761175886));
#43913=CARTESIAN_POINT('Ctrl Pts',(-0.0500638231483971,-0.146063027466233,
-0.691818858278537));
#43914=CARTESIAN_POINT('Ctrl Pts',(-0.0982735569755703,-0.119092830935388,
-0.694467955381187));
#43915=CARTESIAN_POINT('Ctrl Pts',(-0.124091242919077,-0.0780403835931955,
-0.697117052483838));
#43916=CARTESIAN_POINT('Ctrl Pts',(-0.138604242898114,-0.0549634057137551,
-0.698606200127797));
#43917=CARTESIAN_POINT('Ctrl Pts',(-0.146041475016394,-0.0274365115865579,
-0.700095347771755));
#43918=CARTESIAN_POINT('Ctrl Pts',(-0.146123885372185,4.90033357487263E-5,
-0.701584495415714));
#43919=CARTESIAN_POINT('Ctrl Pts',(-0.146113547113789,2.8286021952426E-5,
-0.708715504584287));
#43920=CARTESIAN_POINT('Ctrl Pts',(-0.146068426432147,-0.0261508907749407,
-0.707297383878057));
#43921=CARTESIAN_POINT('Ctrl Pts',(-0.139363609380872,-0.0523516326460269,
-0.705879263171828));
#43922=CARTESIAN_POINT('Ctrl Pts',(-0.126136159605208,-0.0746900727457313,
-0.704461142465599));
#43923=CARTESIAN_POINT('Ctrl Pts',(-0.101426839219253,-0.116419029022818,
-0.701812045362949));
#43924=CARTESIAN_POINT('Ctrl Pts',(-0.0539564693079595,-0.144670292224918,
-0.699162948260299));
#43925=CARTESIAN_POINT('Ctrl Pts',(-0.00549460714200485,-0.146488043945805,
-0.696513851157648));
#43926=CARTESIAN_POINT('Ctrl Pts',(0.0429672550239443,-0.148305795666692,
-0.693864754054998));
#43927=CARTESIAN_POINT('Ctrl Pts',(0.0924206094445576,-0.123690035906373,
-0.691215656952347));
#43928=CARTESIAN_POINT('Ctrl Pts',(0.120186516956348,-0.0839293683320362,
-0.688566559849696));
#43929=CARTESIAN_POINT('Ctrl Pts',(0.14795242446814,-0.044168700757697,
-0.685917462747046));
#43930=CARTESIAN_POINT('Ctrl Pts',(0.154030885071109,0.0107368746306564,
-0.683268365644396));
#43931=CARTESIAN_POINT('Ctrl Pts',(0.135634362108998,0.0556080708350706,
-0.680619268541746));
#43932=CARTESIAN_POINT('Ctrl Pts',(0.117237839146887,0.100479267039487,
-0.677970171439095));
#43933=CARTESIAN_POINT('Ctrl Pts',(0.0743663326196887,0.135316084059958,
-0.675321074336444));
#43934=CARTESIAN_POINT('Ctrl Pts',(0.0266803953810701,0.144142617670912,
-0.672671977233793));
#43935=CARTESIAN_POINT('Ctrl Pts',(-0.0210055418575457,0.152969151281866,
-0.670022880131143));
#43936=CARTESIAN_POINT('Ctrl Pts',(-0.0735059098075844,0.135785401483307,
-0.667373783028492));
#43937=CARTESIAN_POINT('Ctrl Pts',(-0.106744431647197,0.100471707654593,
-0.664724685925842));
#43938=CARTESIAN_POINT('Ctrl Pts',(-0.131877058289386,0.0737699822699243,
-0.662721625478657));
#43939=CARTESIAN_POINT('Ctrl Pts',(-0.14599707480881,0.0367027911865322,
-0.660718565031472));
#43940=CARTESIAN_POINT('Ctrl Pts',(-0.146333590452415,-0.000134607837447892,
-0.658715504584287));
#43941=CARTESIAN_POINT('Origin',(0.,0.,-1.487));
#43942=CARTESIAN_POINT('',(-0.146588075907495,1.88366579988541E-5,-0.601584495415713));
#43943=CARTESIAN_POINT('',(-0.146576141592014,4.24426192752484E-5,-0.608715504584288));
#43944=CARTESIAN_POINT('',(-0.14635,-1.79227059055215E-17,-1.487));
#43945=CARTESIAN_POINT('Ctrl Pts',(-0.146588075907495,1.88366579988541E-5,
-0.601584495415713));
#43946=CARTESIAN_POINT('Ctrl Pts',(-0.146589897057712,0.00102612895765277,
-0.601639515873282));
#43947=CARTESIAN_POINT('Ctrl Pts',(-0.146580414477156,0.00203338605800054,
-0.60169453633085));
#43948=CARTESIAN_POINT('Ctrl Pts',(-0.146559523637802,0.00304040649174867,
-0.601749556788419));
#43949=CARTESIAN_POINT('Ctrl Pts',(-0.145553682093586,0.051525915904862,
-0.604398653891069));
#43950=CARTESIAN_POINT('Ctrl Pts',(-0.118101430682682,0.0994627892809135,
-0.60704775099372));
#43951=CARTESIAN_POINT('Ctrl Pts',(-0.0767921669685648,0.124867534342785,
-0.60969684809637));
#43952=CARTESIAN_POINT('Ctrl Pts',(-0.0354829032544475,0.150272279404657,
-0.612345945199021));
#43953=CARTESIAN_POINT('Ctrl Pts',(0.01968337276288,0.153144896152347,-0.614995042301671));
#43954=CARTESIAN_POINT('Ctrl Pts',(0.0634078187231624,0.132168023989712,
-0.617644139404322));
#43955=CARTESIAN_POINT('Ctrl Pts',(0.107132264683442,0.111191151827078,
-0.620293236506972));
#43956=CARTESIAN_POINT('Ctrl Pts',(0.139414880586675,0.066364790754123,
-0.622942333609623));
#43957=CARTESIAN_POINT('Ctrl Pts',(0.145451099772318,0.0182459753260203,
-0.625591430712273));
#43958=CARTESIAN_POINT('Ctrl Pts',(0.151487318957961,-0.0298728401020852,
-0.628240527814924));
#43959=CARTESIAN_POINT('Ctrl Pts',(0.131277141426005,-0.0812841098853423,
-0.630889624917574));
#43960=CARTESIAN_POINT('Ctrl Pts',(0.0940888037217889,-0.112411009490962,
-0.633538722020225));
#43961=CARTESIAN_POINT('Ctrl Pts',(0.0569004660175705,-0.143537909096584,
-0.636187819122875));
#43962=CARTESIAN_POINT('Ctrl Pts',(0.00273396814109076,-0.154380438524573,
-0.638836916225527));
#43963=CARTESIAN_POINT('Ctrl Pts',(-0.0435703383393503,-0.139966294719726,
-0.641486013328177));
#43964=CARTESIAN_POINT('Ctrl Pts',(-0.0898746448197888,-0.125552150914879,
-0.644135110430828));
#43965=CARTESIAN_POINT('Ctrl Pts',(-0.128316759904187,-0.0858813338771997,
-0.646784207533478));
#43966=CARTESIAN_POINT('Ctrl Pts',(-0.14126741658874,-0.0391465841538942,
-0.649433304636128));
#43967=CARTESIAN_POINT('Ctrl Pts',(-0.144772929620772,-0.026496316434326,
-0.650150368229323));
#43968=CARTESIAN_POINT('Ctrl Pts',(-0.146410711883453,-0.0133284822333657,
-0.650867431822518));
#43969=CARTESIAN_POINT('Ctrl Pts',(-0.146294822930562,-0.000132384695170809,
-0.651584495415713));
#43970=CARTESIAN_POINT('Ctrl Pts',(-0.146333590452415,-0.000134607837447892,
-0.658715504584287));
#43971=CARTESIAN_POINT('Ctrl Pts',(-0.146442125090604,-0.0120155823207427,
-0.658069467928821));
#43972=CARTESIAN_POINT('Ctrl Pts',(-0.145116869066501,-0.0238726533188477,
-0.657423431273356));
#43973=CARTESIAN_POINT('Ctrl Pts',(-0.142264859682514,-0.0353503525615738,
-0.65677739461789));
#43974=CARTESIAN_POINT('Ctrl Pts',(-0.130570090149032,-0.0824150810901572,
-0.65412829751524));
#43975=CARTESIAN_POINT('Ctrl Pts',(-0.0932038753528797,-0.123100900288456,
-0.651479200412589));
#43976=CARTESIAN_POINT('Ctrl Pts',(-0.047302082457368,-0.138749597195485,
-0.648830103309939));
#43977=CARTESIAN_POINT('Ctrl Pts',(-0.00140028956185621,-0.154398294102514,
-0.646181006207288));
#43978=CARTESIAN_POINT('Ctrl Pts',(0.0530370814330175,-0.145009868718274,
-0.643531909104638));
#43979=CARTESIAN_POINT('Ctrl Pts',(0.0910454585689465,-0.114889782838525,
-0.640882812001987));
#43980=CARTESIAN_POINT('Ctrl Pts',(0.129053835704878,-0.0847696969587736,
-0.638233714899337));
#43981=CARTESIAN_POINT('Ctrl Pts',(0.150633218981865,-0.0339179505835095,
-0.635584617796686));
#43982=CARTESIAN_POINT('Ctrl Pts',(0.145887464321147,0.0143452250124984,
-0.632935520694035));
#43983=CARTESIAN_POINT('Ctrl Pts',(0.141141709660429,0.0626084006085036,
-0.630286423591385));
#43984=CARTESIAN_POINT('Ctrl Pts',(0.110070817062014,0.108283005425247,
-0.627637326488734));
#43985=CARTESIAN_POINT('Ctrl Pts',(0.0669236659244788,0.130423006658878,
-0.624988229386084));
#43986=CARTESIAN_POINT('Ctrl Pts',(0.0237765147869411,0.152563007892511,
-0.622339132283433));
#43987=CARTESIAN_POINT('Ctrl Pts',(-0.0314468948897182,0.15116840554302,
-0.619690035180783));
#43988=CARTESIAN_POINT('Ctrl Pts',(-0.0734215196755741,0.126878753837049,
-0.617040938078132));
#43989=CARTESIAN_POINT('Ctrl Pts',(-0.115396144461428,0.102589102131079,
-0.614391840975482));
#43990=CARTESIAN_POINT('Ctrl Pts',(-0.144121984356482,0.0554044010686303,
-0.611742743872831));
#43991=CARTESIAN_POINT('Ctrl Pts',(-0.146425583625881,0.00696320231884148,
-0.609093646770181));
#43992=CARTESIAN_POINT('Ctrl Pts',(-0.146535191796691,0.00465830873023068,
-0.608967599374883));
#43993=CARTESIAN_POINT('Ctrl Pts',(-0.146584980624434,0.00235057045985025,
-0.608841551979585));
#43994=CARTESIAN_POINT('Ctrl Pts',(-0.146576141592014,4.24426192752484E-5,
-0.608715504584288));
#43995=CARTESIAN_POINT('Origin',(0.,0.,-1.487));
#43996=CARTESIAN_POINT('',(-0.146238745768959,0.000121916852571603,-0.551584495415713));
#43997=CARTESIAN_POINT('',(-0.146206336570823,0.000110995926028272,-0.558715504584287));
#43998=CARTESIAN_POINT('',(-0.14635,-1.79227059055215E-17,-1.487));
#43999=CARTESIAN_POINT('Ctrl Pts',(-0.146238745768959,0.000121916852571603,
-0.551584495415713));
#44000=CARTESIAN_POINT('Ctrl Pts',(-0.146358386267051,0.0153578781833637,
-0.552411599924045));
#44001=CARTESIAN_POINT('Ctrl Pts',(-0.14416750967714,0.0305602873884727,
-0.553238704432377));
#44002=CARTESIAN_POINT('Ctrl Pts',(-0.139522367613658,0.0449716241207044,
-0.554065808940709));
#44003=CARTESIAN_POINT('Ctrl Pts',(-0.124644643870395,0.0911290685525648,
-0.556714906043359));
#44004=CARTESIAN_POINT('Ctrl Pts',(-0.0845903527646418,0.12917146201847,
-0.559364003146011));
#44005=CARTESIAN_POINT('Ctrl Pts',(-0.0377280931885555,0.141652846864898,
-0.562013100248661));
#44006=CARTESIAN_POINT('Ctrl Pts',(0.00913416638753079,0.154134231711326,
-0.564662197351312));
#44007=CARTESIAN_POINT('Ctrl Pts',(0.06280439443395,0.141054607938275,-0.567311294453962));
#44008=CARTESIAN_POINT('Ctrl Pts',(0.0986698250217679,0.108412193367482,
-0.569960391556612));
#44009=CARTESIAN_POINT('Ctrl Pts',(0.134535255609584,0.0757697787966903,
-0.572609488659263));
#44010=CARTESIAN_POINT('Ctrl Pts',(0.1525958887388,0.0235645734281581,-0.575258585761914));
#44011=CARTESIAN_POINT('Ctrl Pts',(0.144569252880636,-0.0242625052727336,
-0.577907682864564));
#44012=CARTESIAN_POINT('Ctrl Pts',(0.13654261702247,-0.0720895839736307,
-0.580556779967215));
#44013=CARTESIAN_POINT('Ctrl Pts',(0.102428712176916,-0.115538536006886,
-0.583205877069865));
#44014=CARTESIAN_POINT('Ctrl Pts',(0.0578719204427318,-0.134683996320441,
-0.585854974172515));
#44015=CARTESIAN_POINT('Ctrl Pts',(0.0133151287085501,-0.153829456633996,
-0.588504071275166));
#44016=CARTESIAN_POINT('Ctrl Pts',(-0.0416845499142605,-0.148671425227854,
-0.591153168377817));
#44017=CARTESIAN_POINT('Ctrl Pts',(-0.0819046733869025,-0.121575336799696,
-0.593802265480467));
#44018=CARTESIAN_POINT('Ctrl Pts',(-0.12128944446921,-0.0950420209411587,
-0.596396342125549));
#44019=CARTESIAN_POINT('Ctrl Pts',(-0.146502213240191,-0.0474724701172907,
-0.598990418770631));
#44020=CARTESIAN_POINT('Ctrl Pts',(-0.146588075907495,1.88366579988541E-5,
-0.601584495415713));
#44021=CARTESIAN_POINT('Ctrl Pts',(-0.146576141592014,4.24426192752484E-5,
-0.608715504584288));
#44022=CARTESIAN_POINT('Ctrl Pts',(-0.146399213555472,-0.0461586015113418,
-0.606192454876935));
#44023=CARTESIAN_POINT('Ctrl Pts',(-0.122732021093535,-0.0925157336666332,
-0.603669405169581));
#44024=CARTESIAN_POINT('Ctrl Pts',(-0.0851302884352363,-0.119338894404325,
-0.601146355462229));
#44025=CARTESIAN_POINT('Ctrl Pts',(-0.0456500353314474,-0.14750209594057,
-0.598497258359578));
#44026=CARTESIAN_POINT('Ctrl Pts',(0.00919182951988212,-0.154130802575932,
-0.595848161256928));
#44027=CARTESIAN_POINT('Ctrl Pts',(0.0542452362974532,-0.136185138931333,
-0.593199064154278));
#44028=CARTESIAN_POINT('Ctrl Pts',(0.0992986430750269,-0.118239475286734,
-0.590549967051627));
#44029=CARTESIAN_POINT('Ctrl Pts',(0.134563591778846,-0.0757194413621744,
-0.587900869948976));
#44030=CARTESIAN_POINT('Ctrl Pts',(0.143867840189404,-0.0281244072995196,
-0.585251772846325));
#44031=CARTESIAN_POINT('Ctrl Pts',(0.153172088599961,0.0194706267631353,
-0.582602675743675));
#44032=CARTESIAN_POINT('Ctrl Pts',(0.136515636717257,0.0721406609638817,
-0.579953578641024));
#44033=CARTESIAN_POINT('Ctrl Pts',(0.101537009032763,0.105731610804876,
-0.577304481538374));
#44034=CARTESIAN_POINT('Ctrl Pts',(0.0665583813482707,0.139322560645868,
-0.574655384435724));
#44035=CARTESIAN_POINT('Ctrl Pts',(0.0132575778619858,0.153834426127109,
-0.572006287333074));
#44036=CARTESIAN_POINT('Ctrl Pts',(-0.0339220508426392,0.142612174071299,
-0.569357190230423));
#44037=CARTESIAN_POINT('Ctrl Pts',(-0.0811016795472695,0.131389922015488,
-0.566708093127772));
#44038=CARTESIAN_POINT('Ctrl Pts',(-0.122160133470241,0.0944335524226259,
-0.564058996025121));
#44039=CARTESIAN_POINT('Ctrl Pts',(-0.13826831214759,0.0486909805053239,
-0.56140989892247));
#44040=CARTESIAN_POINT('Ctrl Pts',(-0.143729516946169,0.0331827372546198,
-0.560511767476409));
#44041=CARTESIAN_POINT('Ctrl Pts',(-0.146322852208524,0.016664578011516,
-0.559613636030348));
#44042=CARTESIAN_POINT('Ctrl Pts',(-0.146206336570823,0.000110995926028272,
-0.558715504584287));
#44043=CARTESIAN_POINT('Origin',(0.,0.,-1.487));
#44044=CARTESIAN_POINT('',(-0.146150555575012,-7.84903020770444E-5,-0.501584495415714));
#44045=CARTESIAN_POINT('',(-0.146174139180207,-9.5097358159532E-5,-0.508715504584288));
#44046=CARTESIAN_POINT('',(-0.14635,-1.79227059055215E-17,-1.487));
#44047=CARTESIAN_POINT('Ctrl Pts',(-0.146150555575012,-7.84903020770445E-5,
-0.501584495415714));
#44048=CARTESIAN_POINT('Ctrl Pts',(-0.146007294441014,0.0294246106181032,
-0.503183683974809));
#44049=CARTESIAN_POINT('Ctrl Pts',(-0.137347762399225,0.0590050543034279,
-0.504782872533904));
#44050=CARTESIAN_POINT('Ctrl Pts',(-0.120747946537013,0.083119621315723,
-0.506382061093));
#44051=CARTESIAN_POINT('Ctrl Pts',(-0.0932499233332972,0.123066023658725,
-0.50903115819565));
#44052=CARTESIAN_POINT('Ctrl Pts',(-0.0439631442342578,0.14801363562143,
-0.511680255298301));
#44053=CARTESIAN_POINT('Ctrl Pts',(0.00450984179559201,0.146521668593943,
-0.514329352400951));
#44054=CARTESIAN_POINT('Ctrl Pts',(0.0529828278254446,0.145029701566456,
-0.516978449503602));
#44055=CARTESIAN_POINT('Ctrl Pts',(0.100642020786108,0.117098155548773,
-0.519627546606252));
#44056=CARTESIAN_POINT('Ctrl Pts',(0.125631270566046,0.0755362290330639,
-0.522276643708903));
#44057=CARTESIAN_POINT('Ctrl Pts',(0.150620520345982,0.0339743025173592,
-0.524925740811553));
#44058=CARTESIAN_POINT('Ctrl Pts',(0.152939826945199,-0.0212180044963688,
-0.527574837914204));
#44059=CARTESIAN_POINT('Ctrl Pts',(0.131525573671132,-0.0647299120272388,
-0.530223935016854));
#44060=CARTESIAN_POINT('Ctrl Pts',(0.110111320397064,-0.108241819558111,
-0.532873032119505));
#44061=CARTESIAN_POINT('Ctrl Pts',(0.0649635072497097,-0.140073327606124,
-0.535522129222155));
#44062=CARTESIAN_POINT('Ctrl Pts',(0.0167865843058967,-0.145626744205574,
-0.538171226324806));
#44063=CARTESIAN_POINT('Ctrl Pts',(-0.0313903386379162,-0.151180160805023,
-0.540820323427456));
#44064=CARTESIAN_POINT('Ctrl Pts',(-0.0825963713781873,-0.130455485955909,
-0.543469420530107));
#44065=CARTESIAN_POINT('Ctrl Pts',(-0.113348809557938,-0.0929569008324441,
-0.546118517632757));
#44066=CARTESIAN_POINT('Ctrl Pts',(-0.134499681892776,-0.0671661722389087,
-0.547940510227076));
#44067=CARTESIAN_POINT('Ctrl Pts',(-0.145975194912557,-0.0334407205558631,
-0.549762502821394));
#44068=CARTESIAN_POINT('Ctrl Pts',(-0.146238745768959,0.000121916852571603,
-0.551584495415713));
#44069=CARTESIAN_POINT('Ctrl Pts',(-0.146206336570823,0.000110995926028272,
-0.558715504584287));
#44070=CARTESIAN_POINT('Ctrl Pts',(-0.145979181758502,-0.0321612887738781,
-0.556964538927698));
#44071=CARTESIAN_POINT('Ctrl Pts',(-0.135452415366245,-0.0645682087474814,
-0.555213573271108));
#44072=CARTESIAN_POINT('Ctrl Pts',(-0.115796941921911,-0.0898888534149074,
-0.553462607614519));
#44073=CARTESIAN_POINT('Ctrl Pts',(-0.086059489587164,-0.128197341176096,
-0.550813510511868));
#44074=CARTESIAN_POINT('Ctrl Pts',(-0.0354266814859555,-0.150285542456739,
-0.548164413409218));
#44075=CARTESIAN_POINT('Ctrl Pts',(0.0128816545650474,-0.146023973039977,
-0.545515316306567));
#44076=CARTESIAN_POINT('Ctrl Pts',(0.0611899906160503,-0.141762403623215,
-0.542866219203917));
#44077=CARTESIAN_POINT('Ctrl Pts',(0.107173854616843,-0.111151063509043,
-0.540217122101267));
#44078=CARTESIAN_POINT('Ctrl Pts',(0.129745389810405,-0.0682280847573729,
-0.537568024998616));
#44079=CARTESIAN_POINT('Ctrl Pts',(0.152316925003966,-0.0253051060057029,
-0.534918927895966));
#44080=CARTESIAN_POINT('Ctrl Pts',(0.151476131390297,0.0299295113834688,
-0.532269830793315));
#44081=CARTESIAN_POINT('Ctrl Pts',(0.127608590644025,0.0721455842069272,
-0.529620733690664));
#44082=CARTESIAN_POINT('Ctrl Pts',(0.103741049897751,0.114361657030388,
-0.526971636588014));
#44083=CARTESIAN_POINT('Ctrl Pts',(0.0568467620188787,0.143559185288134,
-0.524322539485364));
#44084=CARTESIAN_POINT('Ctrl Pts',(0.00843109735850967,0.146348400483382,
-0.521673442382713));
#44085=CARTESIAN_POINT('Ctrl Pts',(-0.0399845673018567,0.14913761567863,
-0.519024345280063));
#44086=CARTESIAN_POINT('Ctrl Pts',(-0.0899216087437181,0.125518517811378,
-0.516375248177412));
#44087=CARTESIAN_POINT('Ctrl Pts',(-0.118479272546407,0.0863226488448269,
-0.513726151074762));
#44088=CARTESIAN_POINT('Ctrl Pts',(-0.136484445927416,0.0616102486485755,
-0.512055935577937));
#44089=CARTESIAN_POINT('Ctrl Pts',(-0.145991079342716,0.0307059090068275,
-0.510385720081113));
#44090=CARTESIAN_POINT('Ctrl Pts',(-0.146174139180207,-9.5097358159532E-5,
-0.508715504584288));
#44091=CARTESIAN_POINT('Origin',(0.,0.,-1.487));
#44092=CARTESIAN_POINT('',(-0.146526107979514,-8.67851139334103E-5,-0.451584495415714));
#44093=CARTESIAN_POINT('',(-0.146553134476222,-6.73440674254749E-5,-0.458715504584288));
#44094=CARTESIAN_POINT('',(-0.14635,-1.79227059055215E-17,-1.487));
#44095=CARTESIAN_POINT('Ctrl Pts',(-0.146526107979514,-8.67851139334103E-5,
-0.451584495415714));
#44096=CARTESIAN_POINT('Ctrl Pts',(-0.146221087695475,0.0433742309703717,
-0.453955768025573));
#44097=CARTESIAN_POINT('Ctrl Pts',(-0.125655901340594,0.0870858989641212,
-0.456327040635431));
#44098=CARTESIAN_POINT('Ctrl Pts',(-0.0918156512980374,0.114275212611011,
-0.45869831324529));
#44099=CARTESIAN_POINT('Ctrl Pts',(-0.0540105891689472,0.144650097263912,
-0.46134741034794));
#44100=CARTESIAN_POINT('Ctrl Pts',(0.000362446750819749,0.154404219544638,
-0.463996507450591));
#44101=CARTESIAN_POINT('Ctrl Pts',(0.0463683880881343,0.139064411790662,
-0.466645604553242));
#44102=CARTESIAN_POINT('Ctrl Pts',(0.0923743294254462,0.123724604036686,
-0.469294701655892));
#44103=CARTESIAN_POINT('Ctrl Pts',(0.130013176180307,0.0832908662480113,
-0.471943798758543));
#44104=CARTESIAN_POINT('Ctrl Pts',(0.142024034208366,0.0363058087329784,
-0.474592895861193));
#44105=CARTESIAN_POINT('Ctrl Pts',(0.154034892236424,-0.0106792487820545,
-0.477241992963844));
#44106=CARTESIAN_POINT('Ctrl Pts',(0.14041776153768,-0.0642156260234454,
-0.479891090066494));
#44107=CARTESIAN_POINT('Ctrl Pts',(0.107417356597453,-0.0997519400422375,
-0.482540187169145));
#44108=CARTESIAN_POINT('Ctrl Pts',(0.0744169516572266,-0.13528825406103,
-0.485189284271795));
#44109=CARTESIAN_POINT('Ctrl Pts',(0.0220332724755176,-0.152824504857223,
-0.487838381374446));
#44110=CARTESIAN_POINT('Ctrl Pts',(-0.0257109167238908,-0.144318698725396,
-0.490487478477097));
#44111=CARTESIAN_POINT('Ctrl Pts',(-0.0734551059232992,-0.13581289259357,
-0.493136575579747));
#44112=CARTESIAN_POINT('Ctrl Pts',(-0.116559805140407,-0.101265029533724,
-0.495785672682397));
#44113=CARTESIAN_POINT('Ctrl Pts',(-0.135257521094765,-0.0565185016421515,
-0.498434769785048));
#44114=CARTESIAN_POINT('Ctrl Pts',(-0.142667929609352,-0.0387842472500441,
-0.499484678328603));
#44115=CARTESIAN_POINT('Ctrl Pts',(-0.14624461020521,-0.0194480371521357,
-0.500534586872158));
#44116=CARTESIAN_POINT('Ctrl Pts',(-0.146150555575012,-7.84903020770445E-5,
-0.501584495415714));
#44117=CARTESIAN_POINT('Ctrl Pts',(-0.146174139180207,-9.5097358159532E-5,
-0.508715504584288));
#44118=CARTESIAN_POINT('Ctrl Pts',(-0.146281427076904,-0.0181469826561639,
-0.507736622978462));
#44119=CARTESIAN_POINT('Ctrl Pts',(-0.143186151690998,-0.036163373907249,
-0.506757741372636));
#44120=CARTESIAN_POINT('Ctrl Pts',(-0.136722222588937,-0.0528769475012909,
-0.50577885976681));
#44121=CARTESIAN_POINT('Ctrl Pts',(-0.119229222665258,-0.0981080348150043,
-0.503129762664159));
#44122=CARTESIAN_POINT('Ctrl Pts',(-0.0770649366543811,-0.133797569376577,
-0.500480665561509));
#44123=CARTESIAN_POINT('Ctrl Pts',(-0.0295655913606476,-0.143578597061708,
-0.497831568458858));
#44124=CARTESIAN_POINT('Ctrl Pts',(0.0179337539330859,-0.153359624746839,
-0.495182471356208));
#44125=CARTESIAN_POINT('Ctrl Pts',(0.0707681585096733,-0.137232145555528,
-0.492533374253557));
#44126=CARTESIAN_POINT('Ctrl Pts',(0.104708158843949,-0.102592101051803,
-0.489884277150907));
#44127=CARTESIAN_POINT('Ctrl Pts',(0.138648159178227,-0.0679520565480773,
-0.487235180048256));
#44128=CARTESIAN_POINT('Ctrl Pts',(0.153693755270189,-0.0147994467319301,
-0.484586082945605));
#44129=CARTESIAN_POINT('Ctrl Pts',(0.142945149068807,0.0324903383240258,
-0.481936985842954));
#44130=CARTESIAN_POINT('Ctrl Pts',(0.132196542867426,0.0797801233799763,
-0.479287888740303));
#44131=CARTESIAN_POINT('Ctrl Pts',(0.0956537343727117,0.121207083675741,
-0.476638791637653));
#44132=CARTESIAN_POINT('Ctrl Pts',(0.0500749827649339,0.137773124475729,
-0.473989694535003));
#44133=CARTESIAN_POINT('Ctrl Pts',(0.00449623115715341,0.154339165275717,
-0.471340597432353));
#44134=CARTESIAN_POINT('Ctrl Pts',(-0.0501184635636887,0.146044286579924,
-0.468691500329702));
#44135=CARTESIAN_POINT('Ctrl Pts',(-0.0887232101023002,0.116692457836212,
-0.466042403227052));
#44136=CARTESIAN_POINT('Ctrl Pts',(-0.124314338457565,0.089631932954011,
-0.463600103679464));
#44137=CARTESIAN_POINT('Ctrl Pts',(-0.146297537989927,0.0446736938370164,
-0.461157804131876));
#44138=CARTESIAN_POINT('Ctrl Pts',(-0.146553134476222,-6.73440674254749E-5,
-0.458715504584288));
#44139=CARTESIAN_POINT('Origin',(0.,0.,-1.487));
#44140=CARTESIAN_POINT('',(-0.146418337016564,0.000126760208650031,-0.401584495415714));
#44141=CARTESIAN_POINT('',(-0.146378762148194,0.000132588536401338,-0.408715504584289));
#44142=CARTESIAN_POINT('',(-0.14635,-1.79227059055215E-17,-1.487));
#44143=CARTESIAN_POINT('Ctrl Pts',(-0.146418337016564,0.000126760208650031,
-0.401584495415714));
#44144=CARTESIAN_POINT('Ctrl Pts',(-0.146501206702558,0.00920298031833213,
-0.402078754973686));
#44145=CARTESIAN_POINT('Ctrl Pts',(-0.145729860464663,0.0182651549238106,
-0.402573014531657));
#44146=CARTESIAN_POINT('Ctrl Pts',(-0.144053633590977,0.0271567429897478,
-0.403067274089629));
#44147=CARTESIAN_POINT('Ctrl Pts',(-0.135069512428623,0.0748132420974375,
-0.405716371192279));
#44148=CARTESIAN_POINT('Ctrl Pts',(-0.100091164878443,0.117569354400337,
-0.40836546829493));
#44149=CARTESIAN_POINT('Ctrl Pts',(-0.0551594000103929,0.135817445974617,
-0.41101456539758));
#44150=CARTESIAN_POINT('Ctrl Pts',(-0.0102276351423427,0.154065537548897,
-0.413663662500231));
#44151=CARTESIAN_POINT('Ctrl Pts',(0.0446575470435807,0.14780560839456,
-0.416312759602881));
#44152=CARTESIAN_POINT('Ctrl Pts',(0.084326211719807,0.119908415290841,
-0.418961856705532));
#44153=CARTESIAN_POINT('Ctrl Pts',(0.123994876396033,0.0920112221871226,
-0.421610953808183));
#44154=CARTESIAN_POINT('Ctrl Pts',(0.148447023562565,0.0424767651340214,
-0.424260050910833));
#44155=CARTESIAN_POINT('Ctrl Pts',(0.146469081066342,-0.00597882364315429,
-0.426909148013484));
#44156=CARTESIAN_POINT('Ctrl Pts',(0.144491138570118,-0.05443441242033,
-0.429558245116134));
#44157=CARTESIAN_POINT('Ctrl Pts',(0.116083106411145,-0.101811132921574,
-0.432207342218784));
#44158=CARTESIAN_POINT('Ctrl Pts',(0.0742726960689661,-0.126382374796573,
-0.434856439321434));
#44159=CARTESIAN_POINT('Ctrl Pts',(0.0324622857267876,-0.150953616671573,
-0.437505536424085));
#44160=CARTESIAN_POINT('Ctrl Pts',(-0.0227505027985957,-0.152719379920319,
-0.440154633526736));
#44161=CARTESIAN_POINT('Ctrl Pts',(-0.0660454968579486,-0.130869898698522,
-0.442803730629386));
#44162=CARTESIAN_POINT('Ctrl Pts',(-0.109340490917302,-0.109020417476724,
-0.445452827732037));
#44163=CARTESIAN_POINT('Ctrl Pts',(-0.140717690510626,-0.0635556917843813,
-0.448101924834687));
#44164=CARTESIAN_POINT('Ctrl Pts',(-0.145787746138083,-0.0153255054256747,
-0.450751021937338));
#44165=CARTESIAN_POINT('Ctrl Pts',(-0.146319469052927,-0.0102673567270214,
-0.45102884643013));
#44166=CARTESIAN_POINT('Ctrl Pts',(-0.146561844952713,-0.0051787912795902,
-0.451306670922922));
#44167=CARTESIAN_POINT('Ctrl Pts',(-0.146526107979514,-8.67851139334103E-5,
-0.451584495415714));
#44168=CARTESIAN_POINT('Ctrl Pts',(-0.146553134476222,-6.73440674254749E-5,
-0.458715504584288));
#44169=CARTESIAN_POINT('Ctrl Pts',(-0.14657477667343,-0.00385571525995354,
-0.458508707029226));
#44170=CARTESIAN_POINT('Ctrl Pts',(-0.146440641359803,-0.00764252921378538,
-0.458301909474163));
#44171=CARTESIAN_POINT('Ctrl Pts',(-0.146145799317435,-0.0114167888909704,
-0.4580951119191));
#44172=CARTESIAN_POINT('Ctrl Pts',(-0.14236884363758,-0.0597654280828125,
-0.45544601481645));
#44173=CARTESIAN_POINT('Ctrl Pts',(-0.11222013392149,-0.106053927674869,
-0.452796917713799));
#44174=CARTESIAN_POINT('Ctrl Pts',(-0.0695256433820942,-0.129054727302098,
-0.450147820611148));
#44175=CARTESIAN_POINT('Ctrl Pts',(-0.0268311528426982,-0.152055526929327,
-0.447498723508498));
#44176=CARTESIAN_POINT('Ctrl Pts',(0.0284091185200062,-0.15176862659173,
-0.444849626405847));
#44177=CARTESIAN_POINT('Ctrl Pts',(0.0708623946327502,-0.12832559664239,
-0.442200529303197));
#44178=CARTESIAN_POINT('Ctrl Pts',(0.113315670745497,-0.10488256669305,
-0.439551432200546));
#44179=CARTESIAN_POINT('Ctrl Pts',(0.142981951608284,-0.0582834071319632,
-0.436902335097896));
#44180=CARTESIAN_POINT('Ctrl Pts',(0.146256502278931,-0.00989814466686844,
-0.434253237995245));
#44181=CARTESIAN_POINT('Ctrl Pts',(0.149531052949577,0.0384871177982236,
-0.431604140892594));
#44182=CARTESIAN_POINT('Ctrl Pts',(0.126413873428091,0.0886584831673204,
-0.428955043789944));
#44183=CARTESIAN_POINT('Ctrl Pts',(0.0875063296711659,0.117607737815988,
-0.426305946687294));
#44184=CARTESIAN_POINT('Ctrl Pts',(0.0485987859142427,0.146556992464655,
-0.423656849584643));
#44185=CARTESIAN_POINT('Ctrl Pts',(-0.00609912207811904,0.154284136392889,
-0.421007752481993));
#44186=CARTESIAN_POINT('Ctrl Pts',(-0.0515033420254999,0.137245559079037,
-0.418358655379343));
#44187=CARTESIAN_POINT('Ctrl Pts',(-0.0969075619728886,0.120206981765183,
-0.415709558276692));
#44188=CARTESIAN_POINT('Ctrl Pts',(-0.133018093875295,0.0784026832092323,
-0.413060461174041));
#44189=CARTESIAN_POINT('Ctrl Pts',(-0.14327491737069,0.0310038026560445,
-0.410411364071391));
#44190=CARTESIAN_POINT('Ctrl Pts',(-0.145463604151907,0.0208894330992497,
-0.40984607757569));
#44191=CARTESIAN_POINT('Ctrl Pts',(-0.146475052824873,0.0105203165242242,
-0.409280791079989));
#44192=CARTESIAN_POINT('Ctrl Pts',(-0.146378762148194,0.000132588536401338,
-0.408715504584289));
#44193=CARTESIAN_POINT('Origin',(0.,0.,-1.487));
#44194=CARTESIAN_POINT('',(-0.146110499255218,1.76731672666269E-5,-0.351584495415714));
#44195=CARTESIAN_POINT('',(-0.146108623880082,-3.90423146910683E-6,-0.358715504584288));
#44196=CARTESIAN_POINT('',(-0.14635,-1.79227059055215E-17,-1.487));
#44197=CARTESIAN_POINT('Ctrl Pts',(-0.146110499255218,1.76731672666269E-5,
-0.351584495415714));
#44198=CARTESIAN_POINT('Ctrl Pts',(-0.146135644293297,0.0233961899908976,
-0.352850839024449));
#44199=CARTESIAN_POINT('Ctrl Pts',(-0.140852738332724,0.046763976627278,
-0.354117182633184));
#44200=CARTESIAN_POINT('Ctrl Pts',(-0.130201064998778,0.0673544409356841,
-0.355383526241919));
#44201=CARTESIAN_POINT('Ctrl Pts',(-0.107918552754314,0.110428168291655,
-0.358032623344569));
#44202=CARTESIAN_POINT('Ctrl Pts',(-0.062141485911361,0.141347904510693,
-0.36068172044722));
#44203=CARTESIAN_POINT('Ctrl Pts',(-0.0138628855941101,0.145934089381403,
-0.363330817549871));
#44204=CARTESIAN_POINT('Ctrl Pts',(0.0344157147231407,0.150520274252112,
-0.365979914652521));
#44205=CARTESIAN_POINT('Ctrl Pts',(0.085195848514686,0.128772907774494,
-0.368629011755171));
#44206=CARTESIAN_POINT('Ctrl Pts',(0.115190125502062,0.090665169869106,
-0.371278108857822));
#44207=CARTESIAN_POINT('Ctrl Pts',(0.145184402489437,0.0525574319637175,
-0.373927205960472));
#44208=CARTESIAN_POINT('Ctrl Pts',(0.154392822672642,-0.00191067736944712,
-0.376576303063124));
#44209=CARTESIAN_POINT('Ctrl Pts',(0.138592473297352,-0.0477604897995976,
-0.379225400165774));
#44210=CARTESIAN_POINT('Ctrl Pts',(0.122792123922063,-0.0936103022297454,
-0.381874497268425));
#44211=CARTESIAN_POINT('Ctrl Pts',(0.0819830049882875,-0.130841817756885,
-0.384523594371075));
#44212=CARTESIAN_POINT('Ctrl Pts',(0.0348798737952518,-0.142380941296937,
-0.387172691473725));
#44213=CARTESIAN_POINT('Ctrl Pts',(-0.0122232573977919,-0.153920064836991,
-0.389821788576376));
#44214=CARTESIAN_POINT('Ctrl Pts',(-0.0656204008500953,-0.139766796389948,
-0.392470885679027));
#44215=CARTESIAN_POINT('Ctrl Pts',(-0.100824025188982,-0.10641171921018,
-0.395119982781678));
#44216=CARTESIAN_POINT('Ctrl Pts',(-0.129459476625735,-0.0792799192694744,
-0.397274820326357));
#44217=CARTESIAN_POINT('Ctrl Pts',(-0.146057047674118,-0.0394430964399088,
-0.399429657871036));
#44218=CARTESIAN_POINT('Ctrl Pts',(-0.146418337016564,0.000126760208650031,
-0.401584495415714));
#44219=CARTESIAN_POINT('Ctrl Pts',(-0.146378762148194,0.000132588536401338,
-0.408715504584289));
#44220=CARTESIAN_POINT('Ctrl Pts',(-0.146023806678814,-0.0381596012253703,
-0.406631693977338));
#44221=CARTESIAN_POINT('Ctrl Pts',(-0.130616066484444,-0.076704696682295,
-0.404547883370388));
#44222=CARTESIAN_POINT('Ctrl Pts',(-0.103636877624151,-0.10367417867063,
-0.402464072763439));
#44223=CARTESIAN_POINT('Ctrl Pts',(-0.0693388992938295,-0.137959816893702,
-0.399814975660788));
#44224=CARTESIAN_POINT('Ctrl Pts',(-0.0163398275447988,-0.153537630789426,
-0.397165878558138));
#44225=CARTESIAN_POINT('Ctrl Pts',(0.0310553589617483,-0.143263751195025,
-0.394516781455487));
#44226=CARTESIAN_POINT('Ctrl Pts',(0.0784505454682954,-0.132989871600625,
-0.391867684352837));
#44227=CARTESIAN_POINT('Ctrl Pts',(0.120241846732356,-0.0968642985161015,
-0.389218587250186));
#44228=CARTESIAN_POINT('Ctrl Pts',(0.137264083970114,-0.0514539500773136,
-0.386569490147535));
#44229=CARTESIAN_POINT('Ctrl Pts',(0.154286321207871,-0.00604360163852821,
-0.383920393044885));
#44230=CARTESIAN_POINT('Ctrl Pts',(0.146539494419324,0.0486515221545255,
-0.381271295942235));
#44231=CARTESIAN_POINT('Ctrl Pts',(0.117576240538934,0.087548645834438,
-0.378622198839584));
#44232=CARTESIAN_POINT('Ctrl Pts',(0.0886129866585401,0.126445769514355,
-0.375973101736933));
#44233=CARTESIAN_POINT('Ctrl Pts',(0.0384333056862997,0.149544893081133,
-0.373324004634282));
#44234=CARTESIAN_POINT('Ctrl Pts',(-0.00995077527981938,0.146252930904114,
-0.370674907531632));
#44235=CARTESIAN_POINT('Ctrl Pts',(-0.0583348562459329,0.142960968727096,
-0.368025810428981));
#44236=CARTESIAN_POINT('Ctrl Pts',(-0.104923337205923,0.113277920806288,
-0.365376713326331));
#44237=CARTESIAN_POINT('Ctrl Pts',(-0.128351088578806,0.0708162113315071,
-0.362727616223681));
#44238=CARTESIAN_POINT('Ctrl Pts',(-0.140178357811268,0.0493798360671646,
-0.361390245677217));
#44239=CARTESIAN_POINT('Ctrl Pts',(-0.146102800938292,0.0246866455660807,
-0.360052875130753));
#44240=CARTESIAN_POINT('Ctrl Pts',(-0.146108662346803,-3.9036092742423E-6,
-0.358715504584288));
#44241=CARTESIAN_POINT('Origin',(0.,0.,-1.487));
#44242=CARTESIAN_POINT('',(-0.146353309704914,-0.000134325699099658,-0.301584495415715));
#44243=CARTESIAN_POINT('',(-0.146393127902371,-0.000130920977438367,-0.308715504584288));
#44244=CARTESIAN_POINT('',(-0.14635,-1.79227059055215E-17,-1.487));
#44245=CARTESIAN_POINT('Ctrl Pts',(-0.146353309704914,-0.000134325699099658,
-0.301584495415715));
#44246=CARTESIAN_POINT('Ctrl Pts',(-0.146007391017754,0.0373405958603415,
-0.303622923075213));
#44247=CARTESIAN_POINT('Ctrl Pts',(-0.131331784984381,0.0750562040210813,
-0.305661350734711));
#44248=CARTESIAN_POINT('Ctrl Pts',(-0.105395382320675,0.101885972665794,
-0.307699778394209));
#44249=CARTESIAN_POINT('Ctrl Pts',(-0.0716889866929201,0.136753367665229,
-0.31034887549686));
#44250=CARTESIAN_POINT('Ctrl Pts',(-0.0189641785476722,0.153235616985242,
-0.312997972599511));
#44251=CARTESIAN_POINT('Ctrl Pts',(0.0285998386951484,0.143774084129184,
-0.315647069702161));
#44252=CARTESIAN_POINT('Ctrl Pts',(0.0761638559379663,0.134312551273126,
-0.318296166804812));
#44253=CARTESIAN_POINT('Ctrl Pts',(0.118567082278357,0.0989072362409995,
-0.320945263907462));
#44254=CARTESIAN_POINT('Ctrl Pts',(0.136363714660583,0.0537947522026214,
-0.323594361010112));
#44255=CARTESIAN_POINT('Ctrl Pts',(0.154160347042808,0.00868226816424576,
-0.326243458112763));
#44256=CARTESIAN_POINT('Ctrl Pts',(0.147350385466869,-0.0461373848803806,
-0.328892555215414));
#44257=CARTESIAN_POINT('Ctrl Pts',(0.119056827474505,-0.0855243232787071,
-0.331541652318064));
#44258=CARTESIAN_POINT('Ctrl Pts',(0.0907632694821371,-0.124911261677038,
-0.334190749420715));
#44259=CARTESIAN_POINT('Ctrl Pts',(0.0409861150733369,-0.148865485429065,
-0.336839846523365));
#44260=CARTESIAN_POINT('Ctrl Pts',(-0.00744720433101837,-0.146401766342577,
-0.339488943626016));
#44261=CARTESIAN_POINT('Ctrl Pts',(-0.0558805237353709,-0.143938047256089,
-0.342138040728666));
#44262=CARTESIAN_POINT('Ctrl Pts',(-0.102970008135279,-0.11505638533109,
-0.344787137831317));
#44263=CARTESIAN_POINT('Ctrl Pts',(-0.127120771512246,-0.0730016951221395,
-0.347436234933968));
#44264=CARTESIAN_POINT('Ctrl Pts',(-0.139726784484295,-0.0510503405403165,
-0.348818988427883));
#44265=CARTESIAN_POINT('Ctrl Pts',(-0.146083042734713,-0.0255099368727371,
-0.350201741921799));
#44266=CARTESIAN_POINT('Ctrl Pts',(-0.146110499255218,1.76731672666269E-5,
-0.351584495415714));
#44267=CARTESIAN_POINT('Ctrl Pts',(-0.146108662346803,-3.9036092742423E-6,
-0.358715504584288));
#44268=CARTESIAN_POINT('Ctrl Pts',(-0.1461144113632,-0.0242210131648569,
-0.357403778028102));
#44269=CARTESIAN_POINT('Ctrl Pts',(-0.140426379341273,-0.0484355817180389,
-0.356092051471915));
#44270=CARTESIAN_POINT('Ctrl Pts',(-0.129029699738514,-0.0695720799753903,
-0.354780324915729));
#44271=CARTESIAN_POINT('Ctrl Pts',(-0.106013537739563,-0.112258290778747,
-0.352131227813079));
#44272=CARTESIAN_POINT('Ctrl Pts',(-0.0597141919558894,-0.142390341356705,
-0.349482130710428));
#44273=CARTESIAN_POINT('Ctrl Pts',(-0.0113641967350396,-0.14614989825272,
-0.346833033607778));
#44274=CARTESIAN_POINT('Ctrl Pts',(0.0369857984858101,-0.149909455148735,
-0.344183936505127));
#44275=CARTESIAN_POINT('Ctrl Pts',(0.0873864431438355,-0.127296518362809,
-0.341534839402477));
#44276=CARTESIAN_POINT('Ctrl Pts',(0.11672437784428,-0.0886812118973283,
-0.338885742299826));
#44277=CARTESIAN_POINT('Ctrl Pts',(0.146062312544727,-0.0500659054318454,
-0.336236645197175));
#44278=CARTESIAN_POINT('Ctrl Pts',(0.15433753728759,0.00455177071319376,
-0.333587548094525));
#44279=CARTESIAN_POINT('Ctrl Pts',(0.137755095781102,0.0501245579836111,
-0.330938450991874));
#44280=CARTESIAN_POINT('Ctrl Pts',(0.121172654274615,0.0956973452540258,
-0.328289353889224));
#44281=CARTESIAN_POINT('Ctrl Pts',(0.0797325465187796,0.13222524364982,
-0.325640256786573));
#44282=CARTESIAN_POINT('Ctrl Pts',(0.032438896576232,0.14295683165078,-0.322991159683923));
#44283=CARTESIAN_POINT('Ctrl Pts',(-0.0148547533663157,0.153688419651741,
-0.320342062581272));
#44284=CARTESIAN_POINT('Ctrl Pts',(-0.0680019454955752,0.138623697257868,
-0.317692965478621));
#44285=CARTESIAN_POINT('Ctrl Pts',(-0.102629774249709,0.104671233699461,
-0.315043868375971));
#44286=CARTESIAN_POINT('Ctrl Pts',(-0.130203634220464,0.0776351615717817,
-0.312934413778743));
#44287=CARTESIAN_POINT('Ctrl Pts',(-0.146034721274829,0.0386227352408806,
-0.310824959181516));
#44288=CARTESIAN_POINT('Ctrl Pts',(-0.146393127902371,-0.000130920977438367,
-0.308715504584288));
#44289=CARTESIAN_POINT('Origin',(0.,0.,-1.487));
#44290=CARTESIAN_POINT('',(-0.146567193673927,5.3661049326555E-5,-0.251584495415715));
#44291=CARTESIAN_POINT('',(-0.146544032588096,7.46631685089006E-5,-0.258715504584289));
#44292=CARTESIAN_POINT('',(-0.14635,-1.79227059055215E-17,-1.487));
#44293=CARTESIAN_POINT('Ctrl Pts',(-0.146567193673927,5.3661049326555E-5,
-0.251584495415715));
#44294=CARTESIAN_POINT('Ctrl Pts',(-0.146581110999607,0.00300989945102091,
-0.251745910023326));
#44295=CARTESIAN_POINT('Ctrl Pts',(-0.146499434569904,0.00596535408209463,
-0.251907324630937));
#44296=CARTESIAN_POINT('Ctrl Pts',(-0.146319731190637,0.00891483621586715,
-0.252068739238548));
#44297=CARTESIAN_POINT('Ctrl Pts',(-0.143370483235966,0.0573210163660909,
-0.254717836341199));
#44298=CARTESIAN_POINT('Ctrl Pts',(-0.114018095543567,0.104118529904453,
-0.257366933443849));
#44299=CARTESIAN_POINT('Ctrl Pts',(-0.0717233539896174,0.127846386468801,
-0.2600160305465));
#44300=CARTESIAN_POINT('Ctrl Pts',(-0.0294286124356675,0.151574243033149,
-0.26266512764915));
#44301=CARTESIAN_POINT('Ctrl Pts',(0.0258084829798361,0.152232442623483,
-0.265314224751801));
#44302=CARTESIAN_POINT('Ctrl Pts',(0.0686566126486147,0.129519139821814,
-0.267963321854451));
#44303=CARTESIAN_POINT('Ctrl Pts',(0.111504742317396,0.106805837020143,
-0.270612418957102));
#44304=CARTESIAN_POINT('Ctrl Pts',(0.141963906239453,0.060721031826464,
-0.273261516059753));
#44305=CARTESIAN_POINT('Ctrl Pts',(0.14606575922093,0.0123988718749984,
-0.275910613162403));
#44306=CARTESIAN_POINT('Ctrl Pts',(0.150167612202407,-0.0359232880764644,
-0.278559710265054));
#44307=CARTESIAN_POINT('Ctrl Pts',(0.127912154243313,-0.08648280278571,
-0.281208807367704));
#44308=CARTESIAN_POINT('Ctrl Pts',(0.089505572224467,-0.116093456238312,
-0.283857904470355));
#44309=CARTESIAN_POINT('Ctrl Pts',(0.0510989902056226,-0.145704109690911,
-0.286507001573005));
#44310=CARTESIAN_POINT('Ctrl Pts',(-0.00345871587297271,-0.154365901886864,
-0.289156098675655));
#44311=CARTESIAN_POINT('Ctrl Pts',(-0.0491477892818325,-0.138106599586265,
-0.291805195778306));
#44312=CARTESIAN_POINT('Ctrl Pts',(-0.0948368626906975,-0.121847297285664,
-0.294454292880956));
#44313=CARTESIAN_POINT('Ctrl Pts',(-0.131657303429827,-0.0806669004885042,
-0.297103389983607));
#44314=CARTESIAN_POINT('Ctrl Pts',(-0.142723532244259,-0.0334504317504969,
-0.299752487086258));
#44315=CARTESIAN_POINT('Ctrl Pts',(-0.1452745175521,-0.0225660988798718,
-0.30036315652941));
#44316=CARTESIAN_POINT('Ctrl Pts',(-0.146456939564468,-0.011361012785221,
-0.300973825972562));
#44317=CARTESIAN_POINT('Ctrl Pts',(-0.146353309704914,-0.000134325699099658,
-0.301584495415715));
#44318=CARTESIAN_POINT('Ctrl Pts',(-0.146393127902371,-0.000130920977438367,
-0.308715504584288));
#44319=CARTESIAN_POINT('Ctrl Pts',(-0.146484815796816,-0.0100449149375058,
-0.308175862078865));
#44320=CARTESIAN_POINT('Ctrl Pts',(-0.145563904698664,-0.0199419738644643,
-0.307636219573443));
#44321=CARTESIAN_POINT('Ctrl Pts',(-0.143567948415088,-0.0296172570403707,
-0.30709657706802));
#44322=CARTESIAN_POINT('Ctrl Pts',(-0.133769828447326,-0.0771130794988537,
-0.304447479965369));
#44323=CARTESIAN_POINT('Ctrl Pts',(-0.0980651231327929,-0.11926451969288,
-0.301798382862718));
#44324=CARTESIAN_POINT('Ctrl Pts',(-0.0528277437898429,-0.136741241813826,
-0.299149285760068));
#44325=CARTESIAN_POINT('Ctrl Pts',(-0.00759036444689028,-0.154217963934774,
-0.296500188657417));
#44326=CARTESIAN_POINT('Ctrl Pts',(0.0471796889244828,-0.147019967982639,
-0.293851091554767));
#44327=CARTESIAN_POINT('Ctrl Pts',(0.0863652787115969,-0.118448201167358,
-0.291201994452116));
#44328=CARTESIAN_POINT('Ctrl Pts',(0.125550868498709,-0.0898764343520795,
-0.288552897349466));
#44329=CARTESIAN_POINT('Ctrl Pts',(0.149151994701565,-0.0399308966736649,
-0.285903800246815));
#44330=CARTESIAN_POINT('Ctrl Pts',(0.146345357028125,0.00848376113654518,
-0.283254703144165));
#44331=CARTESIAN_POINT('Ctrl Pts',(0.143538719354685,0.0568984189467553,
-0.280605606041514));
#44332=CARTESIAN_POINT('Ctrl Pts',(0.114324317804944,0.103782196888758,
-0.277956508938864));
#44333=CARTESIAN_POINT('Ctrl Pts',(0.0720996588413956,0.127634544390087,
-0.275307411836213));
#44334=CARTESIAN_POINT('Ctrl Pts',(0.0298749998778472,0.151486891891416,
-0.272658314733563));
#44335=CARTESIAN_POINT('Ctrl Pts',(-0.0253599164995117,0.152307808952074,
-0.270009217630912));
#44336=CARTESIAN_POINT('Ctrl Pts',(-0.0682747699736325,0.129720829136157,
-0.267360120528262));
#44337=CARTESIAN_POINT('Ctrl Pts',(-0.111189623447756,0.107133849320239,
-0.264711023425611));
#44338=CARTESIAN_POINT('Ctrl Pts',(-0.141784414018642,0.0611389726277425,
-0.26206192632296));
#44339=CARTESIAN_POINT('Ctrl Pts',(-0.146028599123545,0.0128291061540969,
-0.25941282922031));
#44340=CARTESIAN_POINT('Ctrl Pts',(-0.146400999570288,0.00859022038162686,
-0.259180387674969));
#44341=CARTESIAN_POINT('Ctrl Pts',(-0.146570527904556,0.00433351160816856,
-0.258947946129629));
#44342=CARTESIAN_POINT('Ctrl Pts',(-0.146544032588096,7.46631685089006E-5,
-0.258715504584289));
#44343=CARTESIAN_POINT('Origin',(0.,0.,-1.487));
#44344=CARTESIAN_POINT('',(-0.146191577767457,0.000104459130465896,-0.201584495415715));
#44345=CARTESIAN_POINT('',(-0.146165083001347,8.93600630285772E-5,-0.208715504584289));
#44346=CARTESIAN_POINT('',(-0.14635,-1.79227059055215E-17,-1.487));
#44347=CARTESIAN_POINT('Ctrl Pts',(-0.146191577767457,0.000104459130465896,
-0.201584495415715));
#44348=CARTESIAN_POINT('Ctrl Pts',(-0.14630480808494,0.0173142675966806,
-0.202517994074089));
#44349=CARTESIAN_POINT('Ctrl Pts',(-0.143497504164964,0.0344883226025476,
-0.203451492732464));
#44350=CARTESIAN_POINT('Ctrl Pts',(-0.137606839493189,0.0505301470283315,
-0.204384991390838));
#44351=CARTESIAN_POINT('Ctrl Pts',(-0.12089021909455,0.0960538874497384,
-0.207034088493489));
#44352=CARTESIAN_POINT('Ctrl Pts',(-0.0793426850817587,0.13245955120465,
-0.209683185596139));
#44353=CARTESIAN_POINT('Ctrl Pts',(-0.0320176263359178,0.143051772611944,
-0.21233228269879));
#44354=CARTESIAN_POINT('Ctrl Pts',(0.0153074324099204,0.153643994019238,
-0.21498137980144));
#44355=CARTESIAN_POINT('Ctrl Pts',(0.0684100158888131,0.138422773078912,
-0.217630476904091));
#44356=CARTESIAN_POINT('Ctrl Pts',(0.102937675700814,0.104368448115231,
-0.220279574006741));
#44357=CARTESIAN_POINT('Ctrl Pts',(0.13746533551282,0.0703141231515449,
-0.222928671109392));
#44358=CARTESIAN_POINT('Ctrl Pts',(0.153418071657937,0.0174266941644967,
-0.225577768212043));
#44359=CARTESIAN_POINT('Ctrl Pts',(0.143480078445581,-0.030040058737127,
-0.228226865314694));
#44360=CARTESIAN_POINT('Ctrl Pts',(0.133542085233227,-0.0775068116387426,
-0.230875962417345));
#44361=CARTESIAN_POINT('Ctrl Pts',(0.0977133626634111,-0.119552888454932,
-0.233525059519995));
#44362=CARTESIAN_POINT('Ctrl Pts',(0.0524246954330384,-0.136896272227596,
-0.236174156622645));
#44363=CARTESIAN_POINT('Ctrl Pts',(0.00713602820266312,-0.154239656000261,
-0.238823253725296));
#44364=CARTESIAN_POINT('Ctrl Pts',(-0.0476125836882674,-0.146880346729396,
-0.241472350827946));
#44365=CARTESIAN_POINT('Ctrl Pts',(-0.086713835525261,-0.11819326871292,
-0.244121447930597));
#44366=CARTESIAN_POINT('Ctrl Pts',(-0.123432572498585,-0.0912541498168937,
-0.246609130425636));
#44367=CARTESIAN_POINT('Ctrl Pts',(-0.146352703250883,-0.0455071629176186,
-0.249096812920676));
#44368=CARTESIAN_POINT('Ctrl Pts',(-0.146567193673927,5.3661049326555E-5,
-0.251584495415715));
#44369=CARTESIAN_POINT('Ctrl Pts',(-0.146544032588096,7.46631685089006E-5,
-0.258715504584289));
#44370=CARTESIAN_POINT('Ctrl Pts',(-0.146268565249962,-0.0442038660177313,
-0.256298849026979));
#44371=CARTESIAN_POINT('Ctrl Pts',(-0.124804097187225,-0.0887136805030915,
-0.253882193469668));
#44372=CARTESIAN_POINT('Ctrl Pts',(-0.0898471773911594,-0.115829281451386,
-0.251465537912358));
#44373=CARTESIAN_POINT('Ctrl Pts',(-0.0515279909149432,-0.145552946328443,
-0.248816440809708));
#44374=CARTESIAN_POINT('Ctrl Pts',(0.00300396167641406,-0.154375419827755,
-0.246167343707057));
#44375=CARTESIAN_POINT('Ctrl Pts',(0.0487407340099472,-0.138250781462385,
-0.243518246604407));
#44376=CARTESIAN_POINT('Ctrl Pts',(0.0944775063434778,-0.122126143097015,
-0.240869149501756));
#44377=CARTESIAN_POINT('Ctrl Pts',(0.131419098419185,-0.0810543928669649,
-0.238220052399106));
#44378=CARTESIAN_POINT('Ctrl Pts',(0.142624371884594,-0.0338707288247468,
-0.235570955296455));
#44379=CARTESIAN_POINT('Ctrl Pts',(0.153829645350003,0.0133129352174713,
-0.232921858193804));
#44380=CARTESIAN_POINT('Ctrl Pts',(0.139298600205113,0.0666085130718572,
-0.230272761091154));
#44381=CARTESIAN_POINT('Ctrl Pts',(0.105695065275732,0.10157505059336,-0.227623663988504));
#44382=CARTESIAN_POINT('Ctrl Pts',(0.0720915303463524,0.136541588114861,
-0.224974566885853));
#44383=CARTESIAN_POINT('Ctrl Pts',(0.0194155056324831,0.153179085303482,
-0.222325469783203));
#44384=CARTESIAN_POINT('Ctrl Pts',(-0.028176177159521,0.143857710143993,
-0.219676372680552));
#44385=CARTESIAN_POINT('Ctrl Pts',(-0.0757678599515305,0.134536334984504,
-0.217027275577902));
#44386=CARTESIAN_POINT('Ctrl Pts',(-0.118275200821673,0.0992560874768987,
-0.214378178475251));
#44387=CARTESIAN_POINT('Ctrl Pts',(-0.136204650575506,0.0541962257673195,
-0.2117290813726));
#44388=CARTESIAN_POINT('Ctrl Pts',(-0.143003416533825,0.0371097307502518,
-0.210724555776496));
#44389=CARTESIAN_POINT('Ctrl Pts',(-0.146268147255594,0.0186170328565388,
-0.209720030180393));
#44390=CARTESIAN_POINT('Ctrl Pts',(-0.146165083001347,8.93600630285772E-5,
-0.208715504584289));
#44391=CARTESIAN_POINT('Origin',(0.,0.,-1.487));
#44392=CARTESIAN_POINT('',(-0.146187581536877,-0.000102482699927964,-0.151584495415715));
#44393=CARTESIAN_POINT('',(-0.146217633328538,-0.000115290056034918,-0.158715504584289));
#44394=CARTESIAN_POINT('',(-0.14635,-1.79227059055215E-17,-1.487));
#44395=CARTESIAN_POINT('Ctrl Pts',(-0.146187581536877,-0.000102482699927964,
-0.151584495415715));
#44396=CARTESIAN_POINT('Ctrl Pts',(-0.145984962940154,0.0313434842482817,
-0.153290078124853));
#44397=CARTESIAN_POINT('Ctrl Pts',(-0.136039089214935,0.0629063216346523,
-0.154995660833991));
#44398=CARTESIAN_POINT('Ctrl Pts',(-0.117317824998014,0.0878946281013525,
-0.156701243543129));
#44399=CARTESIAN_POINT('Ctrl Pts',(-0.0882401106606897,0.126706261161662,
-0.15935034064578));
#44400=CARTESIAN_POINT('Ctrl Pts',(-0.0379926020706468,0.149657464192199,
-0.16199943774843));
#44401=CARTESIAN_POINT('Ctrl Pts',(0.0103815712888817,0.146222984256681,
-0.164648534851081));
#44402=CARTESIAN_POINT('Ctrl Pts',(0.0587557446484075,0.142788504321163,
-0.167297631953731));
#44403=CARTESIAN_POINT('Ctrl Pts',(0.105256582777419,0.112968341419593,
-0.169946729056382));
#44404=CARTESIAN_POINT('Ctrl Pts',(0.128559146939399,0.0704378009967336,
-0.172595826159032));
#44405=CARTESIAN_POINT('Ctrl Pts',(0.151861711101382,0.0279072605738691,
-0.175244923261682));
#44406=CARTESIAN_POINT('Ctrl Pts',(0.151966001296327,-0.0273336573702886,
-0.177894020364333));
#44407=CARTESIAN_POINT('Ctrl Pts',(0.128824191611502,-0.0699518809554031,
-0.180543117466984));
#44408=CARTESIAN_POINT('Ctrl Pts',(0.105682381926679,-0.112570104540515,
-0.183192214569634));
#44409=CARTESIAN_POINT('Ctrl Pts',(0.0592944723620888,-0.142565633766586,
-0.185841311672285));
#44410=CARTESIAN_POINT('Ctrl Pts',(0.0109336115367446,-0.146182742475658,
-0.188490408774935));
#44411=CARTESIAN_POINT('Ctrl Pts',(-0.0374272492885997,-0.14979985118473,
-0.191139505877586));
#44412=CARTESIAN_POINT('Ctrl Pts',(-0.0877610613746981,-0.127038539376803,
-0.193788602980236));
#44413=CARTESIAN_POINT('Ctrl Pts',(-0.116985114025505,-0.0883369749288895,
-0.196437700082887));
#44414=CARTESIAN_POINT('Ctrl Pts',(-0.135911086657086,-0.0632732112444792,
-0.198153298527163));
#44415=CARTESIAN_POINT('Ctrl Pts',(-0.145983481317853,-0.0315239962144383,
-0.199868896971439));
#44416=CARTESIAN_POINT('Ctrl Pts',(-0.146191577767457,0.000104459130465896,
-0.201584495415715));
#44417=CARTESIAN_POINT('Ctrl Pts',(-0.146165083001347,8.93600630285772E-5,
-0.208715504584289));
#44418=CARTESIAN_POINT('Ctrl Pts',(-0.145996350082509,-0.0302434486548492,
-0.207070933077742));
#44419=CARTESIAN_POINT('Ctrl Pts',(-0.136800914172156,-0.0606700006186409,
-0.205426361571195));
#44420=CARTESIAN_POINT('Ctrl Pts',(-0.119308252051597,-0.0851732277138702,
-0.203781790064649));
#44421=CARTESIAN_POINT('Ctrl Pts',(-0.0911308451363325,-0.124643343573932,
-0.201132692961998));
#44422=CARTESIAN_POINT('Ctrl Pts',(-0.0414244726682828,-0.148744099382509,
-0.198483595859348));
#44423=CARTESIAN_POINT('Ctrl Pts',(0.00701589397457254,-0.146423068406191,
-0.195834498756698));
#44424=CARTESIAN_POINT('Ctrl Pts',(0.0554562606174306,-0.144102037429874,
-0.193185401654047));
#44425=CARTESIAN_POINT('Ctrl Pts',(0.102630621435091,-0.115359219668657,
-0.190536304551397));
#44426=CARTESIAN_POINT('Ctrl Pts',(0.126905166768256,-0.0733758568444998,
-0.187887207448746));
#44427=CARTESIAN_POINT('Ctrl Pts',(0.151179712101423,-0.0313924940203378,
-0.185238110346095));
#44428=CARTESIAN_POINT('Ctrl Pts',(0.152554441950085,0.0238314138667743,
-0.182589013243444));
#44429=CARTESIAN_POINT('Ctrl Pts',(0.130398915371771,0.0669705950335863,
-0.179939916140793));
#44430=CARTESIAN_POINT('Ctrl Pts',(0.10824338879346,0.110109776200391,-0.177290819038143));
#44431=CARTESIAN_POINT('Ctrl Pts',(0.0625576057881857,0.141164230646906,
-0.174641721935492));
#44432=CARTESIAN_POINT('Ctrl Pts',(0.0142927255765135,0.145892617156203,
-0.171992624832842));
#44433=CARTESIAN_POINT('Ctrl Pts',(-0.0339721546351587,0.150621003665501,
-0.169343527730192));
#44434=CARTESIAN_POINT('Ctrl Pts',(-0.0848161320532254,0.129023322237581,
-0.166694430627541));
#44435=CARTESIAN_POINT('Ctrl Pts',(-0.114922538535846,0.0910041087871558,
-0.164045333524891));
#44436=CARTESIAN_POINT('Ctrl Pts',(-0.135113316796115,0.0655066284136506,
-0.162268723878024));
#44437=CARTESIAN_POINT('Ctrl Pts',(-0.14597700518956,0.0326232731273325,
-0.160492114231156));
#44438=CARTESIAN_POINT('Ctrl Pts',(-0.146217633328538,-0.000115290056034918,
-0.158715504584289));
#44439=CARTESIAN_POINT('Origin',(0.,0.,-1.487));
#44440=CARTESIAN_POINT('',(-0.146564414435351,-5.66789191273343E-5,-0.101584495415716));
#44441=CARTESIAN_POINT('',(-0.146581435366625,-3.40469869341234E-5,-0.10871550458429));
#44442=CARTESIAN_POINT('',(-0.14635,-1.79227059055215E-17,-1.487));
#44443=CARTESIAN_POINT('Ctrl Pts',(-0.146564414435351,-5.66789191273343E-5,
-0.101584495415716));
#44444=CARTESIAN_POINT('Ctrl Pts',(-0.146340217108257,0.0453231005231363,
-0.104062162175617));
#44445=CARTESIAN_POINT('Ctrl Pts',(-0.12362882200582,0.0908964496879157,
-0.106539828935518));
#44446=CARTESIAN_POINT('Ctrl Pts',(-0.0871594563241677,0.117864973908624,
-0.109017495695419));
#44447=CARTESIAN_POINT('Ctrl Pts',(-0.0481667666992645,0.14669945662925,
-0.11166659279807));
#44448=CARTESIAN_POINT('Ctrl Pts',(0.00655359128472432,0.154265503361126,
-0.11431568990072));
#44449=CARTESIAN_POINT('Ctrl Pts',(0.0519074034152914,0.137093261865771,
-0.116964787003371));
#44450=CARTESIAN_POINT('Ctrl Pts',(0.0972612155458585,0.119921020370417,
-0.119613884106021));
#44451=CARTESIAN_POINT('Ctrl Pts',(0.133248481823007,0.0780104906478297,
-0.122262981208672));
#44452=CARTESIAN_POINT('Ctrl Pts',(0.143365640264857,0.0305815918194669,
-0.124912078311322));
#44453=CARTESIAN_POINT('Ctrl Pts',(0.153482798706707,-0.016847307008896,
-0.127561175413973));
#44454=CARTESIAN_POINT('Ctrl Pts',(0.137729849313264,-0.0697945749430308,
-0.130210272516623));
#44455=CARTESIAN_POINT('Ctrl Pts',(0.10333101412408,-0.103979023385252,
-0.132859369619274));
#44456=CARTESIAN_POINT('Ctrl Pts',(0.0689321789348948,-0.138163471827475,
-0.135508466721924));
#44457=CARTESIAN_POINT('Ctrl Pts',(0.015887457949965,-0.153585100777775,
-0.138157563824575));
#44458=CARTESIAN_POINT('Ctrl Pts',(-0.0314772552874305,-0.143171648821433,
-0.140806660927225));
#44459=CARTESIAN_POINT('Ctrl Pts',(-0.078841968524826,-0.132758196865091,
-0.143455758029876));
#44460=CARTESIAN_POINT('Ctrl Pts',(-0.12052667401469,-0.0965096640021071,
-0.146104855132527));
#44461=CARTESIAN_POINT('Ctrl Pts',(-0.137415066717318,-0.0510493660255724,
-0.148753952235178));
#44462=CARTESIAN_POINT('Ctrl Pts',(-0.143430112969218,-0.0348580208946959,
-0.14969746662869));
#44463=CARTESIAN_POINT('Ctrl Pts',(-0.146299668486034,-0.0174981342122152,
-0.150640981022202));
#44464=CARTESIAN_POINT('Ctrl Pts',(-0.146187581536877,-0.000102482699927964,
-0.151584495415715));
#44465=CARTESIAN_POINT('Ctrl Pts',(-0.146217633328538,-0.000115290056034918,
-0.158715504584289));
#44466=CARTESIAN_POINT('Ctrl Pts',(-0.146335805056997,-0.0161930963137119,
-0.157843017128505));
#44467=CARTESIAN_POINT('Ctrl Pts',(-0.143891948052167,-0.0322359821699961,
-0.156970529672722));
#44468=CARTESIAN_POINT('Ctrl Pts',(-0.138732566475733,-0.0473520089990637,
-0.156098042216939));
#44469=CARTESIAN_POINT('Ctrl Pts',(-0.123067352385828,-0.0932481678619148,
-0.153448945114288));
#44470=CARTESIAN_POINT('Ctrl Pts',(-0.082368088658853,-0.130599740114677,
-0.150799848011638));
#44471=CARTESIAN_POINT('Ctrl Pts',(-0.0352991550669112,-0.142277571968052,
-0.148150750908987));
#44472=CARTESIAN_POINT('Ctrl Pts',(0.011769778525028,-0.153955403821426,
-0.145501653806337));
#44473=CARTESIAN_POINT('Ctrl Pts',(0.0652083819819311,-0.13995949527541,
-0.142852556703686));
#44474=CARTESIAN_POINT('Ctrl Pts',(0.100510113056305,-0.106708268520858,
-0.140203459601036));
#44475=CARTESIAN_POINT('Ctrl Pts',(0.135811844130678,-0.0734570417663067,
-0.137554362498385));
#44476=CARTESIAN_POINT('Ctrl Pts',(0.152976702822525,-0.0209504968032168,
-0.134905265395735));
#44477=CARTESIAN_POINT('Ctrl Pts',(0.144133008567398,0.0267322625321848,
-0.132256168293084));
#44478=CARTESIAN_POINT('Ctrl Pts',(0.135289314312271,0.0744150218675864,
-0.129607071190434));
#44479=CARTESIAN_POINT('Ctrl Pts',(0.10043706711017,0.117273995575304,-0.126957974087783));
#44480=CARTESIAN_POINT('Ctrl Pts',(0.055559255904687,0.135654367406582,
-0.124308876985133));
#44481=CARTESIAN_POINT('Ctrl Pts',(0.0106814446992037,0.15403473923786,
-0.121659779882482));
#44482=CARTESIAN_POINT('Ctrl Pts',(-0.0442219305096567,0.147936509192702,
-0.119010682779832));
#44483=CARTESIAN_POINT('Ctrl Pts',(-0.0839726079418993,0.120156300644783,
-0.116361585677182));
#44484=CARTESIAN_POINT('Ctrl Pts',(-0.122216695312928,0.0934289895265518,
-0.113812891979551));
#44485=CARTESIAN_POINT('Ctrl Pts',(-0.146434922801896,0.0466320910035745,
-0.11126419828192));
#44486=CARTESIAN_POINT('Ctrl Pts',(-0.146581435366625,-3.40469869341234E-5,
-0.10871550458429));
#44487=CARTESIAN_POINT('Origin',(0.,0.,-1.487));
#44488=CARTESIAN_POINT('',(-0.146359156828661,0.000134286233873571,-0.051584495415716));
#44489=CARTESIAN_POINT('',(-0.146319403921505,0.000134192518820611,-0.0587155045842896));
#44490=CARTESIAN_POINT('',(-0.14635,-1.79227059055215E-17,-1.487));
#44491=CARTESIAN_POINT('Ctrl Pts',(-0.146359156828661,0.000134286233873571,
-0.051584495415716));
#44492=CARTESIAN_POINT('Ctrl Pts',(-0.146462627304662,0.0111769826627363,
-0.05218514912373));
#44493=CARTESIAN_POINT('Ctrl Pts',(-0.145320316174143,0.0221985827027607,
-0.0527858028317441));
#44494=CARTESIAN_POINT('Ctrl Pts',(-0.142852300121244,0.0329144147112076,
-0.0533864565397581));
#44495=CARTESIAN_POINT('Ctrl Pts',(-0.13196746899842,0.0801750561545543,
-0.0560355536424086));
#44496=CARTESIAN_POINT('Ctrl Pts',(-0.0952960250695133,0.121488128341987,
-0.0586846507450591));
#44497=CARTESIAN_POINT('Ctrl Pts',(-0.0496670712318524,0.137918395416419,
-0.0613337478477096));
#44498=CARTESIAN_POINT('Ctrl Pts',(-0.00403811739418901,0.154348662490852,
-0.0639828449503602));
#44499=CARTESIAN_POINT('Ctrl Pts',(0.0505483463522294,0.145896124452282,
-0.0666319420530108));
#44500=CARTESIAN_POINT('Ctrl Pts',(0.0890656175158321,0.116431454056438,
-0.0692810391556615));
#44501=CARTESIAN_POINT('Ctrl Pts',(0.127582888679433,0.0869667836605948,
-0.071930136258312));
#44502=CARTESIAN_POINT('Ctrl Pts',(0.150030967260219,0.0364899809074799,
-0.0745792333609626));
#44503=CARTESIAN_POINT('Ctrl Pts',(0.146112043556668,-0.0118477202811764,
-0.0772283304636131));
#44504=CARTESIAN_POINT('Ctrl Pts',(0.142193119853117,-0.0601854214698328,
-0.0798774275662636));
#44505=CARTESIAN_POINT('Ctrl Pts',(0.111907193865229,-0.106384021094031,
-0.0825265246689142));
#44506=CARTESIAN_POINT('Ctrl Pts',(0.0691448976157257,-0.129258739853145,
-0.0851756217715646));
#44507=CARTESIAN_POINT('Ctrl Pts',(0.02638260136622,-0.152133458612262,
-0.0878247188742153));
#44508=CARTESIAN_POINT('Ctrl Pts',(-0.028856065144902,-0.151684296506292,
-0.0904738159768659));
#44509=CARTESIAN_POINT('Ctrl Pts',(-0.0712399745379113,-0.128116417425042,
-0.0931229130795165));
#44510=CARTESIAN_POINT('Ctrl Pts',(-0.113623883930918,-0.104548538343794,
-0.0957720101821671));
#44511=CARTESIAN_POINT('Ctrl Pts',(-0.143153036205815,-0.0578619422872685,
-0.0984211072848177));
#44512=CARTESIAN_POINT('Ctrl Pts',(-0.146285101710351,-0.00946718490431867,
-0.101070204387468));
#44513=CARTESIAN_POINT('Ctrl Pts',(-0.146487786263673,-0.0063354273567671,
-0.101241634730217));
#44514=CARTESIAN_POINT('Ctrl Pts',(-0.146579926700862,-0.00319651647499787,
-0.101413065072967));
#44515=CARTESIAN_POINT('Ctrl Pts',(-0.146564414435351,-5.66789191273343E-5,
-0.101584495415716));
#44516=CARTESIAN_POINT('Ctrl Pts',(-0.146581435366625,-3.40469869341234E-5,
-0.10871550458429));
#44517=CARTESIAN_POINT('Ctrl Pts',(-0.146587207092113,-0.00187241585713054,
-0.10861510117927));
#44518=CARTESIAN_POINT('Ctrl Pts',(-0.146555622107311,-0.00371058180105663,
-0.108514697774249));
#44519=CARTESIAN_POINT('Ctrl Pts',(-0.146486066255375,-0.00554730986340993,
-0.108414294369229));
#44520=CARTESIAN_POINT('Ctrl Pts',(-0.144650867480983,-0.0540085247729829,
-0.105765197266578));
#44521=CARTESIAN_POINT('Ctrl Pts',(-0.116382490276587,-0.101468767541441,
-0.103116100163928));
#44522=CARTESIAN_POINT('Ctrl Pts',(-0.0746446598804173,-0.126163050920102,
-0.100467003061277));
#44523=CARTESIAN_POINT('Ctrl Pts',(-0.0329068294842501,-0.150857334298762,
-0.0978179059586271));
#44524=CARTESIAN_POINT('Ctrl Pts',(0.0223004541036862,-0.152785658287626,
-0.0951688088559769));
#44525=CARTESIAN_POINT('Ctrl Pts',(0.0656596537528744,-0.131063848755951,
-0.0925197117533265));
#44526=CARTESIAN_POINT('Ctrl Pts',(0.109018853402065,-0.109342039224275,
-0.0898706146506759));
#44527=CARTESIAN_POINT('Ctrl Pts',(0.140529969112507,-0.0639700961720474,
-0.0872215175480249));
#44528=CARTESIAN_POINT('Ctrl Pts',(0.145742027776359,-0.0157549866249117,
-0.0845724204453744));
#44529=CARTESIAN_POINT('Ctrl Pts',(0.150954086440211,0.0324601229222266,
-0.0819233233427238));
#44530=CARTESIAN_POINT('Ctrl Pts',(0.129867088057477,0.0835183989642793,
-0.0792742262400732));
#44531=CARTESIAN_POINT('Ctrl Pts',(0.0921517725471056,0.114004389811336,
-0.0766251291374225));
#44532=CARTESIAN_POINT('Ctrl Pts',(0.054436457036736,0.14449038065839,-0.0739760320347719));
#44533=CARTESIAN_POINT('Ctrl Pts',(9.28243987341967E-5,0.15440408631045,
-0.0713269349321214));
#44534=CARTESIAN_POINT('Ctrl Pts',(-0.0459583001113908,0.139200118538303,
-0.0686778378294708));
#44535=CARTESIAN_POINT('Ctrl Pts',(-0.0920094246215131,0.123996150766157,
-0.0660287407268205));
#44536=CARTESIAN_POINT('Ctrl Pts',(-0.129768041003757,0.0836745095698077,
-0.0633796436241703));
#44537=CARTESIAN_POINT('Ctrl Pts',(-0.141916889037382,0.0367245704198023,
-0.0607305465215199));
#44538=CARTESIAN_POINT('Ctrl Pts',(-0.144997238974008,0.024820376566606,
-0.0600588658757764));
#44539=CARTESIAN_POINT('Ctrl Pts',(-0.1464311881288,0.012490062696057,-0.059387185230033));
#44540=CARTESIAN_POINT('Ctrl Pts',(-0.146319403921505,0.000134192518820611,
-0.0587155045842896));
#44541=CARTESIAN_POINT('Origin',(0.,0.,-3.06008671147362));
#44542=CARTESIAN_POINT('',(-0.117782368947698,0.000108066697646992,-0.0350867114736242));
#44543=CARTESIAN_POINT('',(-0.117559568560248,-6.5321138236249E-5,-0.0252132885263911));
#44544=CARTESIAN_POINT('',(-0.117775,1.13296574333067E-13,-3.06008671147362));
#44545=CARTESIAN_POINT('',(0.106356886625425,-0.0510349087439493,-0.0136500000000001));
#44546=CARTESIAN_POINT('Ctrl Pts',(-0.117782368947698,0.000108066697646985,
-0.0350867114736242));
#44547=CARTESIAN_POINT('Ctrl Pts',(-0.117498396216706,-0.0301984012316938,
-0.0330382680789872));
#44548=CARTESIAN_POINT('Ctrl Pts',(-0.0901079789233812,-0.100150743397372,
-0.0283407275816995));
#44549=CARTESIAN_POINT('Ctrl Pts',(0.0244229449298219,-0.135448756285299,
-0.0211951570904917));
#44550=CARTESIAN_POINT('Ctrl Pts',(0.0905597122481844,-0.0834873633603501,
-0.0160980299939206));
#44551=CARTESIAN_POINT('Ctrl Pts',(0.106356886625425,-0.0510349087439493,
-0.0136500000000001));
#44552=CARTESIAN_POINT('',(-0.0138313775859597,-0.116960008631475,-0.0136500000000002));
#44553=CARTESIAN_POINT('Origin',(0.,0.,-0.0136500000000002));
#44554=CARTESIAN_POINT('Ctrl Pts',(-0.117559568560248,-6.53211382362472E-5,
-0.0252132885263911));
#44555=CARTESIAN_POINT('Ctrl Pts',(-0.117588588566995,-0.0179836296355686,
-0.0240079561202446));
#44556=CARTESIAN_POINT('Ctrl Pts',(-0.105317098863147,-0.075201842880568,
-0.0201535266114477));
#44557=CARTESIAN_POINT('Ctrl Pts',(-0.0527668217477812,-0.112355607212729,
-0.0162990971026507));
#44558=CARTESIAN_POINT('Ctrl Pts',(-0.0138313775859597,-0.116960008631475,
-0.0136500000000002));
#44559=CARTESIAN_POINT('Origin',(0.,0.,-3.06008671147362));
#44560=CARTESIAN_POINT('',(-0.117947549778773,-4.5612297192055E-5,-0.0850867114736239));
#44561=CARTESIAN_POINT('',(-0.117750377839804,0.000107991280655955,-0.0752132885263904));
#44562=CARTESIAN_POINT('',(-0.117775,1.13296574333067E-13,-3.06008671147362));
#44563=CARTESIAN_POINT('Ctrl Pts',(-0.117947549778773,-4.56122971920513E-5,
-0.0850867114736239));
#44564=CARTESIAN_POINT('Ctrl Pts',(-0.11796003325722,-0.00257239308396317,
-0.0849152811308741));
#44565=CARTESIAN_POINT('Ctrl Pts',(-0.116740051627237,-0.0441330121862037,
-0.0820947536854738));
#44566=CARTESIAN_POINT('Ctrl Pts',(-0.0676751419254551,-0.12170630648443,
-0.0766251291374228));
#44567=CARTESIAN_POINT('Ctrl Pts',(0.0656846246959371,-0.122790694602604,
-0.0686778378294716));
#44568=CARTESIAN_POINT('Ctrl Pts',(0.138802320628112,-0.0112558793500066,
-0.0607305465215197));
#44569=CARTESIAN_POINT('Ctrl Pts',(0.0846071216902694,0.110607573555673,
-0.0527832552135683));
#44570=CARTESIAN_POINT('Ctrl Pts',(-0.0471780665789619,0.131014085359439,
-0.0448359639056163));
#44571=CARTESIAN_POINT('Ctrl Pts',(-0.112892038546555,0.0569824744721723,
-0.0389371159923019));
#44572=CARTESIAN_POINT('Ctrl Pts',(-0.117865636698367,0.00899466438748865,
-0.0356873651816377));
#44573=CARTESIAN_POINT('Ctrl Pts',(-0.117782368947698,0.000108066697646985,
-0.0350867114736242));
#44574=CARTESIAN_POINT('Ctrl Pts',(-0.117750377839804,0.000107991280655946,
-0.0752132885263904));
#44575=CARTESIAN_POINT('Ctrl Pts',(-0.117485542371871,-0.0291651300276833,
-0.0732358720694808));
#44576=CARTESIAN_POINT('Ctrl Pts',(-0.0916414878538697,-0.0980717922490419,
-0.0686093585099205));
#44577=CARTESIAN_POINT('Ctrl Pts',(0.0240158013170603,-0.137163045762996,
-0.0613337478477098));
#44578=CARTESIAN_POINT('Ctrl Pts',(0.128339992499329,-0.0540801177957914,
-0.0533864565397582));
#44579=CARTESIAN_POINT('Ctrl Pts',(0.114921489370477,0.0786438502502632,
-0.0454391652318065));
#44580=CARTESIAN_POINT('Ctrl Pts',(-0.0038420162804081,0.139161560048721,
-0.0374918739238548));
#44581=CARTESIAN_POINT('Ctrl Pts',(-0.101699995939352,0.0823447168505036,
-0.0307499150220496));
#44582=CARTESIAN_POINT('Ctrl Pts',(-0.117524807973858,0.0213974895334067,
-0.0266570532228951));
#44583=CARTESIAN_POINT('Ctrl Pts',(-0.117559568560248,-6.53211382362472E-5,
-0.0252132885263911));
#44584=CARTESIAN_POINT('Origin',(0.,0.,-3.06008671147362));
#44585=CARTESIAN_POINT('',(-0.117644293922143,-8.24728389195078E-5,-0.135086711473624));
#44586=CARTESIAN_POINT('',(-0.117961247354316,-2.73992748022617E-5,-0.12521328852639));
#44587=CARTESIAN_POINT('',(-0.117775,1.13296574333067E-13,-3.06008671147362));
#44588=CARTESIAN_POINT('Ctrl Pts',(-0.117644293922143,-8.24728389195242E-5,
-0.135086711473624));
#44589=CARTESIAN_POINT('Ctrl Pts',(-0.117734495770028,-0.0140816040781494,
-0.134143197080111));
#44590=CARTESIAN_POINT('Ctrl Pts',(-0.108941502454585,-0.0672763816880252,
-0.130550585583947));
#44591=CARTESIAN_POINT('Ctrl Pts',(-0.0299022661697765,-0.136007978091718,
-0.124308876985132));
#44592=CARTESIAN_POINT('Ctrl Pts',(0.0981607747731693,-0.0987763617687909,
-0.116361585677181));
#44593=CARTESIAN_POINT('Ctrl Pts',(0.136192280372371,0.0290514034709051,
-0.108414294369229));
#44594=CARTESIAN_POINT('Ctrl Pts',(0.0493101426383743,0.130233760247366,
-0.100467003061278));
#44595=CARTESIAN_POINT('Ctrl Pts',(-0.0799485994171707,0.112361477994011,
-0.092691142096076));
#44596=CARTESIAN_POINT('Ctrl Pts',(-0.117767127228718,0.0364737148214392,
-0.0875643782335247));
#44597=CARTESIAN_POINT('Ctrl Pts',(-0.117947549778773,-4.56122971920513E-5,
-0.0850867114736239));
#44598=CARTESIAN_POINT('Ctrl Pts',(-0.117961247354316,-2.73992748022543E-5,
-0.12521328852639));
#44599=CARTESIAN_POINT('Ctrl Pts',(-0.117965892143996,-0.001506824581892,
-0.125112885121367));
#44600=CARTESIAN_POINT('Ctrl Pts',(-0.11726983255438,-0.0420157259051257,
-0.122363384613694));
#44601=CARTESIAN_POINT('Ctrl Pts',(-0.0709097346571945,-0.11985045568327,
-0.116964787003371));
#44602=CARTESIAN_POINT('Ctrl Pts',(0.0623742658464559,-0.124505905450053,
-0.109017495695419));
#44603=CARTESIAN_POINT('Ctrl Pts',(0.138449871985116,-0.0149668430727117,
-0.101070204387468));
#44604=CARTESIAN_POINT('Ctrl Pts',(0.0875406563815945,0.108300429783857,
-0.093122913079516));
#44605=CARTESIAN_POINT('Ctrl Pts',(-0.0436582776930319,0.132234560631268,
-0.0851756217715646));
#44606=CARTESIAN_POINT('Ctrl Pts',(-0.112135132893251,0.0591095510259165,
-0.0792057469205228));
#44607=CARTESIAN_POINT('Ctrl Pts',(-0.117840336056494,0.0100513640863849,
-0.0758849691721313));
#44608=CARTESIAN_POINT('Ctrl Pts',(-0.117750377839804,0.000107991280655946,
-0.0752132885263904));
#44609=CARTESIAN_POINT('Origin',(0.,0.,-3.06008671147362));
#44610=CARTESIAN_POINT('',(-0.117647509884266,8.40633693049918E-5,-0.185086711473623));
#44611=CARTESIAN_POINT('',(-0.117668478068114,-9.27795444453927E-5,-0.17521328852639));
#44612=CARTESIAN_POINT('',(-0.117775,1.13296574333067E-13,-3.06008671147362));
#44613=CARTESIAN_POINT('Ctrl Pts',(-0.117647509884266,8.40633693049864E-5,
-0.185086711473623));
#44614=CARTESIAN_POINT('Ctrl Pts',(-0.117480044497517,-0.0253689009508002,
-0.183371113029347));
#44615=CARTESIAN_POINT('Ctrl Pts',(-0.096858013655478,-0.0903716449468221,
-0.17900641748242));
#44616=CARTESIAN_POINT('Ctrl Pts',(0.0103865420804345,-0.138868404314727,
-0.171992624832842));
#44617=CARTESIAN_POINT('Ctrl Pts',(0.12237839822605,-0.0664517977974861,
-0.164045333524891));
#44618=CARTESIAN_POINT('Ctrl Pts',(0.122126615970329,0.0669134043386132,
-0.156098042216939));
#44619=CARTESIAN_POINT('Ctrl Pts',(0.00986212241425144,0.138906633291134,
-0.148150750908988));
#44620=CARTESIAN_POINT('Ctrl Pts',(-0.0970456661352901,0.0900751105073112,
-0.141146973994549));
#44621=CARTESIAN_POINT('Ctrl Pts',(-0.117481236831397,0.025223634146552,
-0.136792294182761));
#44622=CARTESIAN_POINT('Ctrl Pts',(-0.117644293922143,-8.24728389195242E-5,
-0.135086711473624));
#44623=CARTESIAN_POINT('Ctrl Pts',(-0.117668478068114,-9.27795444453997E-5,
-0.17521328852639));
#44624=CARTESIAN_POINT('Ctrl Pts',(-0.117763576635394,-0.0130313762783267,
-0.174340801070604));
#44625=CARTESIAN_POINT('Ctrl Pts',(-0.109825503309218,-0.0651414645689068,
-0.170819216512168));
#44626=CARTESIAN_POINT('Ctrl Pts',(-0.0335329405968919,-0.135158632142634,
-0.16464853485108));
#44627=CARTESIAN_POINT('Ctrl Pts',(0.0954810297919763,-0.101369056556591,
-0.156701243543129));
#44628=CARTESIAN_POINT('Ctrl Pts',(0.136921232711689,0.0253946947183125,
-0.148753952235177));
#44629=CARTESIAN_POINT('Ctrl Pts',(0.0527793109988149,0.128866829226554,
-0.140806660927226));
#44630=CARTESIAN_POINT('Ctrl Pts',(-0.0780963839282828,0.114330198428394,
-0.132959773024297));
#44631=CARTESIAN_POINT('Ctrl Pts',(-0.117843341530487,0.0375271234571879,
-0.127761982224018));
#44632=CARTESIAN_POINT('Ctrl Pts',(-0.117961247354316,-2.73992748022543E-5,
-0.12521328852639));
#44633=CARTESIAN_POINT('Origin',(0.,0.,-3.06008671147362));
#44634=CARTESIAN_POINT('',(-0.117949786367931,4.31836698983784E-5,-0.235086711473623));
#44635=CARTESIAN_POINT('',(-0.117626188250658,7.19124116373773E-5,-0.22521328852639));
#44636=CARTESIAN_POINT('',(-0.117775,1.13296574333067E-13,-3.06008671147362));
#44637=CARTESIAN_POINT('Ctrl Pts',(-0.117949786367931,4.31836698983855E-5,
-0.235086711473623));
#44638=CARTESIAN_POINT('Ctrl Pts',(-0.117777175438158,-0.0366218388289575,
-0.232599028978583));
#44639=CARTESIAN_POINT('Ctrl Pts',(-0.0796904654718219,-0.112640263012373,
-0.227462249380893));
#44640=CARTESIAN_POINT('Ctrl Pts',(0.0498015954015689,-0.130046587870231,
-0.219676372680552));
#44641=CARTESIAN_POINT('Ctrl Pts',(0.136300969518302,-0.0285369869745706,
-0.2117290813726));
#44642=CARTESIAN_POINT('Ctrl Pts',(0.0977871294194325,0.099146312286434,
-0.203781790064648));
#44643=CARTESIAN_POINT('Ctrl Pts',(-0.0304156058568074,0.135894094238902,
-0.195834498756697));
#44644=CARTESIAN_POINT('Ctrl Pts',(-0.109068335787174,0.0669753266805635,
-0.189602805893022));
#44645=CARTESIAN_POINT('Ctrl Pts',(-0.117738631856529,0.0139336376235387,
-0.186020210131997));
#44646=CARTESIAN_POINT('Ctrl Pts',(-0.117647509884266,8.40633693049864E-5,
-0.185086711473623));
#44647=CARTESIAN_POINT('Ctrl Pts',(-0.117626188250658,7.19124116373634E-5,
-0.22521328852639));
#44648=CARTESIAN_POINT('Ctrl Pts',(-0.117490400621603,-0.0243383817240207,
-0.22356871701984));
#44649=CARTESIAN_POINT('Ctrl Pts',(-0.0981703407268072,-0.0882660532411596,
-0.219275048410641));
#44650=CARTESIAN_POINT('Ctrl Pts',(0.00666484966802229,-0.139096705296418,
-0.21233228269879));
#44651=CARTESIAN_POINT('Ctrl Pts',(0.12055539313165,-0.0697044532603406,
-0.204384991390839));
#44652=CARTESIAN_POINT('Ctrl Pts',(0.123874330089505,0.0636196824021741,
-0.196437700082887));
#44653=CARTESIAN_POINT('Ctrl Pts',(0.0135775806509123,0.138592795605587,
-0.188490408774936));
#44654=CARTESIAN_POINT('Ctrl Pts',(-0.0956963157972435,0.0921750501080625,
-0.181415604922769));
#44655=CARTESIAN_POINT('Ctrl Pts',(-0.117474832840424,0.0262535428260036,
-0.176989898173254));
#44656=CARTESIAN_POINT('Ctrl Pts',(-0.117668478068114,-9.27795444453997E-5,
-0.17521328852639));
#44657=CARTESIAN_POINT('Origin',(0.,0.,-3.06008671147362));
#44658=CARTESIAN_POINT('',(-0.117777663481355,-0.000108098457152765,-0.285086711473623));
#44659=CARTESIAN_POINT('',(-0.117931147509827,6.00851020906984E-5,-0.27521328852639));
#44660=CARTESIAN_POINT('',(-0.117775,1.13296574333067E-13,-3.06008671147362));
#44661=CARTESIAN_POINT('Ctrl Pts',(-0.117777663481355,-0.000108098457152784,
-0.285086711473623));
#44662=CARTESIAN_POINT('Ctrl Pts',(-0.117861059495769,-0.0091427624241447,
-0.28447604203047));
#44663=CARTESIAN_POINT('Ctrl Pts',(-0.112781650293578,-0.057277199051128,
-0.281216275484667));
#44664=CARTESIAN_POINT('Ctrl Pts',(-0.0466886511469119,-0.131196355795028,
-0.275307411836213));
#44665=CARTESIAN_POINT('Ctrl Pts',(0.0850271090185907,-0.11028465283889,
-0.267360120528261));
#44666=CARTESIAN_POINT('Ctrl Pts',(0.138757274262191,0.0117784871313546,
-0.25941282922031));
#44667=CARTESIAN_POINT('Ctrl Pts',(0.0652213392245596,0.123038574559143,
-0.251465537912358));
#44668=CARTESIAN_POINT('Ctrl Pts',(-0.0681346343844765,0.121449518390703,
-0.243518246604407));
#44669=CARTESIAN_POINT('Ctrl Pts',(-0.116816528750904,0.043834312617339,
-0.238058637791495));
#44670=CARTESIAN_POINT('Ctrl Pts',(-0.117960986320319,0.00242221324119258,
-0.235248126081234));
#44671=CARTESIAN_POINT('Ctrl Pts',(-0.117949786367931,4.31836698983855E-5,
-0.235086711473623));
#44672=CARTESIAN_POINT('Ctrl Pts',(-0.117931147509827,6.00851020906897E-5,
-0.27521328852639));
#44673=CARTESIAN_POINT('Ctrl Pts',(-0.117709465475371,-0.0355730120958269,
-0.272796632969077));
#44674=CARTESIAN_POINT('Ctrl Pts',(-0.0815010314853682,-0.110656665461582,
-0.267730880309114));
#44675=CARTESIAN_POINT('Ctrl Pts',(0.0463019631218519,-0.131333323447874,
-0.2600160305465));
#44676=CARTESIAN_POINT('Ctrl Pts',(0.135488078736147,-0.0321759872672793,
-0.252068739238548));
#44677=CARTESIAN_POINT('Ctrl Pts',(0.100406551398842,0.0964926840371405,
-0.244121447930597));
#44678=CARTESIAN_POINT('Ctrl Pts',(-0.0267663657998475,0.136659706204361,
-0.236174156622645));
#44679=CARTESIAN_POINT('Ctrl Pts',(-0.108153254503891,0.0691102072572639,
-0.229871436821243));
#44680=CARTESIAN_POINT('Ctrl Pts',(-0.117709129094809,0.0149820365199399,
-0.226217814122491));
#44681=CARTESIAN_POINT('Ctrl Pts',(-0.117626188250658,7.19124116373634E-5,
-0.22521328852639));
#44682=CARTESIAN_POINT('Origin',(0.,0.,-3.06008671147362));
#44683=CARTESIAN_POINT('',(-0.117582262041567,1.42224617900698E-5,-0.335086711473623));
#44684=CARTESIAN_POINT('',(-0.117809707131545,-0.000105358511082676,-0.32521328852639));
#44685=CARTESIAN_POINT('',(-0.117775,1.13296574333067E-13,-3.06008671147362));
#44686=CARTESIAN_POINT('Ctrl Pts',(-0.117582262041567,1.42224617900675E-5,
-0.335086711473623));
#44687=CARTESIAN_POINT('Ctrl Pts',(-0.117560166437186,-0.0205290933732839,
-0.333703957979707));
#44688=CARTESIAN_POINT('Ctrl Pts',(-0.102645223840771,-0.0804595807109724,
-0.32967210738314));
#44689=CARTESIAN_POINT('Ctrl Pts',(-0.00707457914409293,-0.139076469072788,
-0.322991159683922));
#44690=CARTESIAN_POINT('Ctrl Pts',(0.113099750076884,-0.08124506417234,
-0.315043868375971));
#44691=CARTESIAN_POINT('Ctrl Pts',(0.12954067712726,0.0511031005833377,
-0.307096577068019));
#44692=CARTESIAN_POINT('Ctrl Pts',(0.0271688291824932,0.136580264462594,
-0.299149285760068));
#44693=CARTESIAN_POINT('Ctrl Pts',(-0.0903408531884669,0.0998456806777311,
-0.291812663895269));
#44694=CARTESIAN_POINT('Ctrl Pts',(-0.117499285801941,0.0300498030574484,
-0.287125139133121));
#44695=CARTESIAN_POINT('Ctrl Pts',(-0.117777663481355,-0.000108098457152784,
-0.285086711473623));
#44696=CARTESIAN_POINT('Ctrl Pts',(-0.117809707131545,-0.000105358511082682,
-0.32521328852639));
#44697=CARTESIAN_POINT('Ctrl Pts',(-0.117883492862803,-0.00808363414246525,
-0.324673646020964));
#44698=CARTESIAN_POINT('Ctrl Pts',(-0.113504330986124,-0.055146616911953,
-0.321484906412888));
#44699=CARTESIAN_POINT('Ctrl Pts',(-0.0501844769972613,-0.129899314490461,
-0.315647069702161));
#44700=CARTESIAN_POINT('Ctrl Pts',(0.0820439419124697,-0.112521576739974,
-0.30769977839421));
#44701=CARTESIAN_POINT('Ctrl Pts',(0.139022882231082,0.00805927122877484,
-0.299752487086258));
#44702=CARTESIAN_POINT('Ctrl Pts',(0.0684921106044416,0.12124827595279,
-0.291805195778306));
#44703=CARTESIAN_POINT('Ctrl Pts',(-0.0648586022690144,0.123230172231987,
-0.283857904470355));
#44704=CARTESIAN_POINT('Ctrl Pts',(-0.116261197910494,0.0459537469292771,
-0.278327268719716));
#44705=CARTESIAN_POINT('Ctrl Pts',(-0.117952469586325,0.00348738865504856,
-0.275445730071727));
#44706=CARTESIAN_POINT('Ctrl Pts',(-0.117931147509827,6.00851020906897E-5,
-0.27521328852639));
#44707=CARTESIAN_POINT('Origin',(0.,0.,-3.06008671147362));
#44708=CARTESIAN_POINT('',(-0.117829994138202,0.000102010137211548,-0.385086711473623));
#44709=CARTESIAN_POINT('',(-0.117580749259438,-3.1419836459024E-6,-0.375213288526389));
#44710=CARTESIAN_POINT('',(-0.117775,1.13296574333067E-13,-3.06008671147362));
#44711=CARTESIAN_POINT('Ctrl Pts',(-0.117829994138202,0.000102010137211534,
-0.385086711473623));
#44712=CARTESIAN_POINT('Ctrl Pts',(-0.11753924694104,-0.0317417880642616,
-0.382931873928943));
#44713=CARTESIAN_POINT('Ctrl Pts',(-0.0877617986391311,-0.103212422463877,
-0.378127939281613));
#44714=CARTESIAN_POINT('Ctrl Pts',(0.0331346390848385,-0.135256828339786,
-0.370674907531632));
#44715=CARTESIAN_POINT('Ctrl Pts',(0.131657918533283,-0.0453707659986463,
-0.362727616223681));
#44716=CARTESIAN_POINT('Ctrl Pts',(0.109426520779767,0.086128685522627,
-0.354780324915729));
#44717=CARTESIAN_POINT('Ctrl Pts',(-0.0131692480750101,0.138632192599552,
-0.346833033607777));
#44718=CARTESIAN_POINT('Ctrl Pts',(-0.104457444059357,0.0769723455536469,
-0.340268495793742));
#44719=CARTESIAN_POINT('Ctrl Pts',(-0.117602497483033,0.0188280579172152,
-0.336353055082357));
#44720=CARTESIAN_POINT('Ctrl Pts',(-0.117582262041567,1.42224617900675E-5,
-0.335086711473623));
#44721=CARTESIAN_POINT('Ctrl Pts',(-0.117580783791559,-3.14142509273696E-6,
-0.375213288526389));
#44722=CARTESIAN_POINT('Ctrl Pts',(-0.117585410306143,-0.0194918334504725,
-0.3739015619702));
#44723=CARTESIAN_POINT('Ctrl Pts',(-0.10376360996306,-0.0783327349515231,
-0.369940738311361));
#44724=CARTESIAN_POINT('Ctrl Pts',(-0.0107955825619163,-0.138837203348852,
-0.363330817549871));
#44725=CARTESIAN_POINT('Ctrl Pts',(0.11088400591638,-0.0842439960384028,
-0.35538352624192));
#44726=CARTESIAN_POINT('Ctrl Pts',(0.130862439686628,0.0476165466602282,
-0.347436234933967));
#44727=CARTESIAN_POINT('Ctrl Pts',(0.0308157975764226,0.135803903685831,
-0.339488943626016));
#44728=CARTESIAN_POINT('Ctrl Pts',(-0.0887820097619692,0.101903565882743,
-0.33208129482349));
#44729=CARTESIAN_POINT('Ctrl Pts',(-0.11752127979595,0.0310816033003742,
-0.327322743123614));
#44730=CARTESIAN_POINT('Ctrl Pts',(-0.117809707131545,-0.000105358511082682,
-0.32521328852639));
#44731=CARTESIAN_POINT('Origin',(0.,0.,-3.06008671147362));
#44732=CARTESIAN_POINT('',(-0.117916722700972,-6.98402240337386E-5,-0.435086711473622));
#44733=CARTESIAN_POINT('',(-0.117798146306824,0.000106700477578273,-0.425213288526389));
#44734=CARTESIAN_POINT('',(-0.117775,1.13296574333067E-13,-3.06008671147362));
#44735=CARTESIAN_POINT('Ctrl Pts',(-0.117916722700972,-6.98402240337384E-5,
-0.435086711473622));
#44736=CARTESIAN_POINT('Ctrl Pts',(-0.117945481990475,-0.00416762653193182,
-0.43480888698083));
#44737=CARTESIAN_POINT('Ctrl Pts',(-0.115890583470698,-0.04730923266947,
-0.431881965385387));
#44738=CARTESIAN_POINT('Ctrl Pts',(-0.0627408721263131,-0.124321747432419,
-0.426305946687293));
#44739=CARTESIAN_POINT('Ctrl Pts',(0.0705564186542189,-0.120058759391021,
-0.418358655379342));
#44740=CARTESIAN_POINT('Ctrl Pts',(0.139140415665318,-0.0056796697353837,
-0.41041136407139));
#44741=CARTESIAN_POINT('Ctrl Pts',(0.0801069008200053,0.113908728203041,
-0.402464072763439));
#44742=CARTESIAN_POINT('Ctrl Pts',(-0.0523994674467565,0.129021741311752,
-0.394516781455487));
#44743=CARTESIAN_POINT('Ctrl Pts',(-0.113948945296141,0.0537861578315203,
-0.388724327692215));
#44744=CARTESIAN_POINT('Ctrl Pts',(-0.117896683425988,0.00740608819267113,
-0.385580971031594));
#44745=CARTESIAN_POINT('Ctrl Pts',(-0.117829994138202,0.000102010137211534,
-0.385086711473623));
#44746=CARTESIAN_POINT('Ctrl Pts',(-0.117798146306824,0.000106700477578266,
-0.425213288526389));
#44747=CARTESIAN_POINT('Ctrl Pts',(-0.117512496286999,-0.030708896715437,
-0.423129477919436));
#44748=CARTESIAN_POINT('Ctrl Pts',(-0.0893501311828865,-0.101161866296878,
-0.418396570209834));
#44749=CARTESIAN_POINT('Ctrl Pts',(0.0295014860686701,-0.136095466332724,
-0.41101456539758));
#44750=CARTESIAN_POINT('Ctrl Pts',(0.130395995936294,-0.0488794218497269,
-0.403067274089629));
#44751=CARTESIAN_POINT('Ctrl Pts',(0.111693245167184,0.083168098575145,
-0.395119982781677));
#44752=CARTESIAN_POINT('Ctrl Pts',(-0.00945288246871811,0.138935080701795,
-0.387172691473725));
#44753=CARTESIAN_POINT('Ctrl Pts',(-0.103364419861196,0.0791009627546925,
-0.380537126721963));
#44754=CARTESIAN_POINT('Ctrl Pts',(-0.117576066829546,0.0198665506085378,
-0.376550659072851));
#44755=CARTESIAN_POINT('Ctrl Pts',(-0.117580783791559,-3.14142509273696E-6,
-0.375213288526389));
#44756=CARTESIAN_POINT('Origin',(0.,0.,-3.06008671147362));
#44757=CARTESIAN_POINT('',(-0.117614497320444,-6.31649834024115E-5,-0.485086711473622));
#44758=CARTESIAN_POINT('',(-0.117938472244188,-5.41950633561744E-5,-0.475213288526389));
#44759=CARTESIAN_POINT('',(-0.117775,1.13296574333067E-13,-3.06008671147362));
#44760=CARTESIAN_POINT('Ctrl Pts',(-0.117614497320444,-6.31649834024247E-5,
-0.485086711473622));
#44761=CARTESIAN_POINT('Ctrl Pts',(-0.117690187679668,-0.0156507863039807,
-0.484036802930066));
#44762=CARTESIAN_POINT('Ctrl Pts',(-0.107549344443015,-0.0704740980699968,
-0.48033779728386));
#44763=CARTESIAN_POINT('Ctrl Pts',(-0.0244244560972015,-0.137097628951694,
-0.473989694535004));
#44764=CARTESIAN_POINT('Ctrl Pts',(0.102042666874295,-0.0947607938812361,
-0.466042403227051));
#44765=CARTESIAN_POINT('Ctrl Pts',(0.134917779304342,0.0344892265411343,
-0.4580951119191));
#44766=CARTESIAN_POINT('Ctrl Pts',(0.0440483189035268,0.132106243310428,
-0.450147820611148));
#44767=CARTESIAN_POINT('Ctrl Pts',(-0.0826326171253195,0.10938061617266,
-0.442478353795989));
#44768=CARTESIAN_POINT('Ctrl Pts',(-0.117671257966059,0.0349053642127825,
-0.43745798408348));
#44769=CARTESIAN_POINT('Ctrl Pts',(-0.117916722700972,-6.98402240337384E-5,
-0.435086711473622));
#44770=CARTESIAN_POINT('Ctrl Pts',(-0.117938472244188,-5.41950633561714E-5,
-0.475213288526389));
#44771=CARTESIAN_POINT('Ctrl Pts',(-0.117955888778364,-0.00310288257415361,
-0.475006490971324));
#44772=CARTESIAN_POINT('Ctrl Pts',(-0.116465154288894,-0.0451882515470556,
-0.472150596313608));
#44773=CARTESIAN_POINT('Ctrl Pts',(-0.0660468875011581,-0.122597399189343,
-0.466645604553241));
#44774=CARTESIAN_POINT('Ctrl Pts',(0.0673167536278285,-0.121904751005003,
-0.45869831324529));
#44775=CARTESIAN_POINT('Ctrl Pts',(0.138938473380797,-0.00940288525907187,
-0.450751021937338));
#44776=CARTESIAN_POINT('Ctrl Pts',(0.0831278997256812,0.111723166459686,
-0.442803730629387));
#44777=CARTESIAN_POINT('Ctrl Pts',(-0.0489263424431069,0.1303783979489,
-0.434856439321435));
#44778=CARTESIAN_POINT('Ctrl Pts',(-0.113247210086591,0.0559156688588903,
-0.428992958620436));
#44779=CARTESIAN_POINT('Ctrl Pts',(-0.117875636121955,0.00846621304170956,
-0.425778575022087));
#44780=CARTESIAN_POINT('Ctrl Pts',(-0.117798146306824,0.000106700477578266,
-0.425213288526389));
#44781=CARTESIAN_POINT('Origin',(0.,0.,-3.06008671147362));
#44782=CARTESIAN_POINT('',(-0.117685468281101,9.81124517920193E-5,-0.535086711473622));
#44783=CARTESIAN_POINT('',(-0.117633476200538,-7.65294932578153E-5,-0.525213288526388));
#44784=CARTESIAN_POINT('',(-0.117775,1.13296574333067E-13,-3.06008671147362));
#44785=CARTESIAN_POINT('Ctrl Pts',(-0.117685468281101,9.81124517920162E-5,
-0.535086711473622));
#44786=CARTESIAN_POINT('Ctrl Pts',(-0.117473376022059,-0.0269113827363188,
-0.533264718879303));
#44787=CARTESIAN_POINT('Ctrl Pts',(-0.094811321954978,-0.0935130246987491,
-0.528793629182333));
#44788=CARTESIAN_POINT('Ctrl Pts',(0.0159466578264506,-0.13834022561781,
-0.521673442382713));
#44789=CARTESIAN_POINT('Ctrl Pts',(0.124944615327587,-0.0614911133454406,
-0.513726151074761));
#44790=CARTESIAN_POINT('Ctrl Pts',(0.119345237096187,0.071756730013814,
-0.50577885976681));
#44791=CARTESIAN_POINT('Ctrl Pts',(0.00428418924635087,0.139190371945483,
-0.497831568458857));
#44792=CARTESIAN_POINT('Ctrl Pts',(-0.0989865471327881,0.0869175656192404,
-0.490934185694462));
#44793=CARTESIAN_POINT('Ctrl Pts',(-0.117499208081921,0.0236794227232818,
-0.486685900032717));
#44794=CARTESIAN_POINT('Ctrl Pts',(-0.117614497320444,-6.31649834024247E-5,
-0.485086711473622));
#44795=CARTESIAN_POINT('Ctrl Pts',(-0.117633476200538,-7.65294932578171E-5,
-0.525213288526388));
#44796=CARTESIAN_POINT('Ctrl Pts',(-0.117719816016294,-0.0146037641429175,
-0.52423440692056));
#44797=CARTESIAN_POINT('Ctrl Pts',(-0.108487849042328,-0.0683394445861028,
-0.52060642821208));
#44798=CARTESIAN_POINT('Ctrl Pts',(-0.0280862598533812,-0.136394558703894,
-0.514329352400952));
#44799=CARTESIAN_POINT('Ctrl Pts',(0.0994690254013135,-0.0974588457878242,
-0.506382061092999));
#44800=CARTESIAN_POINT('Ctrl Pts',(0.135792805648636,0.0308646654064759,
-0.498434769785048));
#44801=CARTESIAN_POINT('Ctrl Pts',(0.0475694519664141,0.130879566305045,
-0.490487478477097));
#44802=CARTESIAN_POINT('Ctrl Pts',(-0.0808529189036142,0.111374779294211,
-0.48274698472421));
#44803=CARTESIAN_POINT('Ctrl Pts',(-0.117732781255603,0.0359511055119116,
-0.477655588073974));
#44804=CARTESIAN_POINT('Ctrl Pts',(-0.117938472244188,-5.41950633561714E-5,
-0.475213288526389));
#44805=CARTESIAN_POINT('Origin',(0.,0.,-3.06008671147362));
#44806=CARTESIAN_POINT('',(-0.117966591322209,1.51587796647229E-5,-0.585086711473623));
#44807=CARTESIAN_POINT('',(-0.117659387014888,8.93238483695505E-5,-0.575213288526388));
#44808=CARTESIAN_POINT('',(-0.117775,1.13296574333067E-13,-3.06008671147362));
#44809=CARTESIAN_POINT('Ctrl Pts',(-0.117966591322209,1.51587796647183E-5,
-0.585086711473623));
#44810=CARTESIAN_POINT('Ctrl Pts',(-0.117897493436053,-0.0382034176156981,
-0.58249263482854));
#44811=CARTESIAN_POINT('Ctrl Pts',(-0.076887247580097,-0.115578456916855,
-0.577249461080806));
#44812=CARTESIAN_POINT('Ctrl Pts',(0.0549762653464128,-0.127945004468253,
-0.569357190230422));
#44813=CARTESIAN_POINT('Ctrl Pts',(0.137335646484491,-0.02304851675287,
-0.561409898922471));
#44814=CARTESIAN_POINT('Ctrl Pts',(0.0937328231132788,0.102987726409681,
-0.553462607614519));
#44815=CARTESIAN_POINT('Ctrl Pts',(-0.0358403461692648,0.134565164534837,
-0.545515316306567));
#44816=CARTESIAN_POINT('Ctrl Pts',(-0.11037166930448,0.0637774950500043,
-0.539390017592935));
#44817=CARTESIAN_POINT('Ctrl Pts',(-0.117781748839092,0.0123592354154572,
-0.535913815981954));
#44818=CARTESIAN_POINT('Ctrl Pts',(-0.117685468281101,9.81124517920162E-5,
-0.535086711473622));
#44819=CARTESIAN_POINT('Ctrl Pts',(-0.117659387014888,8.93238483695418E-5,
-0.575213288526388));
#44820=CARTESIAN_POINT('Ctrl Pts',(-0.117476584431924,-0.0258817614303258,
-0.573462322869796));
#44821=CARTESIAN_POINT('Ctrl Pts',(-0.0961884985075474,-0.0914176792266589,
-0.569062260110554));
#44822=CARTESIAN_POINT('Ctrl Pts',(0.0122371135094518,-0.13871757887715,
-0.562013100248661));
#44823=CARTESIAN_POINT('Ctrl Pts',(0.123253503998567,-0.0648142529746122,
-0.554065808940709));
#44824=CARTESIAN_POINT('Ctrl Pts',(0.121223620817521,0.0685357380676061,
-0.546118517632758));
#44825=CARTESIAN_POINT('Ctrl Pts',(0.00800924251344417,0.139025773405302,
-0.538171226324806));
#44826=CARTESIAN_POINT('Ctrl Pts',(-0.0977014684982498,0.0890269837912308,
-0.531202816622683));
#44827=CARTESIAN_POINT('Ctrl Pts',(-0.117486158999552,0.0247105461789745,
-0.52688350402321));
#44828=CARTESIAN_POINT('Ctrl Pts',(-0.117633476200538,-7.65294932578171E-5,
-0.525213288526388));
#44829=CARTESIAN_POINT('Origin',(0.,0.,-3.06008671147362));
#44830=CARTESIAN_POINT('',(-0.117730596314636,-0.000106536436396233,-0.635086711473622));
#44831=CARTESIAN_POINT('',(-0.117956987195077,3.41556508710135E-5,-0.625213288526389));
#44832=CARTESIAN_POINT('',(-0.117775,1.13296574333067E-13,-3.06008671147362));
#44833=CARTESIAN_POINT('Ctrl Pts',(-0.117730596314636,-0.000106536436396257,
-0.635086711473622));
#44834=CARTESIAN_POINT('Ctrl Pts',(-0.117823857820801,-0.0107260812779556,
-0.634369647880426));
#44835=CARTESIAN_POINT('Ctrl Pts',(-0.111636663996842,-0.0604713644574023,
-0.63100348718458));
#44836=CARTESIAN_POINT('Ctrl Pts',(-0.0413902711963712,-0.13296300000418,
-0.624988229386083));
#44837=CARTESIAN_POINT('Ctrl Pts',(0.0893810158703018,-0.106786459449753,
-0.617040938078132));
#44838=CARTESIAN_POINT('Ctrl Pts',(0.138173369655621,0.0173330273706489,
-0.60909364677018));
#44839=CARTESIAN_POINT('Ctrl Pts',(0.0602351717464476,0.125554920271953,
-0.60114635546223));
#44840=CARTESIAN_POINT('Ctrl Pts',(-0.072949826366452,0.118619714857712,
-0.593199064154276));
#44841=CARTESIAN_POINT('Ctrl Pts',(-0.117593007644085,0.0406641950725845,
-0.587845849491409));
#44842=CARTESIAN_POINT('Ctrl Pts',(-0.117968056890823,0.000825776139351177,
-0.58514173193119));
#44843=CARTESIAN_POINT('Ctrl Pts',(-0.117966591322209,1.51587796647183E-5,
-0.585086711473623));
#44844=CARTESIAN_POINT('Ctrl Pts',(-0.117956987195077,3.41556508710156E-5,
-0.625213288526388));
#44845=CARTESIAN_POINT('Ctrl Pts',(-0.117814604554168,-0.037146083313863,
-0.622690238819033));
#44846=CARTESIAN_POINT('Ctrl Pts',(-0.0787707968119144,-0.113621523240544,
-0.617518092009027));
#44847=CARTESIAN_POINT('Ctrl Pts',(0.0515310444452701,-0.129371036538173,
-0.609696848096371));
#44848=CARTESIAN_POINT('Ctrl Pts',(0.136669329383979,-0.0267171862724199,
-0.601749556788419));
#44849=CARTESIAN_POINT('Ctrl Pts',(0.0964565459097508,0.100441268349926,
-0.593802265480467));
#44850=CARTESIAN_POINT('Ctrl Pts',(-0.0322247413590565,0.135476491248201,
-0.585854974172516));
#44851=CARTESIAN_POINT('Ctrl Pts',(-0.109510475119334,0.065912251287834,
-0.579658648521156));
#44852=CARTESIAN_POINT('Ctrl Pts',(-0.117753152844938,0.0134108006513239,
-0.576111419972447));
#44853=CARTESIAN_POINT('Ctrl Pts',(-0.117659387014888,8.93238483695418E-5,
-0.575213288526388));
#44854=CARTESIAN_POINT('Origin',(0.,0.,-3.06008671147362));
#44855=CARTESIAN_POINT('',(-0.117593034504333,3.94353800751308E-5,-0.685086711473621));
#44856=CARTESIAN_POINT('',(-0.1177617944348,-0.000108325507588214,-0.675213288526388));
#44857=CARTESIAN_POINT('',(-0.117775,1.13296574333067E-13,-3.06008671147362));
#44858=CARTESIAN_POINT('Ctrl Pts',(-0.117593034504333,3.94353800751042E-5,
-0.685086711473621));
#44859=CARTESIAN_POINT('Ctrl Pts',(-0.117526714862022,-0.0220795022350645,
-0.683597563829663));
#44860=CARTESIAN_POINT('Ctrl Pts',(-0.100894498114864,-0.0836391338586082,
-0.679459319083053));
#44861=CARTESIAN_POINT('Ctrl Pts',(-0.00149207632259066,-0.13924829488388,
-0.672671977233793));
#44862=CARTESIAN_POINT('Ctrl Pts',(0.116266623106448,-0.0766445449542468,
-0.664724685925842));
#44863=CARTESIAN_POINT('Ctrl Pts',(0.12738731170417,0.0562564372903673,
-0.65677739461789));
#44864=CARTESIAN_POINT('Ctrl Pts',(0.0216702599226566,0.13755985517114,
-0.648830103309939));
#44865=CARTESIAN_POINT('Ctrl Pts',(-0.0925905262321655,0.0967434292388231,
-0.641599875595182));
#44866=CARTESIAN_POINT('Ctrl Pts',(-0.117479315456474,0.0285064299500534,
-0.637018744983077));
#44867=CARTESIAN_POINT('Ctrl Pts',(-0.117730596314636,-0.000106536436396257,
-0.635086711473622));
#44868=CARTESIAN_POINT('Ctrl Pts',(-0.1177617944348,-0.00010832550758821,
-0.675213288526388));
#44869=CARTESIAN_POINT('Ctrl Pts',(-0.117849137564383,-0.00966952653099531,
-0.67456725187092));
#44870=CARTESIAN_POINT('Ctrl Pts',(-0.112409423629664,-0.0583386690669818,
-0.671272118112801));
#44871=CARTESIAN_POINT('Ctrl Pts',(-0.0449352953335994,-0.131807180646063,
-0.665327887252032));
#44872=CARTESIAN_POINT('Ctrl Pts',(0.086489946256864,-0.109141205935553,
-0.657380595944081));
#44873=CARTESIAN_POINT('Ctrl Pts',(0.138587900451223,0.0136274533609135,
-0.649433304636128));
#44874=CARTESIAN_POINT('Ctrl Pts',(0.0635751014943803,0.123897215895116,
-0.641486013328178));
#44875=CARTESIAN_POINT('Ctrl Pts',(-0.0697478313652302,0.120530301818377,
-0.633538722020224));
#44876=CARTESIAN_POINT('Ctrl Pts',(-0.117081947198759,0.0427798822024834,
-0.628114480419629));
#44877=CARTESIAN_POINT('Ctrl Pts',(-0.1179641003966,0.00189161896770185,
-0.625339335921684));
#44878=CARTESIAN_POINT('Ctrl Pts',(-0.117956987195077,3.41556508710156E-5,
-0.625213288526388));
#44879=CARTESIAN_POINT('Origin',(0.,0.,-3.06008671147362));
#44880=CARTESIAN_POINT('',(-0.117875484466013,8.93978020177876E-5,-0.735086711473622));
#44881=CARTESIAN_POINT('',(-0.117584714802368,2.27631449018287E-5,-0.725213288526388));
#44882=CARTESIAN_POINT('',(-0.117775,1.13296574333067E-13,-3.06008671147362));
#44883=CARTESIAN_POINT('Ctrl Pts',(-0.117875484466013,8.93978020177879E-5,
-0.735086711473622));
#44884=CARTESIAN_POINT('Ctrl Pts',(-0.117594165739836,-0.0332932738978478,
-0.732825479778899));
#44885=CARTESIAN_POINT('Ctrl Pts',(-0.0852952950029288,-0.106260690388895,
-0.727915150981525));
#44886=CARTESIAN_POINT('Ctrl Pts',(0.0385316388930217,-0.133819380973154,
-0.720355725081504));
#44887=CARTESIAN_POINT('Ctrl Pts',(0.13337134577548,-0.0400549378461348,
-0.712408433773551));
#44888=CARTESIAN_POINT('Ctrl Pts',(0.105884845571219,0.0904472962458246,
-0.7044611424656));
#44889=CARTESIAN_POINT('Ctrl Pts',(-0.018717654110887,0.137992620615763,
-0.696513851157648));
#44890=CARTESIAN_POINT('Ctrl Pts',(-0.106021654180243,0.0737796804798823,
-0.690055707493655));
#44891=CARTESIAN_POINT('Ctrl Pts',(-0.117644693205544,0.0172686535960106,
-0.686246660932313));
#44892=CARTESIAN_POINT('Ctrl Pts',(-0.117593034504333,3.94353800751042E-5,
-0.685086711473621));
#44893=CARTESIAN_POINT('Ctrl Pts',(-0.117584714802368,2.27631449018183E-5,
-0.725213288526388));
#44894=CARTESIAN_POINT('Ctrl Pts',(-0.11754840398394,-0.0210449003143397,
-0.723795167820157));
#44895=CARTESIAN_POINT('Ctrl Pts',(-0.102073372171732,-0.0815174398122862,
-0.719727950011274));
#44896=CARTESIAN_POINT('Ctrl Pts',(-0.00521968128764912,-0.139158429726111,
-0.713011635099741));
#44897=CARTESIAN_POINT('Ctrl Pts',(0.114172914890457,-0.0797299137212506,
-0.705064343791791));
#44898=CARTESIAN_POINT('Ctrl Pts',(0.128847818153508,0.0528256887665676,
-0.697117052483838));
#44899=CARTESIAN_POINT('Ctrl Pts',(0.0253454263276182,0.136930358214871,
-0.689169761175887));
#44900=CARTESIAN_POINT('Ctrl Pts',(-0.0910999775854965,0.0988169360777528,
-0.681868506523403));
#44901=CARTESIAN_POINT('Ctrl Pts',(-0.117490983844226,0.0295365304544467,
-0.67721634897357));
#44902=CARTESIAN_POINT('Ctrl Pts',(-0.1177617944348,-0.00010832550758821,
-0.675213288526388));
#44903=CARTESIAN_POINT('Origin',(0.,0.,-3.06008671147362));
#44904=CARTESIAN_POINT('',(-0.117876965213514,-8.8851257191466E-5,-0.785086711473622));
#44905=CARTESIAN_POINT('',(-0.117845523526878,9.85473074824224E-5,-0.775213288526388));
#44906=CARTESIAN_POINT('',(-0.117775,1.13296574333067E-13,-3.06008671147362));
#44907=CARTESIAN_POINT('Ctrl Pts',(-0.117876965213514,-8.88512571914774E-5,
-0.785086711473622));
#44908=CARTESIAN_POINT('Ctrl Pts',(-0.117924564182101,-0.00576090399454924,
-0.784702492830786));
#44909=CARTESIAN_POINT('Ctrl Pts',(-0.114972566077973,-0.0504906643974819,
-0.7816691770853));
#44910=CARTESIAN_POINT('Ctrl Pts',(-0.0577052458335282,-0.126737597117481,
-0.775986764237163));
#44911=CARTESIAN_POINT('Ctrl Pts',(0.0753138949338155,-0.117132963548775,
-0.768039472929213));
#44912=CARTESIAN_POINT('Ctrl Pts',(0.139256255718067,-9.57246296715326E-5,
-0.760092181621259));
#44913=CARTESIAN_POINT('Ctrl Pts',(0.075474857879039,0.117029311490581,
-0.75214489031331));
#44914=CARTESIAN_POINT('Ctrl Pts',(-0.0575309527532313,0.126816810380666,
-0.744197599005357));
#44915=CARTESIAN_POINT('Ctrl Pts',(-0.11493986229245,0.0505997987675953,
-0.738511539392129));
#44916=CARTESIAN_POINT('Ctrl Pts',(-0.117923738611195,0.00581547337703481,
-0.73547457688155));
#44917=CARTESIAN_POINT('Ctrl Pts',(-0.117875484466013,8.93978020177879E-5,
-0.735086711473622));
#44918=CARTESIAN_POINT('Ctrl Pts',(-0.117845523526878,9.8547307482425E-5,
-0.775213288526388));
#44919=CARTESIAN_POINT('Ctrl Pts',(-0.117555464158849,-0.0322568831287426,
-0.773023083769393));
#44920=CARTESIAN_POINT('Ctrl Pts',(-0.086953565764276,-0.10422895270096,
-0.768183781909747));
#44921=CARTESIAN_POINT('Ctrl Pts',(0.0349350364218175,-0.134803029887269,
-0.760695382947452));
#44922=CARTESIAN_POINT('Ctrl Pts',(0.132251131348421,-0.0436113734436843,
-0.752748091639499));
#44923=CARTESIAN_POINT('Ctrl Pts',(0.108268463135797,0.087579983596677,
-0.744800800331548));
#44924=CARTESIAN_POINT('Ctrl Pts',(-0.0150164229970535,0.138444287267318,
-0.736853509023596));
#44925=CARTESIAN_POINT('Ctrl Pts',(-0.10498705715791,0.075911527904859,
-0.730324338421876));
#44926=CARTESIAN_POINT('Ctrl Pts',(-0.117616233812155,0.0183102025229871,
-0.726444264922807));
#44927=CARTESIAN_POINT('Ctrl Pts',(-0.117584714802368,2.27631449018183E-5,
-0.725213288526388));
#44928=CARTESIAN_POINT('Origin',(0.,0.,-3.06008671147362));
#44929=CARTESIAN_POINT('',(-0.117593581734726,-4.02682066843004E-5,-0.835086711473621));
#44930=CARTESIAN_POINT('',(-0.117904332456761,-7.67924259059416E-5,-0.825213288526388));
#44931=CARTESIAN_POINT('',(-0.117775,1.13296574333067E-13,-3.06008671147362));
#44932=CARTESIAN_POINT('Ctrl Pts',(-0.117593581734727,-4.02682066843133E-5,
-0.83508671147362));
#44933=CARTESIAN_POINT('Ctrl Pts',(-0.117646179449728,-0.0172151199308131,
-0.833930408780022));
#44934=CARTESIAN_POINT('Ctrl Pts',(-0.106073737451821,-0.0736701797484393,
-0.830125008983773));
#44935=CARTESIAN_POINT('Ctrl Pts',(-0.0189073483484057,-0.137966757221631,
-0.823670512084875));
#44936=CARTESIAN_POINT('Ctrl Pts',(0.105760398778781,-0.0905927810036414,
-0.81572322077692));
#44937=CARTESIAN_POINT('Ctrl Pts',(0.133426287168139,0.0398715413841222,
-0.807775929468972));
#44938=CARTESIAN_POINT('Ctrl Pts',(0.038715577045716,0.133766281303764,
-0.799828638161018));
#44939=CARTESIAN_POINT('Ctrl Pts',(-0.0852088813915643,0.106364641204736,
-0.792265565495903));
#44940=CARTESIAN_POINT('Ctrl Pts',(-0.117596380497826,0.0333465645075948,
-0.787351589933437));
#44941=CARTESIAN_POINT('Ctrl Pts',(-0.117876965213514,-8.88512571914774E-5,
-0.785086711473622));
#44942=CARTESIAN_POINT('Ctrl Pts',(-0.117904332456761,-7.67924259059459E-5,
-0.825213288526388));
#44943=CARTESIAN_POINT('Ctrl Pts',(-0.117939220517964,-0.00469750316242473,
-0.82490009682128));
#44944=CARTESIAN_POINT('Ctrl Pts',(-0.115593117736479,-0.0483662331465746,
-0.821937808013521));
#44945=CARTESIAN_POINT('Ctrl Pts',(-0.0610777466931965,-0.1251472033066,
-0.816326422103112));
#44946=CARTESIAN_POINT('Ctrl Pts',(0.0721508577441712,-0.119107377451451,
-0.808379130795161));
#44947=CARTESIAN_POINT('Ctrl Pts',(0.139203772684067,-0.00382404329272468,
-0.800431839487209));
#44948=CARTESIAN_POINT('Ctrl Pts',(0.0785810656558809,0.114966646280423,
-0.792484548179258));
#44949=CARTESIAN_POINT('Ctrl Pts',(-0.0541150215622158,0.12831164435819,
-0.784537256871306));
#44950=CARTESIAN_POINT('Ctrl Pts',(-0.114286285428402,0.0527264646981619,
-0.778780170320349));
#44951=CARTESIAN_POINT('Ctrl Pts',(-0.117906296851084,0.00687766662048267,
-0.775672180872043));
#44952=CARTESIAN_POINT('Ctrl Pts',(-0.117845523526878,9.8547307482425E-5,
-0.775213288526388));
#44953=CARTESIAN_POINT('Origin',(0.,0.,-3.06008671147362));
#44954=CARTESIAN_POINT('',(-0.117729028952017,0.000106365187095507,-0.885086711473621));
#44955=CARTESIAN_POINT('',(-0.117606504447261,-5.5889115292404E-5,-0.875213288526388));
#44956=CARTESIAN_POINT('',(-0.117775,1.13296574333067E-13,-3.06008671147362));
#44957=CARTESIAN_POINT('Ctrl Pts',(-0.117729028952017,0.000106365187095494,
-0.885086711473621));
#44958=CARTESIAN_POINT('Ctrl Pts',(-0.117478889294716,-0.0284535591076875,
-0.883158324729259));
#44959=CARTESIAN_POINT('Ctrl Pts',(-0.0926658391403091,-0.0966367106808196,
-0.878580840882248));
#44960=CARTESIAN_POINT('Ctrl Pts',(0.0214811224820551,-0.137589517394064,
-0.871354259932582));
#44961=CARTESIAN_POINT('Ctrl Pts',(0.127309850102664,-0.0564315158989901,
-0.863406968624633));
#44962=CARTESIAN_POINT('Ctrl Pts',(0.116371883968419,0.0764846294458023,
-0.855459677316679));
#44963=CARTESIAN_POINT('Ctrl Pts',(-0.0013006366881828,0.139250214592387,
-0.847512386008729));
#44964=CARTESIAN_POINT('Ctrl Pts',(-0.100832864752058,0.0837479595872449,
-0.840721397394375));
#44965=CARTESIAN_POINT('Ctrl Pts',(-0.117525677737513,0.0221325787234608,
-0.836579505882672));
#44966=CARTESIAN_POINT('Ctrl Pts',(-0.117593581734727,-4.02682066843133E-5,
-0.83508671147362));
#44967=CARTESIAN_POINT('Ctrl Pts',(-0.117606504447261,-5.58891152924006E-5,
-0.875213288526387));
#44968=CARTESIAN_POINT('Ctrl Pts',(-0.117675456234588,-0.0161713341894999,
-0.874128012770516));
#44969=CARTESIAN_POINT('Ctrl Pts',(-0.107068193774824,-0.0715367874318198,
-0.870393639911994));
#44970=CARTESIAN_POINT('Ctrl Pts',(-0.0225943993144704,-0.137411086729565,
-0.864010169950823));
#44971=CARTESIAN_POINT('Ctrl Pts',(0.103297016147289,-0.0933918630912153,
-0.856062878642869));
#44972=CARTESIAN_POINT('Ctrl Pts',(0.134445950642072,0.0362849830168238,
-0.848115587334919));
#44973=CARTESIAN_POINT('Ctrl Pts',(0.0422830665105441,0.132681784443256,
-0.840168296026967));
#44974=CARTESIAN_POINT('Ctrl Pts',(-0.0835008827885007,0.108381751794679,
-0.832534196424123));
#44975=CARTESIAN_POINT('Ctrl Pts',(-0.117644123743871,0.0343862631847281,
-0.827549193923931));
#44976=CARTESIAN_POINT('Ctrl Pts',(-0.117904332456761,-7.67924259059459E-5,
-0.825213288526388));
#44977=CARTESIAN_POINT('Origin',(0.,0.,-3.06008671147362));
#44978=CARTESIAN_POINT('',(-0.117966893777284,-1.41613286548E-5,-0.935086711473621));
#44979=CARTESIAN_POINT('',(-0.117699425459372,0.000101537840546506,-0.925213288526387));
#44980=CARTESIAN_POINT('',(-0.117775,1.13296574333067E-13,-3.06008671147362));
#44981=CARTESIAN_POINT('Ctrl Pts',(-0.117966893777284,-1.41613286548282E-5,
-0.935086711473621));
#44982=CARTESIAN_POINT('Ctrl Pts',(-0.11796817649413,-0.000771045615368247,
-0.935035337781146));
#44983=CARTESIAN_POINT('Ctrl Pts',(-0.117618462361427,-0.0405556373780832,
-0.932334866986021));
#44984=CARTESIAN_POINT('Ctrl Pts',(-0.0731128355279682,-0.118519311510323,
-0.926985299088244));
#44985=CARTESIAN_POINT('Ctrl Pts',(0.0600625022165961,-0.125637612788934,
-0.919038007780293));
#44986=CARTESIAN_POINT('Ctrl Pts',(0.138149409672222,-0.0175229714100354,
-0.911090716472342));
#44987=CARTESIAN_POINT('Ctrl Pts',(0.0895277411724023,0.106663477724982,
-0.903143425164389));
#44988=CARTESIAN_POINT('Ctrl Pts',(-0.0412074348652185,0.133019777595849,
-0.895196133856439));
#44989=CARTESIAN_POINT('Ctrl Pts',(-0.111596070039508,0.0605808954844544,
-0.889177229292848));
#44990=CARTESIAN_POINT('Ctrl Pts',(-0.117822515511475,0.0107802786701471,
-0.885807421831909));
#44991=CARTESIAN_POINT('Ctrl Pts',(-0.117729028952017,0.000106365187095494,
-0.885086711473621));
#44992=CARTESIAN_POINT('Ctrl Pts',(-0.117699425459372,0.000101537840546503,
-0.925213288526387));
#44993=CARTESIAN_POINT('Ctrl Pts',(-0.117473768977369,-0.0274239955520595,
-0.923355928719752));
#44994=CARTESIAN_POINT('Ctrl Pts',(-0.0941091841536456,-0.0945534961756978,
-0.918849471810467));
#44995=CARTESIAN_POINT('Ctrl Pts',(0.017789693141843,-0.1381153157854,-0.911693917798532));
#44996=CARTESIAN_POINT('Ctrl Pts',(0.125753353137608,-0.0598197944766599,
-0.90374662649058));
#44997=CARTESIAN_POINT('Ctrl Pts',(0.118377915156088,0.0733415492056153,
-0.895799335182628));
#44998=CARTESIAN_POINT('Ctrl Pts',(0.00242802079729554,0.139235118959227,
-0.887852043874677));
#44999=CARTESIAN_POINT('Ctrl Pts',(-0.0996106832345008,0.0858651502554784,
-0.880990028322597));
#45000=CARTESIAN_POINT('Ctrl Pts',(-0.117507148798398,0.0231655611783769,
-0.876777109873167));
#45001=CARTESIAN_POINT('Ctrl Pts',(-0.117606504447261,-5.58891152924006E-5,
-0.875213288526387));
#45002=CARTESIAN_POINT('Origin',(0.,0.,-3.06008671147362));
#45003=CARTESIAN_POINT('',(-0.117686879986589,-9.84958757579055E-5,-0.985086711473621));
#45004=CARTESIAN_POINT('',(-0.117968676352971,5.43384420481955E-6,-0.975213288526387));
#45005=CARTESIAN_POINT('',(-0.117775,1.13296574333067E-13,-3.06008671147362));
#45006=CARTESIAN_POINT('Ctrl Pts',(-0.117686879986589,-9.84958757579094E-5,
-0.985086711473621));
#45007=CARTESIAN_POINT('Ctrl Pts',(-0.117783191571813,-0.0123051889181925,
-0.984263253730382));
#45008=CARTESIAN_POINT('Ctrl Pts',(-0.11041493107276,-0.0636679012646631,
-0.980790698884494));
#45009=CARTESIAN_POINT('Ctrl Pts',(-0.0360253121667897,-0.134515764143485,
-0.974669046935953));
#45010=CARTESIAN_POINT('Ctrl Pts',(0.0935911472513838,-0.103116492744809,
-0.966721755628004));
#45011=CARTESIAN_POINT('Ctrl Pts',(0.13736720374351,0.0228596862513367,
-0.958774464320049));
#45012=CARTESIAN_POINT('Ctrl Pts',(0.0551521118795285,0.127869302317047,
-0.950827173012101));
#45013=CARTESIAN_POINT('Ctrl Pts',(-0.0767892156275477,0.115678421683065,
-0.942931255396621));
#45014=CARTESIAN_POINT('Ctrl Pts',(-0.117902032884089,0.038257879003206,
-0.937684434883797));
#45015=CARTESIAN_POINT('Ctrl Pts',(-0.117966893777284,-1.41613286548282E-5,
-0.935086711473621));
#45016=CARTESIAN_POINT('Ctrl Pts',(-0.117968676352971,5.43384420481787E-6,
-0.975213288526387));
#45017=CARTESIAN_POINT('Ctrl Pts',(-0.117942707376789,-0.0387323630877177,
-0.972583844668988));
#45018=CARTESIAN_POINT('Ctrl Pts',(-0.07593103584133,-0.116545765660636,
-0.967305303708942));
#45019=CARTESIAN_POINT('Ctrl Pts',(0.0566772345635106,-0.127200647477969,
-0.959377665646241));
#45020=CARTESIAN_POINT('Ctrl Pts',(0.137630738076998,-0.0212154088568283,
-0.95143037433829));
#45021=CARTESIAN_POINT('Ctrl Pts',(0.0923513834783183,0.104228286017869,
-0.943483083030339));
#45022=CARTESIAN_POINT('Ctrl Pts',(-0.0376312812236582,0.13407535310432,
-0.935535791722386));
#45023=CARTESIAN_POINT('Ctrl Pts',(-0.110787333250892,0.0627146963454166,
-0.92944586022107));
#45024=CARTESIAN_POINT('Ctrl Pts',(-0.117795616112498,0.011834854832662,
-0.926005025822403));
#45025=CARTESIAN_POINT('Ctrl Pts',(-0.117699425459372,0.000101537840546503,
-0.925213288526387));
#45026=CARTESIAN_POINT('Origin',(0.,0.,-3.06008671147362));
#45027=CARTESIAN_POINT('',(-0.117613627014458,6.24323588500954E-5,-1.03508671147362));
#45028=CARTESIAN_POINT('',(-0.11771557645994,-0.000104556441113679,-1.02521328852639));
#45029=CARTESIAN_POINT('',(-0.117775,1.13296574333067E-13,-3.06008671147362));
#45030=CARTESIAN_POINT('Ctrl Pts',(-0.117613627014458,6.24323588500949E-5,
-1.03508671147362));
#45031=CARTESIAN_POINT('Ctrl Pts',(-0.117499984628548,-0.0236264518139759,
-1.03349116967962));
#45032=CARTESIAN_POINT('Ctrl Pts',(-0.0990513846795703,-0.0868091095822184,
-1.02924653078297));
#45033=CARTESIAN_POINT('Ctrl Pts',(0.00409282660561049,-0.13919613029893,
-1.02235279478367));
#45034=CARTESIAN_POINT('Ctrl Pts',(0.119246473329177,-0.0719207377490957,
-1.01440550347571));
#45035=CARTESIAN_POINT('Ctrl Pts',(0.12502903508685,0.0613192816744626,
-1.00645821216776));
#45036=CARTESIAN_POINT('Ctrl Pts',(0.0161368325691865,0.138318171454277,
-0.998510920859808));
#45037=CARTESIAN_POINT('Ctrl Pts',(-0.0947394295923312,0.0936204014483265,
-0.991387087295095));
#45038=CARTESIAN_POINT('Ctrl Pts',(-0.117473353279,0.0269642398256485,-0.986912350833033));
#45039=CARTESIAN_POINT('Ctrl Pts',(-0.117686879986589,-9.84958757579094E-5,
-0.985086711473621));
#45040=CARTESIAN_POINT('Ctrl Pts',(-0.11771557645994,-0.000104556441113676,
-1.02521328852639));
#45041=CARTESIAN_POINT('Ctrl Pts',(-0.117810672883519,-0.011251489233664,
-1.02446085772088));
#45042=CARTESIAN_POINT('Ctrl Pts',(-0.111239157541274,-0.0615337344264252,
-1.02105932981271));
#45043=CARTESIAN_POINT('Ctrl Pts',(-0.0396138321773288,-0.133503025946263,
-1.0150087048019));
#45044=CARTESIAN_POINT('Ctrl Pts',(0.0907968256135503,-0.105585274044654,
-1.00706141349395));
#45045=CARTESIAN_POINT('Ctrl Pts',(0.137929990564865,0.0191737148032896,
-0.999114122186));
#45046=CARTESIAN_POINT('Ctrl Pts',(0.0585558274900352,0.126346858700717,
-0.991166830878047));
#45047=CARTESIAN_POINT('Ctrl Pts',(-0.0745248663094564,0.117636550179523,
-0.983219539570098));
#45048=CARTESIAN_POINT('Ctrl Pts',(-0.117836667080937,0.0396116618043791,
-0.977901692119542));
#45049=CARTESIAN_POINT('Ctrl Pts',(-0.11796887045282,0.000294971657115395,
-0.975232941771639));
#45050=CARTESIAN_POINT('Ctrl Pts',(-0.117968676352971,5.43384420481787E-6,
-0.975213288526387));
#45051=CARTESIAN_POINT('Origin',(0.,0.,-3.06008671147362));
#45052=CARTESIAN_POINT('',(-0.117915488935345,7.05844075192093E-5,-1.08508671147362));
#45053=CARTESIAN_POINT('',(-0.117598824873155,4.73937789327097E-5,-1.07521328852639));
#45054=CARTESIAN_POINT('',(-0.117775,1.13296574333067E-13,-3.06008671147362));
#45055=CARTESIAN_POINT('Ctrl Pts',(-0.117915488935345,7.05844075192083E-5,
-1.08508671147362));
#45056=CARTESIAN_POINT('Ctrl Pts',(-0.117668354362795,-0.0348517922405095,
-1.08271908562885));
#45057=CARTESIAN_POINT('Ctrl Pts',(-0.0827226944694583,-0.109277798319543,
-1.07770236268144));
#45058=CARTESIAN_POINT('Ctrl Pts',(0.043866657927493,-0.132166675989422,
-1.07003654263137));
#45059=CARTESIAN_POINT('Ctrl Pts',(0.134870236095805,-0.0346746785894572,
-1.06208925132342));
#45060=CARTESIAN_POINT('Ctrl Pts',(0.102172847354302,0.0946204163134727,
-1.05414196001547));
#45061=CARTESIAN_POINT('Ctrl Pts',(-0.0242359515212969,0.137131078073783,
-1.04619466870752));
#45062=CARTESIAN_POINT('Ctrl Pts',(-0.107500160123668,0.0705836828280244,
-1.03984291919357));
#45063=CARTESIAN_POINT('Ctrl Pts',(-0.11768866643957,0.0157044855912191,
-1.03614026678227));
#45064=CARTESIAN_POINT('Ctrl Pts',(-0.117613627014458,6.24323588500949E-5,
-1.03508671147362));
#45065=CARTESIAN_POINT('Ctrl Pts',(-0.117598824873155,4.73937789327028E-5,
-1.07521328852639));
#45066=CARTESIAN_POINT('Ctrl Pts',(-0.117516998884501,-0.0225940828510371,
-1.07368877367011));
#45067=CARTESIAN_POINT('Ctrl Pts',(-0.100292170955009,-0.0846940636737381,
-1.06951516171119));
#45068=CARTESIAN_POINT('Ctrl Pts',(0.00036461620057585,-0.139255810261576,
-1.06269245264961));
#45069=CARTESIAN_POINT('Ctrl Pts',(0.117278168930411,-0.0750875803905805,
-1.05474516134166));
#45070=CARTESIAN_POINT('Ctrl Pts',(0.126625936101752,0.0579498571433683,
-1.04679787003371));
#45071=CARTESIAN_POINT('Ctrl Pts',(0.0198342852289171,0.137836550907369,
-1.03885057872576));
#45072=CARTESIAN_POINT('Ctrl Pts',(-0.0933159459371162,0.0957074358369753,
-1.03165571822332));
#45073=CARTESIAN_POINT('Ctrl Pts',(-0.117475865139962,0.0279937239446263,
-1.02710995482353));
#45074=CARTESIAN_POINT('Ctrl Pts',(-0.11771557645994,-0.000104556441113676,
-1.02521328852639));
#45075=CARTESIAN_POINT('Origin',(0.,0.,-3.06008671147362));
#45076=CARTESIAN_POINT('',(-0.117831609157221,-0.000101687419266419,-1.13508671147362));
#45077=CARTESIAN_POINT('',(-0.117889553338148,8.37928209511622E-5,-1.12521328852639));
#45078=CARTESIAN_POINT('',(-0.117775,1.13296574333067E-13,-3.06008671147362));
#45079=CARTESIAN_POINT('Ctrl Pts',(-0.117831609157221,-0.000101687419266441,
-1.13508671147362));
#45080=CARTESIAN_POINT('Ctrl Pts',(-0.117897702251559,-0.00735161785805869,
-1.13459609868074));
#45081=CARTESIAN_POINT('Ctrl Pts',(-0.113984098036961,-0.053676869687243,
-1.13145638878521));
#45082=CARTESIAN_POINT('Ctrl Pts',(-0.0525767967102828,-0.128949580718614,
-1.12566758178704));
#45083=CARTESIAN_POINT('Ctrl Pts',(0.0799502236678128,-0.114018751331906,
-1.11772029047908));
#45084=CARTESIAN_POINT('Ctrl Pts',(0.13914809256923,0.00548837445564355,
-1.10977299917113));
#45085=CARTESIAN_POINT('Ctrl Pts',(0.0707214084725853,0.11996164513491,
-1.10182570786318));
#45086=CARTESIAN_POINT('Ctrl Pts',(-0.0625698955915714,0.124407885945709,
-1.09387841655523));
#45087=CARTESIAN_POINT('Ctrl Pts',(-0.115860262917991,0.0474181950354391,
-1.08829875109204));
#45088=CARTESIAN_POINT('Ctrl Pts',(-0.117944869117673,0.00422227303062001,
-1.08536818273151));
#45089=CARTESIAN_POINT('Ctrl Pts',(-0.117915488935345,7.05844075192083E-5,
-1.08508671147362));
#45090=CARTESIAN_POINT('Ctrl Pts',(-0.117889553338148,8.37928209511596E-5,
-1.12521328852639));
#45091=CARTESIAN_POINT('Ctrl Pts',(-0.117616609082175,-0.0338104601163673,
-1.12291668961935));
#45092=CARTESIAN_POINT('Ctrl Pts',(-0.0844519668986341,-0.107267264374004,
-1.11797099360966));
#45093=CARTESIAN_POINT('Ctrl Pts',(0.0403123913820496,-0.13329375355823,
-1.11037620049732));
#45094=CARTESIAN_POINT('Ctrl Pts',(0.133893531780113,-0.0382731731638424,
-1.10242890918937));
#45095=CARTESIAN_POINT('Ctrl Pts',(0.10466952388434,0.0918509902309573,
-1.09448161788142));
#45096=CARTESIAN_POINT('Ctrl Pts',(-0.0205558085830443,0.137730796737981,
-1.08653432657347));
#45097=CARTESIAN_POINT('Ctrl Pts',(-0.106522535859557,0.0727175613247637,
-1.08011155012179));
#45098=CARTESIAN_POINT('Ctrl Pts',(-0.117659185094477,0.0167492334133705,
-1.07633787077276));
#45099=CARTESIAN_POINT('Ctrl Pts',(-0.117598824873155,4.73937789327028E-5,
-1.07521328852639));
#45100=CARTESIAN_POINT('Origin',(0.,0.,-3.06008671147362));
#45101=CARTESIAN_POINT('',(-0.117582462475556,-1.51080851551548E-5,-1.18508671147362));
#45102=CARTESIAN_POINT('',(-0.117862347076416,-9.38393982804209E-5,-1.17521328852639));
#45103=CARTESIAN_POINT('',(-0.117775,1.13296574333067E-13,-3.06008671147362));
#45104=CARTESIAN_POINT('Ctrl Pts',(-0.117582462475556,-1.51080851551744E-5,
-1.18508671147362));
#45105=CARTESIAN_POINT('Ctrl Pts',(-0.117603898091645,-0.0187746844758571,
-1.18382401462998));
#45106=CARTESIAN_POINT('Ctrl Pts',(-0.104512501002388,-0.0768629882428656,
-1.17991222068369));
#45107=CARTESIAN_POINT('Ctrl Pts',(-0.0133598268380069,-0.138613956536415,
-1.17335132963475));
#45108=CARTESIAN_POINT('Ctrl Pts',(0.10930800785607,-0.0862790434483248,
-1.16540403832679));
#45109=CARTESIAN_POINT('Ctrl Pts',(0.131720169733078,0.0451897201286931,
-1.15745674701884));
#45110=CARTESIAN_POINT('Ctrl Pts',(0.0333205585370974,0.135211147094447,
-1.14950945571089));
#45111=CARTESIAN_POINT('Ctrl Pts',(-0.0876789955812038,0.103317381663382,
-1.14205277719582));
#45112=CARTESIAN_POINT('Ctrl Pts',(-0.117540828098952,0.0317948740366197,
-1.13724519578339));
#45113=CARTESIAN_POINT('Ctrl Pts',(-0.117831609157221,-0.000101687419266441,
-1.13508671147362));
#45114=CARTESIAN_POINT('Ctrl Pts',(-0.117862347076416,-9.38393982804252E-5,
-1.17521328852639));
#45115=CARTESIAN_POINT('Ctrl Pts',(-0.1179162650566,-0.00628999992156921,
-1.17479370267124));
#45116=CARTESIAN_POINT('Ctrl Pts',(-0.114651893565344,-0.0515493094812837,
-1.17172501971343));
#45117=CARTESIAN_POINT('Ctrl Pts',(-0.0560103581567255,-0.127495699597034,
-1.16600723965299));
#45118=CARTESIAN_POINT('Ctrl Pts',(0.0768689022763401,-0.116118411543615,
-1.15805994834503));
#45119=CARTESIAN_POINT('Ctrl Pts',(0.139245153208294,0.00176094990851802,
-1.15011265703708));
#45120=CARTESIAN_POINT('Ctrl Pts',(0.0739078285731691,0.118025194395861,
-1.14216536572913));
#45121=CARTESIAN_POINT('Ctrl Pts',(-0.0592166529718895,0.126038492721028,
-1.13421807442118));
#45122=CARTESIAN_POINT('Ctrl Pts',(-0.11525354823914,0.0495416262248971,
-1.12856738202026));
#45123=CARTESIAN_POINT('Ctrl Pts',(-0.117931446747328,0.00528612178028246,
-1.125565786722));
#45124=CARTESIAN_POINT('Ctrl Pts',(-0.117889553338148,8.37928209511596E-5,
-1.12521328852639));
#45125=CARTESIAN_POINT('Origin',(0.,0.,-3.06008671147362));
#45126=CARTESIAN_POINT('',(-0.117776021319591,0.000108156687832219,-1.23508671147362));
#45127=CARTESIAN_POINT('',(-0.117588764972749,-3.20871466719039E-5,-1.22521328852639));
#45128=CARTESIAN_POINT('',(-0.117775,1.13296574333067E-13,-3.06008671147362));
#45129=CARTESIAN_POINT('Ctrl Pts',(-0.117776021319591,0.000108156687832213,
-1.23508671147362));
#45130=CARTESIAN_POINT('Ctrl Pts',(-0.117498350433057,-0.0299968654539389,
-1.23305193057921));
#45131=CARTESIAN_POINT('Ctrl Pts',(-0.0904196508311549,-0.0997397256260159,
-1.22836805258216));
#45132=CARTESIAN_POINT('Ctrl Pts',(0.0269810332845223,-0.136617487031199,
-1.22103507748245));
#45133=CARTESIAN_POINT('Ctrl Pts',(0.12947029828579,-0.0512811445036981,
-1.2130877861745));
#45134=CARTESIAN_POINT('Ctrl Pts',(0.113211338714528,0.0810894981257437,
-1.20514049486655));
#45135=CARTESIAN_POINT('Ctrl Pts',(-0.00688337045973726,0.139086063755268,
-1.1971932035586));
#45136=CARTESIAN_POINT('Ctrl Pts',(-0.102586721940106,0.0805686970688501,
-1.19050860909429));
#45137=CARTESIAN_POINT('Ctrl Pts',(-0.117558926862991,0.0205822995174214,
-1.18647311173263));
#45138=CARTESIAN_POINT('Ctrl Pts',(-0.117582462475556,-1.51080851551744E-5,
-1.18508671147362));
#45139=CARTESIAN_POINT('Ctrl Pts',(-0.117588764972749,-3.20871466718952E-5,
-1.22521328852639));
#45140=CARTESIAN_POINT('Ctrl Pts',(-0.117631858824093,-0.0177340663052872,
-1.22402161862047));
#45141=CARTESIAN_POINT('Ctrl Pts',(-0.10556436402768,-0.0747319718305033,
-1.22018085161191));
#45142=CARTESIAN_POINT('Ctrl Pts',(-0.01706619414058,-0.138206579634031,
-1.21369098750069));
#45143=CARTESIAN_POINT('Ctrl Pts',(0.106958846585331,-0.0891746532021148,
-1.20574369619274));
#45144=CARTESIAN_POINT('Ctrl Pts',(0.132882830138289,0.0416469337529245,
-1.19779640488479));
#45145=CARTESIAN_POINT('Ctrl Pts',(0.036928665853329,0.134270574866107,
-1.18984911357684));
#45146=CARTESIAN_POINT('Ctrl Pts',(-0.0860416897627608,0.105354972619519,
-1.18232140812404));
#45147=CARTESIAN_POINT('Ctrl Pts',(-0.117575848516499,0.0328300769073127,
-1.17744279977389));
#45148=CARTESIAN_POINT('Ctrl Pts',(-0.117862347076416,-9.38393982804252E-5,
-1.17521328852639));
#45149=CARTESIAN_POINT('Origin',(0.,0.,-3.06008671147362));
#45150=CARTESIAN_POINT('',(-0.117950597231983,-4.22694188566558E-5,-1.28508671147362));
#45151=CARTESIAN_POINT('',(-0.117744385826804,0.000107701528469582,-1.27521328852639));
#45152=CARTESIAN_POINT('',(-0.117775,1.13296574333067E-13,-3.06008671147362));
#45153=CARTESIAN_POINT('Ctrl Pts',(-0.117950597231983,-4.22694188566583E-5,
-1.28508671147362));
#45154=CARTESIAN_POINT('Ctrl Pts',(-0.117961342406869,-0.00236750816820977,
-1.2849289436311));
#45155=CARTESIAN_POINT('Ctrl Pts',(-0.116844235725132,-0.0437255601152145,
-1.28212207868593));
#45156=CARTESIAN_POINT('Ctrl Pts',(-0.0683015385030549,-0.121355732282971,
-1.27666611663811));
#45157=CARTESIAN_POINT('Ctrl Pts',(0.0650521244483742,-0.123128124425631,
-1.26871882533016));
#45158=CARTESIAN_POINT('Ctrl Pts',(0.138740950095853,-0.0119692391704875,
-1.26077153402221));
#45159=CARTESIAN_POINT('Ctrl Pts',(0.0851786477431396,0.110167653548901,
-1.25282424271426));
#45160=CARTESIAN_POINT('Ctrl Pts',(-0.0465082385868169,0.131260419256424,
-1.24487695140631));
#45161=CARTESIAN_POINT('Ctrl Pts',(-0.112743652358229,0.0573866324060485,
-1.23896444099276));
#45162=CARTESIAN_POINT('Ctrl Pts',(-0.117859852324013,0.00919709746870165,
-1.23570102768187));
#45163=CARTESIAN_POINT('Ctrl Pts',(-0.117776021319591,0.000108156687832213,
-1.23508671147362));
#45164=CARTESIAN_POINT('Ctrl Pts',(-0.117744385826804,0.000107701528469589,
-1.27521328852639));
#45165=CARTESIAN_POINT('Ctrl Pts',(-0.117483723357635,-0.0289663776992756,
-1.27324953456971));
#45166=CARTESIAN_POINT('Ctrl Pts',(-0.0919304336464584,-0.0976706501736823,
-1.26863668351038));
#45167=CARTESIAN_POINT('Ctrl Pts',(0.0233136568373885,-0.137290884771896,
-1.2613747353484));
#45168=CARTESIAN_POINT('Ctrl Pts',(0.128050919416408,-0.0547291117522856,
-1.25342744404045));
#45169=CARTESIAN_POINT('Ctrl Pts',(0.115341790530312,0.0780293854508893,
-1.2454801527325));
#45170=CARTESIAN_POINT('Ctrl Pts',(-0.003157106556191,0.139220495311483,
-1.23753286142455));
#45171=CARTESIAN_POINT('Ctrl Pts',(-0.101426030289338,0.0826920768249464,
-1.23077724002251));
#45172=CARTESIAN_POINT('Ctrl Pts',(-0.117536060653668,0.0216176547271468,
-1.22667071572312));
#45173=CARTESIAN_POINT('Ctrl Pts',(-0.117588764972749,-3.20871466718952E-5,
-1.22521328852639));
#45174=CARTESIAN_POINT('Origin',(0.,0.,-3.06008671147362));
#45175=CARTESIAN_POINT('',(-0.117648697715254,-8.46313478923296E-5,-1.33508671147362));
#45176=CARTESIAN_POINT('',(-0.117963151496065,-2.37579109470393E-5,-1.32521328852639));
#45177=CARTESIAN_POINT('',(-0.117775,1.13296574333067E-13,-3.06008671147362));
#45178=CARTESIAN_POINT('Ctrl Pts',(-0.117648697715254,-8.46313478923295E-5,
-1.33508671147362));
#45179=CARTESIAN_POINT('Ctrl Pts',(-0.11774013592033,-0.0138797514576444,
-1.33415685958034));
#45180=CARTESIAN_POINT('Ctrl Pts',(-0.109114338455593,-0.0668657107954565,
-1.33057791058441));
#45181=CARTESIAN_POINT('Ctrl Pts',(-0.0306024039612664,-0.135852150485784,
-1.32434986448582));
#45182=CARTESIAN_POINT('Ctrl Pts',(0.097650730877784,-0.0992806561161591,
-1.31640257317787));
#45183=CARTESIAN_POINT('Ctrl Pts',(0.136340073298976,0.0283495737648783,
-1.30845528186992));
#45184=CARTESIAN_POINT('Ctrl Pts',(0.0499803360725424,0.129977997853083,
-1.30050799056197));
#45185=CARTESIAN_POINT('Ctrl Pts',(-0.0795961955054469,0.112741645408569,
-1.29271846709654));
#45186=CARTESIAN_POINT('Ctrl Pts',(-0.117780918999896,0.036675830040556,
-1.28757804073375));
#45187=CARTESIAN_POINT('Ctrl Pts',(-0.117950597231983,-4.22694188566583E-5,
-1.28508671147362));
#45188=CARTESIAN_POINT('Ctrl Pts',(-0.117963151496065,-2.3757910947049E-5,
-1.32521328852639));
#45189=CARTESIAN_POINT('Ctrl Pts',(-0.11796667100053,-0.00130181316577145,
-1.32512654762159));
#45190=CARTESIAN_POINT('Ctrl Pts',(-0.117368372503623,-0.0416087406635258,
-1.32239070961415));
#45191=CARTESIAN_POINT('Ctrl Pts',(-0.0715261504195623,-0.119483569760616,
-1.31700577450407));
#45192=CARTESIAN_POINT('Ctrl Pts',(0.0617322554776575,-0.124825647485695,
-1.30905848319611));
#45193=CARTESIAN_POINT('Ctrl Pts',(0.138370758324617,-0.0156795050066074,
-1.30111119188816));
#45194=CARTESIAN_POINT('Ctrl Pts',(0.0880976675369301,0.107847645366666,
-1.29316390058021));
#45195=CARTESIAN_POINT('Ctrl Pts',(-0.0429772886013641,0.132458545594676,
-1.28521660927226));
#45196=CARTESIAN_POINT('Ctrl Pts',(-0.111985965485845,0.0595187591475933,
-1.27923307192098));
#45197=CARTESIAN_POINT('Ctrl Pts',(-0.11783535610139,0.0102544517649053,
-1.27589863167236));
#45198=CARTESIAN_POINT('Ctrl Pts',(-0.117744385826804,0.000107701528469589,
-1.27521328852639));
#45199=CARTESIAN_POINT('Origin',(0.,0.,-3.06008671147362));
#45200=CARTESIAN_POINT('',(-0.117643137731857,8.18848197860175E-5,-1.38508671147362));
#45201=CARTESIAN_POINT('',(-0.117673475788507,-9.44926190546702E-5,-1.37521328852639));
#45202=CARTESIAN_POINT('',(-0.117775,1.13296574333067E-13,-3.06008671147362));
#45203=CARTESIAN_POINT('Ctrl Pts',(-0.117643137731858,8.18848197859986E-5,
-1.38508671147362));
#45204=CARTESIAN_POINT('Ctrl Pts',(-0.117481692417359,-0.0251707373262468,
-1.38338477552957));
#45205=CARTESIAN_POINT('Ctrl Pts',(-0.0971137812511854,-0.0899671114874316,
-1.37903374248288));
#45206=CARTESIAN_POINT('Ctrl Pts',(0.00967114594259312,-0.13892005922824,
-1.37203361233354));
#45207=CARTESIAN_POINT('Ctrl Pts',(0.122034507452407,-0.0670812411234985,
-1.36408632102558));
#45208=CARTESIAN_POINT('Ctrl Pts',(0.122469640724355,0.0662834898045348,
-1.35613902971763));
#45209=CARTESIAN_POINT('Ctrl Pts',(0.0105774480180276,0.138853993508456,
-1.34819173840968));
#45210=CARTESIAN_POINT('Ctrl Pts',(-0.0967894748877886,0.0904795809546536,
-1.34117429899501));
#45211=CARTESIAN_POINT('Ctrl Pts',(-0.11747963348345,0.0254217899787136,
-1.33680595668299));
#45212=CARTESIAN_POINT('Ctrl Pts',(-0.117648697715254,-8.46313478923295E-5,
-1.33508671147362));
#45213=CARTESIAN_POINT('Ctrl Pts',(-0.117673475788507,-9.44926190546719E-5,
-1.37521328852639));
#45214=CARTESIAN_POINT('Ctrl Pts',(-0.117769086788655,-0.0128291175224179,
-1.37435446357083));
#45215=CARTESIAN_POINT('Ctrl Pts',(-0.109991446578368,-0.0647308244202197,
-1.37084654151263));
#45216=CARTESIAN_POINT('Ctrl Pts',(-0.0342286474655051,-0.134984122508034,
-1.36468952235177));
#45217=CARTESIAN_POINT('Ctrl Pts',(0.0949576520728147,-0.10185950102666,
-1.35674223104382));
#45218=CARTESIAN_POINT('Ctrl Pts',(0.137050210865036,0.0246891340154153,
-1.34879493973587));
#45219=CARTESIAN_POINT('Ctrl Pts',(0.0534423624365219,0.12859326395183,
-1.34084764842792));
#45220=CARTESIAN_POINT('Ctrl Pts',(-0.0777344908263304,0.114706808671506,
-1.33298709802476));
#45221=CARTESIAN_POINT('Ctrl Pts',(-0.117859184122194,0.0377304344315316,
-1.32777564472425));
#45222=CARTESIAN_POINT('Ctrl Pts',(-0.117963151496065,-2.3757910947049E-5,
-1.32521328852639));
#45223=CARTESIAN_POINT('Origin',(0.,0.,-3.06008671147362));
#45224=CARTESIAN_POINT('',(-0.117946614788854,4.6571822748169E-5,-1.43508671147362));
#45225=CARTESIAN_POINT('',(-0.117622503294115,6.93536635249722E-5,-1.42521328852639));
#45226=CARTESIAN_POINT('',(-0.117775,1.13296574333067E-13,-3.06008671147362));
#45227=CARTESIAN_POINT('Ctrl Pts',(-0.117946614788854,4.65718227481639E-5,
-1.43508671147362));
#45228=CARTESIAN_POINT('Ctrl Pts',(-0.11776338497764,-0.0364196896702833,
-1.43261269147881));
#45229=CARTESIAN_POINT('Ctrl Pts',(-0.0800425056981712,-0.112260027951507,
-1.42748957438135));
#45230=CARTESIAN_POINT('Ctrl Pts',(0.0491311144456285,-0.130301371877472,
-1.41971736018124));
#45231=CARTESIAN_POINT('Ctrl Pts',(0.136152178426768,-0.0292386427432272,
-1.41177006887329));
#45232=CARTESIAN_POINT('Ctrl Pts',(0.0982964971317635,0.0986413329768289,
-1.40382277756534));
#45233=CARTESIAN_POINT('Ctrl Pts',(-0.0297152637478395,0.136048950823653,
-1.39587548625739));
#45234=CARTESIAN_POINT('Ctrl Pts',(-0.108895140667733,0.0673859988607212,
-1.38963013089348));
#45235=CARTESIAN_POINT('Ctrl Pts',(-0.117732985256182,0.014135470639733,
-1.38603387263222));
#45236=CARTESIAN_POINT('Ctrl Pts',(-0.117643137731858,8.18848197859986E-5,
-1.38508671147362));
#45237=CARTESIAN_POINT('Ctrl Pts',(-0.117622503294115,6.9353663524974E-5,
-1.42521328852639));
#45238=CARTESIAN_POINT('Ctrl Pts',(-0.117492881168235,-0.0241400490349439,
-1.42358237952007));
#45239=CARTESIAN_POINT('Ctrl Pts',(-0.0984178786166064,-0.0878603341406336,
-1.4193023734111));
#45240=CARTESIAN_POINT('Ctrl Pts',(0.0059483271787393,-0.139129188312001,
-1.41237327019948));
#45241=CARTESIAN_POINT('Ctrl Pts',(0.120194773022965,-0.0703244635567145,
-1.40442597889153));
#45242=CARTESIAN_POINT('Ctrl Pts',(0.12420036758044,0.0629808092157078,
-1.39647868758358));
#45243=CARTESIAN_POINT('Ctrl Pts',(0.0142912393273046,0.138521024090466,
-1.38853139627563));
#45244=CARTESIAN_POINT('Ctrl Pts',(-0.0954317712490366,0.0925781715067274,
-1.38144292992323));
#45245=CARTESIAN_POINT('Ctrl Pts',(-0.117474168922288,0.0264515970361115,
-1.37700356067348));
#45246=CARTESIAN_POINT('Ctrl Pts',(-0.117673475788507,-9.44926190546719E-5,
-1.37521328852639));
#45247=CARTESIAN_POINT('Origin',(0.,0.,-3.06008671147362));
#45248=CARTESIAN_POINT('',(-0.117783823687606,-0.000107808840122532,-1.48508671147362));
#45249=CARTESIAN_POINT('',(-0.11792699295135,6.31151991691888E-5,-1.47521328852639));
#45250=CARTESIAN_POINT('',(-0.117775,1.13296574333067E-13,-3.06008671147362));
#45251=CARTESIAN_POINT('Ctrl Pts',(-0.117783823687606,-0.000107808840122531,
-1.48508671147362));
#45252=CARTESIAN_POINT('Ctrl Pts',(-0.117865535679874,-0.00893915841207697,
-1.4844897045307));
#45253=CARTESIAN_POINT('Ctrl Pts',(-0.112923229129106,-0.0568672450942766,
-1.48124360048513));
#45254=CARTESIAN_POINT('Ctrl Pts',(-0.0473637742173777,-0.130954140109069,
-1.47534839933691));
#45255=CARTESIAN_POINT('Ctrl Pts',(0.0844579470046824,-0.110721132163533,
-1.46740110802895));
#45256=CARTESIAN_POINT('Ctrl Pts',(0.138816100206623,0.0110636451156712,
-1.459453816721));
#45257=CARTESIAN_POINT('Ctrl Pts',(0.0658541988487744,0.122701012277025,
-1.45150652541305));
#45258=CARTESIAN_POINT('Ctrl Pts',(-0.0675081904779539,0.121798842926412,
-1.4435592341051));
#45259=CARTESIAN_POINT('Ctrl Pts',(-0.116712029120029,0.0442418089731312,
-1.43808596279196));
#45260=CARTESIAN_POINT('Ctrl Pts',(-0.11795958127477,0.00262715225840995,
-1.43526178858146));
#45261=CARTESIAN_POINT('Ctrl Pts',(-0.117946614788854,4.65718227481639E-5,
-1.43508671147362));
#45262=CARTESIAN_POINT('Ctrl Pts',(-0.11792699295135,6.3115199169191E-5,
-1.47521328852638));
#45263=CARTESIAN_POINT('Ctrl Pts',(-0.11769755575331,-0.0353718248083651,
-1.4728102954693));
#45264=CARTESIAN_POINT('Ctrl Pts',(-0.0818437614380234,-0.110273199218807,
-1.46775820530957));
#45265=CARTESIAN_POINT('Ctrl Pts',(0.045624901106524,-0.131570065119699,
-1.46005701804719));
#45266=CARTESIAN_POINT('Ctrl Pts',(0.135320555318067,-0.0328734078700636,
-1.45210972673924));
#45267=CARTESIAN_POINT('Ctrl Pts',(0.100902216552484,0.0959742482720097,
-1.44416243543129));
#45268=CARTESIAN_POINT('Ctrl Pts',(-0.0260621287465163,0.13679575681205,
-1.43621514412334));
#45269=CARTESIAN_POINT('Ctrl Pts',(-0.107973035031269,0.0695208292702655,
-1.4298987618217));
#45270=CARTESIAN_POINT('Ctrl Pts',(-0.117703427309545,0.0151834560147021,
-1.42623147662272));
#45271=CARTESIAN_POINT('Ctrl Pts',(-0.117622503294115,6.9353663524974E-5,
-1.42521328852639));
#45272=CARTESIAN_POINT('Origin',(0.,0.,-3.06008671147362));
#45273=CARTESIAN_POINT('',(-0.117581619011794,1.08966417829141E-5,-1.53508671147362));
#45274=CARTESIAN_POINT('',(-0.117815844487591,-0.000104481014402413,-1.52521328852638));
#45275=CARTESIAN_POINT('',(-0.117775,1.13296574333067E-13,-3.06008671147362));
#45276=CARTESIAN_POINT('Ctrl Pts',(-0.117581619011794,1.089664178292E-5,
-1.53508671147362));
#45277=CARTESIAN_POINT('Ctrl Pts',(-0.117564862655435,-0.0203297153006686,
-1.53371762047993));
#45278=CARTESIAN_POINT('Ctrl Pts',(-0.102863457479005,-0.0800507033264646,
-1.5296994323836));
#45279=CARTESIAN_POINT('Ctrl Pts',(-0.00779081513336725,-0.139038185831728,
-1.52303214718461));
#45280=CARTESIAN_POINT('Ctrl Pts',(0.112679787534581,-0.0818265201568669,
-1.51508485587666));
#45281=CARTESIAN_POINT('Ctrl Pts',(0.129802171405619,0.0504352081209822,
-1.50713756456871));
#45282=CARTESIAN_POINT('Ctrl Pts',(0.0278719416335478,0.136438516517136,
-1.49919027326076));
#45283=CARTESIAN_POINT('Ctrl Pts',(-0.0900445677183776,0.100242387200107,
-1.49183998889573));
#45284=CARTESIAN_POINT('Ctrl Pts',(-0.117502955303656,0.0302481623401825,
-1.48713880163335));
#45285=CARTESIAN_POINT('Ctrl Pts',(-0.117783823687606,-0.000107808840122531,
-1.48508671147362));
#45286=CARTESIAN_POINT('Ctrl Pts',(-0.117815844487591,-0.000104481014402428,
-1.52521328852638));
#45287=CARTESIAN_POINT('Ctrl Pts',(-0.117887561503818,-0.00787972330702221,
-1.52468730852119));
#45288=CARTESIAN_POINT('Ctrl Pts',(-0.113639577894226,-0.054736975302814,
-1.52151223141335));
#45289=CARTESIAN_POINT('Ctrl Pts',(-0.0508528731324187,-0.129639110343907,
-1.51568805720286));
#45290=CARTESIAN_POINT('Ctrl Pts',(0.0814632979273637,-0.112942661237371,
-1.5077407658949));
#45291=CARTESIAN_POINT('Ctrl Pts',(0.139062548390083,0.0073431105015257,
-1.49979347458695));
#45292=CARTESIAN_POINT('Ctrl Pts',(0.0691157056986611,0.120893890922402,
-1.491846183279));
#45293=CARTESIAN_POINT('Ctrl Pts',(-0.0642230303494631,0.123562599557122,
-1.48389889197105));
#45294=CARTESIAN_POINT('Ctrl Pts',(-0.116150928522588,0.0463617126739875,
-1.47835459372018));
#45295=CARTESIAN_POINT('Ctrl Pts',(-0.117950490906318,0.00369220687078259,
-1.47545939257196));
#45296=CARTESIAN_POINT('Ctrl Pts',(-0.11792699295135,6.3115199169191E-5,
-1.47521328852638));
#45297=CARTESIAN_POINT('Origin',(0.,0.,-3.06008671147362));
#45298=CARTESIAN_POINT('',(-0.117823920457094,0.000103148469539977,-1.58508671147362));
#45299=CARTESIAN_POINT('',(-0.117581030135854,-6.48590087786588E-6,-1.57521328852638));
#45300=CARTESIAN_POINT('',(-0.117775,1.13296574333067E-13,-3.06008671147362));
#45301=CARTESIAN_POINT('Ctrl Pts',(-0.117823920457094,0.00010314846953997,
-1.58508671147362));
#45302=CARTESIAN_POINT('Ctrl Pts',(-0.117533506753675,-0.0315429534362953,
-1.58294553642917));
#45303=CARTESIAN_POINT('Ctrl Pts',(-0.0880709269273121,-0.102818908660365,
-1.57815526428207));
#45304=CARTESIAN_POINT('Ctrl Pts',(0.0324375432515528,-0.135425698106468,
-1.57071589503233));
#45305=CARTESIAN_POINT('Ctrl Pts',(0.131422484648456,-0.0460482838838423,
-1.56276860372437));
#45306=CARTESIAN_POINT('Ctrl Pts',(0.109868685287492,0.0855639288077546,
-1.55482131241642));
#45307=CARTESIAN_POINT('Ctrl Pts',(-0.0124550318596216,0.138698183481963,
-1.54687402110847));
#45308=CARTESIAN_POINT('Ctrl Pts',(-0.104250256091004,0.0773819952015474,
-1.5402958207942));
#45309=CARTESIAN_POINT('Ctrl Pts',(-0.117597285054886,0.0190279726919229,
-1.53636671758259));
#45310=CARTESIAN_POINT('Ctrl Pts',(-0.117581619011794,1.089664178292E-5,
-1.53508671147362));
#45311=CARTESIAN_POINT('Ctrl Pts',(-0.117581030135854,-6.48590087786935E-6,
-1.57521328852638));
#45312=CARTESIAN_POINT('Ctrl Pts',(-0.117590483811689,-0.0192920895595535,
-1.57391522447043));
#45313=CARTESIAN_POINT('Ctrl Pts',(-0.103974180293752,-0.0779232980843118,
-1.56996806331182));
#45314=CARTESIAN_POINT('Ctrl Pts',(-0.0115105368274101,-0.138779757812609,
-1.56337180505056));
#45315=CARTESIAN_POINT('Ctrl Pts',(0.110448626411003,-0.0848139997907445,
-1.55542451374261));
#45316=CARTESIAN_POINT('Ctrl Pts',(0.131105958523409,0.0469418925506857,
-1.54747722243466));
#45317=CARTESIAN_POINT('Ctrl Pts',(0.0315148629140466,0.135643381895656,
-1.53952993112671));
#45318=CARTESIAN_POINT('Ctrl Pts',(-0.0884768683350901,0.102298108392725,
-1.53210861982395));
#45319=CARTESIAN_POINT('Ctrl Pts',(-0.117526358914326,0.0312802668568986,
-1.52733640562384));
#45320=CARTESIAN_POINT('Ctrl Pts',(-0.117815844487591,-0.000104481014402428,
-1.52521328852638));
#45321=CARTESIAN_POINT('Origin',(0.,0.,-3.06008671147362));
#45322=CARTESIAN_POINT('',(-0.117921249980265,-6.69982741048494E-5,-1.63508671147362));
#45323=CARTESIAN_POINT('',(-0.117791976321323,0.000107252653627231,-1.62521328852638));
#45324=CARTESIAN_POINT('',(-0.117775,1.13296574333067E-13,-3.06008671147362));
#45325=CARTESIAN_POINT('Ctrl Pts',(-0.117921249980265,-6.69982741048542E-5,
-1.63508671147362));
#45326=CARTESIAN_POINT('Ctrl Pts',(-0.117947710639304,-0.00396287537901269,
-1.63482254948106));
#45327=CARTESIAN_POINT('Ctrl Pts',(-0.116003462933909,-0.0469010631975345,
-1.63190929038585));
#45328=CARTESIAN_POINT('Ctrl Pts',(-0.0633803737869685,-0.123996944068975,
-1.62634693418799));
#45329=CARTESIAN_POINT('Ctrl Pts',(0.0699371058934867,-0.120420576061834,
-1.61839964288003));
#45330=CARTESIAN_POINT('Ctrl Pts',(0.139109316222199,-0.00639625359196896,
-1.61045235157208));
#45331=CARTESIAN_POINT('Ctrl Pts',(0.0806925386394054,0.113494617175214,
-1.60250506026413));
#45332=CARTESIAN_POINT('Ctrl Pts',(-0.051734230629111,0.129289919564653,
-1.59455776895618));
#45333=CARTESIAN_POINT('Ctrl Pts',(-0.113816488971119,0.0541956459344663,
-1.58875165269268));
#45334=CARTESIAN_POINT('Ctrl Pts',(-0.117892811380493,0.00761012612454138,
-1.58559463353182));
#45335=CARTESIAN_POINT('Ctrl Pts',(-0.117823920457094,0.00010314846953997,
-1.58508671147362));
#45336=CARTESIAN_POINT('Ctrl Pts',(-0.117791976321323,0.000107252653627225,
-1.62521328852638));
#45337=CARTESIAN_POINT('Ctrl Pts',(-0.117508209392984,-0.0305104146554398,
-1.62314314041966));
#45338=CARTESIAN_POINT('Ctrl Pts',(-0.0896503593683097,-0.100766102680647,
-1.61842389521029));
#45339=CARTESIAN_POINT('Ctrl Pts',(0.0288001189230785,-0.136245611990252,
-1.61105555289827));
#45340=CARTESIAN_POINT('Ctrl Pts',(0.130142507042637,-0.0495503935124521,
-1.60310826159032));
#45341=CARTESIAN_POINT('Ctrl Pts',(0.112120130754087,0.0825917060985434,
-1.59516097028237));
#45342=CARTESIAN_POINT('Ctrl Pts',(-0.00873715548808248,0.138981925985211,
-1.58721367897442));
#45343=CARTESIAN_POINT('Ctrl Pts',(-0.103149623928905,0.0795101044780683,
-1.58056445172242));
#45344=CARTESIAN_POINT('Ctrl Pts',(-0.117571190691948,0.0200660889067739,
-1.57656432157308));
#45345=CARTESIAN_POINT('Ctrl Pts',(-0.117581030135854,-6.48590087786935E-6,
-1.57521328852638));
#45346=CARTESIAN_POINT('Origin',(0.,0.,-3.06008671147362));
#45347=CARTESIAN_POINT('',(-0.117617850646942,-6.5871718804936E-5,-1.68508671147362));
#45348=CARTESIAN_POINT('',(-0.117942108415767,-5.09551612454251E-5,-1.67521328852638));
#45349=CARTESIAN_POINT('',(-0.117775,1.13296574333067E-13,-3.06008671147362));
#45350=CARTESIAN_POINT('Ctrl Pts',(-0.117617850646942,-6.58717188049326E-5,
-1.68508671147362));
#45351=CARTESIAN_POINT('Ctrl Pts',(-0.117695889536837,-0.0154495527158428,
-1.68405046543029));
#45352=CARTESIAN_POINT('Ctrl Pts',(-0.107732741084233,-0.0700635255376361,
-1.68036512228432));
#45353=CARTESIAN_POINT('Ctrl Pts',(-0.0251302696981556,-0.136970009362336,
-1.6740306820357));
#45354=CARTESIAN_POINT('Ctrl Pts',(0.101553236631872,-0.0952851197690979,
-1.66608339072774));
#45355=CARTESIAN_POINT('Ctrl Pts',(0.135093630531518,0.0337938590521173,
-1.65813609941979));
#45356=CARTESIAN_POINT('Ctrl Pts',(0.0447281634802288,0.131877614899218,
-1.65018880811184));
#45357=CARTESIAN_POINT('Ctrl Pts',(-0.0822940200144428,0.109765453494247,
-1.64250567879645));
#45358=CARTESIAN_POINT('Ctrl Pts',(-0.117682355072768,0.0351061695311471,
-1.63747164658371));
#45359=CARTESIAN_POINT('Ctrl Pts',(-0.117921249980265,-6.69982741048542E-5,
-1.63508671147362));
#45360=CARTESIAN_POINT('Ctrl Pts',(-0.117942108415767,-5.09551612454281E-5,
-1.67521328852638));
#45361=CARTESIAN_POINT('Ctrl Pts',(-0.117957552138955,-0.00289799243842009,
-1.67502015347155));
#45362=CARTESIAN_POINT('Ctrl Pts',(-0.116572218065069,-0.0447805435194828,
-1.67217792131407));
#45363=CARTESIAN_POINT('Ctrl Pts',(-0.0666774638491984,-0.122255590674703,
-1.66668659205393));
#45364=CARTESIAN_POINT('Ctrl Pts',(0.0666879758411977,-0.122249856911105,
-1.65873930074598));
#45365=CARTESIAN_POINT('Ctrl Pts',(0.138888199753706,-0.0101183796013297,
-1.65079200943803));
#45366=CARTESIAN_POINT('Ctrl Pts',(0.0837022404783003,0.111293524409529,
-1.64284471813008));
#45367=CARTESIAN_POINT('Ctrl Pts',(-0.0482541640740641,0.130628669464612,
-1.63489742682213));
#45368=CARTESIAN_POINT('Ctrl Pts',(-0.113108473408961,0.056325488927834,
-1.6290202836209));
#45369=CARTESIAN_POINT('Ctrl Pts',(-0.117871336139931,0.00866995775128773,
-1.62579223752231));
#45370=CARTESIAN_POINT('Ctrl Pts',(-0.117791976321323,0.000107252653627225,
-1.62521328852638));
#45371=CARTESIAN_POINT('Origin',(0.,0.,-3.06008671147362));
#45372=CARTESIAN_POINT('',(-0.11768023886796,9.66154492266578E-5,-1.73508671147362));
#45373=CARTESIAN_POINT('',(-0.117637551566029,-7.88858851605845E-5,-1.72521328852638));
#45374=CARTESIAN_POINT('',(-0.117775,1.13296574333067E-13,-3.06008671147362));
#45375=CARTESIAN_POINT('Ctrl Pts',(-0.11768023886796,9.66154492266658E-5,
-1.73508671147362));
#45376=CARTESIAN_POINT('Ctrl Pts',(-0.117473587897162,-0.026713351369385,
-1.73327838137953));
#45377=CARTESIAN_POINT('Ctrl Pts',(-0.0950796332385711,-0.0931105570833916,
-1.72882095418279));
#45378=CARTESIAN_POINT('Ctrl Pts',(0.0152339085805741,-0.138420525750985,
-1.72171442988341));
#45379=CARTESIAN_POINT('Ctrl Pts',(0.124626240732756,-0.062133839738435,
-1.71376713857545));
#45380=CARTESIAN_POINT('Ctrl Pts',(0.11971324557739,0.0711410764126323,
-1.7058198472675));
#45381=CARTESIAN_POINT('Ctrl Pts',(0.00500104891906081,0.139166459427298,
-1.69787255595955));
#45382=CARTESIAN_POINT('Ctrl Pts',(-0.0987426466397743,0.087323766405728,
-1.69096151069492));
#45383=CARTESIAN_POINT('Ctrl Pts',(-0.117496388078233,0.0238778493233859,
-1.68669956253294));
#45384=CARTESIAN_POINT('Ctrl Pts',(-0.117617850646942,-6.58717188049326E-5,
-1.68508671147362));
#45385=CARTESIAN_POINT('Ctrl Pts',(-0.117637551566029,-7.88858851605862E-5,
-1.72521328852638));
#45386=CARTESIAN_POINT('Ctrl Pts',(-0.117725496492675,-0.0144021151159734,
-1.72424806942079));
#45387=CARTESIAN_POINT('Ctrl Pts',(-0.108664165918674,-0.06792878474672,
-1.72063375321254));
#45388=CARTESIAN_POINT('Ctrl Pts',(-0.0287884036356622,-0.136248087886369,
-1.71437033990164));
#45389=CARTESIAN_POINT('Ctrl Pts',(0.0989657326610272,-0.0979698800420198,
-1.70642304859369));
#45390=CARTESIAN_POINT('Ctrl Pts',(0.135949976537486,0.0301648390686699,
-1.69847575728574));
#45391=CARTESIAN_POINT('Ctrl Pts',(0.0482429316917392,0.130632818152132,
-1.69052846597779));
#45392=CARTESIAN_POINT('Ctrl Pts',(-0.0805050460052469,0.111756485186054,
-1.68277430972467));
#45393=CARTESIAN_POINT('Ctrl Pts',(-0.117745721498532,0.0361528065407269,
-1.6776692505742));
#45394=CARTESIAN_POINT('Ctrl Pts',(-0.117942108415767,-5.09551612454281E-5,
-1.67521328852638));
#45395=CARTESIAN_POINT('Origin',(0.,0.,-3.06008671147362));
#45396=CARTESIAN_POINT('',(-0.117965285605798,1.88808896691469E-5,-1.78508671147362));
#45397=CARTESIAN_POINT('',(-0.117654705075576,8.73580116268896E-5,-1.77521328852638));
#45398=CARTESIAN_POINT('',(-0.117775,1.13296574333067E-13,-3.06008671147362));
#45399=CARTESIAN_POINT('Ctrl Pts',(-0.117965285605798,1.88808896691539E-5,
-1.78508671147362));
#45400=CARTESIAN_POINT('Ctrl Pts',(-0.117880735353708,-0.0379995363499562,
-1.78250629732877));
#45401=CARTESIAN_POINT('Ctrl Pts',(-0.0772533694302627,-0.1152034904333,
-1.77727678608127));
#45402=CARTESIAN_POINT('Ctrl Pts',(0.054316540209444,-0.128226469106407,
-1.76939817773111));
#45403=CARTESIAN_POINT('Ctrl Pts',(0.137215110676543,-0.0237555745425038,
-1.76145088642316));
#45404=CARTESIAN_POINT('Ctrl Pts',(0.0942620302777797,0.102503578316717,
-1.75350359511521));
#45405=CARTESIAN_POINT('Ctrl Pts',(-0.0351467769424353,0.13474797954099,
-1.74555630380726));
#45406=CARTESIAN_POINT('Ctrl Pts',(-0.110208765147338,0.0641880976310302,
-1.7394173425934));
#45407=CARTESIAN_POINT('Ctrl Pts',(-0.117776319400548,0.0125616712902332,
-1.73592747848218));
#45408=CARTESIAN_POINT('Ctrl Pts',(-0.11768023886796,9.66154492266658E-5,
-1.73508671147362));
#45409=CARTESIAN_POINT('Ctrl Pts',(-0.117654705075576,8.73580116268809E-5,
-1.77521328852638));
#45410=CARTESIAN_POINT('Ctrl Pts',(-0.117477780202669,-0.0256836588302884,
-1.77347598537002));
#45411=CARTESIAN_POINT('Ctrl Pts',(-0.0964484074419039,-0.0910137929807851,
-1.76908958511102));
#45412=CARTESIAN_POINT('Ctrl Pts',(0.0115224698662327,-0.138778767557446,
-1.76205408774935));
#45413=CARTESIAN_POINT('Ctrl Pts',(0.122918035611167,-0.0654482250185099,
-1.7541067964414));
#45414=CARTESIAN_POINT('Ctrl Pts',(0.121575014282259,0.06791045235345,-1.74615950513345));
#45415=CARTESIAN_POINT('Ctrl Pts',(0.00872520499083007,0.138982676742282,
-1.7382122138255));
#45416=CARTESIAN_POINT('Ctrl Pts',(-0.0974493906730333,0.0894320653748823,
-1.73123014162315));
#45417=CARTESIAN_POINT('Ctrl Pts',(-0.117484126788099,0.0249087779610027,
-1.72689716652344));
#45418=CARTESIAN_POINT('Ctrl Pts',(-0.117637551566029,-7.88858851605862E-5,
-1.72521328852638));
#45419=CARTESIAN_POINT('Origin',(0.,0.,-3.06008671147362));
#45420=CARTESIAN_POINT('',(-0.117736502923752,-0.000107109896749501,-1.83508671147362));
#45421=CARTESIAN_POINT('',(-0.117954382942583,3.76844323675355E-5,-1.82521328852638));
#45422=CARTESIAN_POINT('',(-0.117775,1.13296574333067E-13,-3.06008671147362));
#45423=CARTESIAN_POINT('Ctrl Pts',(-0.117736502923752,-0.000107109896749515,
-1.83508671147362));
#45424=CARTESIAN_POINT('Ctrl Pts',(-0.117828850108629,-0.0105229883610132,
-1.83438331038065));
#45425=CARTESIAN_POINT('Ctrl Pts',(-0.11178794712638,-0.0600610348697975,
-1.83103081218504));
#45426=CARTESIAN_POINT('Ctrl Pts',(-0.0420745638576578,-0.132748050818114,
-1.82502921688678));
#45427=CARTESIAN_POINT('Ctrl Pts',(0.0888298139634637,-0.107245410489387,
-1.81708192557882));
#45428=CARTESIAN_POINT('Ctrl Pts',(0.13826081266264,0.0166211191466418,
-1.80913463427087));
#45429=CARTESIAN_POINT('Ctrl Pts',(0.0608810582468267,0.125243006457714,
-1.80118734296292));
#45430=CARTESIAN_POINT('Ctrl Pts',(-0.072337893827657,0.118993878146731,
-1.79324005165497));
#45431=CARTESIAN_POINT('Ctrl Pts',(-0.117496963864637,0.0410709634385956,
-1.78787317449187));
#45432=CARTESIAN_POINT('Ctrl Pts',(-0.117967536082299,0.00103081819907492,
-1.78515539443142));
#45433=CARTESIAN_POINT('Ctrl Pts',(-0.117965285605798,1.88808896691539E-5,
-1.78508671147362));
#45434=CARTESIAN_POINT('Ctrl Pts',(-0.117954382942583,3.76844323675288E-5,
-1.82521328852638));
#45435=CARTESIAN_POINT('Ctrl Pts',(-0.117799847059692,-0.0369433981909912,
-1.82270390131926));
#45436=CARTESIAN_POINT('Ctrl Pts',(-0.0791275006836936,-0.113242981745652,
-1.81754541700949));
#45437=CARTESIAN_POINT('Ctrl Pts',(0.0508640200603842,-0.129634737242294,
-1.80973783559706));
#45438=CARTESIAN_POINT('Ctrl Pts',(0.136529906497424,-0.0274207634537505,
-1.80179054428911));
#45439=CARTESIAN_POINT('Ctrl Pts',(0.0969726011114629,0.0999431251775667,
-1.79384325298116));
#45440=CARTESIAN_POINT('Ctrl Pts',(-0.0315265261952861,0.13564067156513,
-1.78589596167321));
#45441=CARTESIAN_POINT('Ctrl Pts',(-0.109340731502731,0.0663229187380152,
-1.77968597352162));
#45442=CARTESIAN_POINT('Ctrl Pts',(-0.117747561079132,0.0136128368897407,
-1.77612508247267));
#45443=CARTESIAN_POINT('Ctrl Pts',(-0.117654705075576,8.73580116268809E-5,
-1.77521328852638));
#45444=CARTESIAN_POINT('Origin',(0.,0.,-3.06008671147362));
#45445=CARTESIAN_POINT('',(-0.117591087501129,3.6292447154734E-5,-1.88508671147362));
#45446=CARTESIAN_POINT('',(-0.11776790710648,-0.000108326905674527,-1.87521328852638));
#45447=CARTESIAN_POINT('',(-0.117775,1.13296574333067E-13,-3.06008671147362));
#45448=CARTESIAN_POINT('Ctrl Pts',(-0.117591087501129,3.62924471547406E-5,
-1.88508671147362));
#45449=CARTESIAN_POINT('Ctrl Pts',(-0.117530670031507,-0.0218806161763991,
-1.88361122632989));
#45450=CARTESIAN_POINT('Ctrl Pts',(-0.101124441328067,-0.0832313222762371,
-1.87948664408351));
#45451=CARTESIAN_POINT('Ctrl Pts',(-0.00220927137030462,-0.139238762705767,
-1.87271296473448));
#45452=CARTESIAN_POINT('Ctrl Pts',(0.115870314076337,-0.077242373317187,
-1.86476567342653));
#45453=CARTESIAN_POINT('Ctrl Pts',(0.127675377417112,0.0555995676351779,
-1.85681838211858));
#45454=CARTESIAN_POINT('Ctrl Pts',(0.0223784908076123,0.137446415264255,
-1.84887109081063));
#45455=CARTESIAN_POINT('Ctrl Pts',(-0.0923073152845968,0.0971430293605453,
-1.84162720059564));
#45456=CARTESIAN_POINT('Ctrl Pts',(-0.117481058980149,0.0287045217143467,
-1.83703240748331));
#45457=CARTESIAN_POINT('Ctrl Pts',(-0.117736502923752,-0.000107109896749515,
-1.83508671147362));
#45458=CARTESIAN_POINT('Ctrl Pts',(-0.11776790710648,-0.000108326905674527,
-1.87521328852638));
#45459=CARTESIAN_POINT('Ctrl Pts',(-0.117853798527441,-0.00946608599639612,
-1.87458091437115));
#45460=CARTESIAN_POINT('Ctrl Pts',(-0.112554198892079,-0.0579285772143487,
-1.87129944311326));
#45461=CARTESIAN_POINT('Ctrl Pts',(-0.0456135877873082,-0.131573987724592,
-1.86536887475272));
#45462=CARTESIAN_POINT('Ctrl Pts',(0.085926654297937,-0.109585234944059,
-1.85742158344477));
#45463=CARTESIAN_POINT('Ctrl Pts',(0.138656251961757,0.0129134591995952,
-1.84947429213682));
#45464=CARTESIAN_POINT('Ctrl Pts',(0.0642124054894162,0.123568121365685,
-1.84152700082887));
#45465=CARTESIAN_POINT('Ctrl Pts',(-0.0691261005948764,0.120887947509786,
-1.83357970952092));
#45466=CARTESIAN_POINT('Ctrl Pts',(-0.116980282886529,0.0431871392476156,
-1.82814180542009));
#45467=CARTESIAN_POINT('Ctrl Pts',(-0.117962986713253,0.00209660271135738,
-1.82535299842191));
#45468=CARTESIAN_POINT('Ctrl Pts',(-0.117954382942583,3.76844323675288E-5,
-1.82521328852638));
#45469=CARTESIAN_POINT('Origin',(0.,0.,-3.06008671147362));
#45470=CARTESIAN_POINT('',(-0.117869880861692,9.13799831027575E-5,-1.93508671147362));
#45471=CARTESIAN_POINT('',(-0.117583632441682,1.94776852104478E-5,-1.92521328852638));
#45472=CARTESIAN_POINT('',(-0.117775,1.13296574333067E-13,-3.06008671147362));
#45473=CARTESIAN_POINT('Ctrl Pts',(-0.117869880861692,9.13799831027641E-5,
-1.93508671147362));
#45474=CARTESIAN_POINT('Ctrl Pts',(-0.117586069037807,-0.0330936947020148,
-1.93283914227913));
#45475=CARTESIAN_POINT('Ctrl Pts',(-0.0856179332394516,-0.10587091750467,
-1.92794247598199));
#45476=CARTESIAN_POINT('Ctrl Pts',(0.037841875214064,-0.134016067693779,
-1.92039671258219));
#45477=CARTESIAN_POINT('Ctrl Pts',(0.133163268965518,-0.0407413514532521,
-1.91244942127425));
#45478=CARTESIAN_POINT('Ctrl Pts',(0.106349300573725,0.0899007240643813,
-1.90450212996629));
#45479=CARTESIAN_POINT('Ctrl Pts',(-0.0180066584898106,0.138087197704393,
-1.89655483865834));
#45480=CARTESIAN_POINT('Ctrl Pts',(-0.105825629738042,0.0741898865853727,
-1.89008303249411));
#45481=CARTESIAN_POINT('Ctrl Pts',(-0.117639144009984,0.0174691660837329,
-1.88626032343254));
#45482=CARTESIAN_POINT('Ctrl Pts',(-0.117591087501129,3.62924471547406E-5,
-1.88508671147362));
#45483=CARTESIAN_POINT('Ctrl Pts',(-0.117583632441682,1.94776852104391E-5,
-1.92521328852638));
#45484=CARTESIAN_POINT('Ctrl Pts',(-0.117552877563387,-0.0208456941039662,
-1.92380883032038));
#45485=CARTESIAN_POINT('Ctrl Pts',(-0.102295467731519,-0.0811088855391901,
-1.91975527501173));
#45486=CARTESIAN_POINT('Ctrl Pts',(-0.00593636402933215,-0.139129699269039,
-1.91305262260043));
#45487=CARTESIAN_POINT('Ctrl Pts',(0.113760742075024,-0.0803169172660493,
-1.90510533129248));
#45488=CARTESIAN_POINT('Ctrl Pts',(0.129118194016824,0.052161342107116,
-1.89715803998453));
#45489=CARTESIAN_POINT('Ctrl Pts',(0.0260503661646103,0.136797997277999,
-1.88921074867658));
#45490=CARTESIAN_POINT('Ctrl Pts',(-0.0908080642029844,0.0992146499208666,
-1.88189583152386));
#45491=CARTESIAN_POINT('Ctrl Pts',(-0.117493988259224,0.0297347767986486,
-1.8772300114738));
#45492=CARTESIAN_POINT('Ctrl Pts',(-0.11776790710648,-0.000108326905674527,
-1.87521328852638));
#45493=CARTESIAN_POINT('Origin',(0.,0.,-3.06008671147362));
#45494=CARTESIAN_POINT('',(-0.117882453427845,-8.67389818698854E-5,-1.98508671147362));
#45495=CARTESIAN_POINT('',(-0.117839561452888,9.99727772240215E-5,-1.97521328852638));
#45496=CARTESIAN_POINT('',(-0.117775,1.13296574333067E-13,-3.06008671147362));
#45497=CARTESIAN_POINT('Ctrl Pts',(-0.117882453427845,-8.67389818699172E-5,
-1.98508671147362));
#45498=CARTESIAN_POINT('Ctrl Pts',(-0.117927594753219,-0.00555643476035982,
-1.98471615533101));
#45499=CARTESIAN_POINT('Ctrl Pts',(-0.115094354639881,-0.0500818457912055,
-1.98169650208576));
#45500=CARTESIAN_POINT('Ctrl Pts',(-0.058357257409372,-0.126438698298729,
-1.97602775173786));
#45501=CARTESIAN_POINT('Ctrl Pts',(0.0747095887255279,-0.117519322974067,
-1.9680804604299));
#45502=CARTESIAN_POINT('Ctrl Pts',(0.139253915509176,-0.000812979202544665,
-1.96013316912196));
#45503=CARTESIAN_POINT('Ctrl Pts',(0.0760766300741984,0.116639016955623,
-1.952185877814));
#45504=CARTESIAN_POINT('Ctrl Pts',(-0.0568770046268523,0.127111448203918,
-1.94423858650605));
#45505=CARTESIAN_POINT('Ctrl Pts',(-0.114816601332513,0.0510087171606275,
-1.93853886439259));
#45506=CARTESIAN_POINT('Ctrl Pts',(-0.117920583802556,0.00601988872629186,
-1.93548823938178));
#45507=CARTESIAN_POINT('Ctrl Pts',(-0.117869880861692,9.13799831027641E-5,
-1.93508671147362));
#45508=CARTESIAN_POINT('Ctrl Pts',(-0.117839561452888,9.9972777224025E-5,
-1.97521328852638));
#45509=CARTESIAN_POINT('Ctrl Pts',(-0.117548964242824,-0.0320578308581577,
-1.97303674626962));
#45510=CARTESIAN_POINT('Ctrl Pts',(-0.0872671618046854,-0.103836632251253,
-1.96821110691021));
#45511=CARTESIAN_POINT('Ctrl Pts',(0.0342402540498007,-0.13498117883315,
-1.96073637044814));
#45512=CARTESIAN_POINT('Ctrl Pts',(0.132024751554693,-0.0442919700792729,
-1.95278907914019));
#45513=CARTESIAN_POINT('Ctrl Pts',(0.108718118087273,0.0870211723441102,
-1.94484178783224));
#45514=CARTESIAN_POINT('Ctrl Pts',(-0.0143031501084346,0.138519794735472,
-1.93689449652429));
#45515=CARTESIAN_POINT('Ctrl Pts',(-0.104783611163582,0.0763213888572104,
-1.93035166342234));
#45516=CARTESIAN_POINT('Ctrl Pts',(-0.117610887590767,0.0185103122883274,
-1.92645792742304));
#45517=CARTESIAN_POINT('Ctrl Pts',(-0.117583632441682,1.94776852104391E-5,
-1.92521328852638));
#45518=CARTESIAN_POINT('Origin',(0.,0.,-3.06008671147362));
#45519=CARTESIAN_POINT('',(-0.117595734395081,-4.33641902384193E-5,-2.03508671147362));
#45520=CARTESIAN_POINT('',(-0.117909228031939,-7.4177712346371E-5,-2.02521328852638));
#45521=CARTESIAN_POINT('',(-0.117775,1.13296574333067E-13,-3.06008671147362));
#45522=CARTESIAN_POINT('Ctrl Pts',(-0.117595734395081,-4.33641902384211E-5,
-2.03508671147362));
#45523=CARTESIAN_POINT('Ctrl Pts',(-0.117651765097342,-0.0170145075963943,
-2.03394407128025));
#45524=CARTESIAN_POINT('Ctrl Pts',(-0.106267972168461,-0.073259904947786,
-2.03015233398423));
#45525=CARTESIAN_POINT('Ctrl Pts',(-0.0196177116792869,-0.137867542620766,
-2.02371149958557));
#45526=CARTESIAN_POINT('Ctrl Pts',(0.105292387066522,-0.0911363107968193,
-2.01576420827761));
#45527=CARTESIAN_POINT('Ctrl Pts',(0.133629880429484,0.039183784608208,
-2.00781691696966));
#45528=CARTESIAN_POINT('Ctrl Pts',(0.0394040425810417,0.133565097791645,
-1.99986962566171));
#45529=CARTESIAN_POINT('Ctrl Pts',(-0.0848840258511211,0.106753762101256,
-1.99229289049636));
#45530=CARTESIAN_POINT('Ctrl Pts',(-0.117604880485369,0.0335462910435847,
-1.98736525243366));
#45531=CARTESIAN_POINT('Ctrl Pts',(-0.117882453427845,-8.67389818699172E-5,
-1.98508671147362));
#45532=CARTESIAN_POINT('Ctrl Pts',(-0.117909228031939,-7.41777123463737E-5,
-2.02521328852638));
#45533=CARTESIAN_POINT('Ctrl Pts',(-0.117941722441543,-0.00449283611884619,
-2.02491375932151));
#45534=CARTESIAN_POINT('Ctrl Pts',(-0.115708932072434,-0.0479578416298998,
-2.02196513301398));
#45535=CARTESIAN_POINT('Ctrl Pts',(-0.0617215220226959,-0.124830955118446,
-2.0163674096038));
#45536=CARTESIAN_POINT('Ctrl Pts',(0.0715364240393441,-0.11947741908932,
-2.00842011829585));
#45537=CARTESIAN_POINT('Ctrl Pts',(0.139182230024373,-0.00454097809115471,
-2.0004728269879));
#45538=CARTESIAN_POINT('Ctrl Pts',(0.0791721726471583,0.114560380214585,
-1.99252553567995));
#45539=CARTESIAN_POINT('Ctrl Pts',(-0.0534534194270322,0.128588668194905,
-1.984578244372));
#45540=CARTESIAN_POINT('Ctrl Pts',(-0.114156913744517,0.0531357723352751,
-1.97880749532081));
#45541=CARTESIAN_POINT('Ctrl Pts',(-0.117902653781737,0.00708183857550709,
-1.97568584337227));
#45542=CARTESIAN_POINT('Ctrl Pts',(-0.117839561452888,9.9972777224025E-5,
-1.97521328852638));
#45543=CARTESIAN_POINT('Origin',(0.,0.,-3.06008671147362));
#45544=CARTESIAN_POINT('',(-0.117723193797192,0.000105656000806925,-2.08508671147362));
#45545=CARTESIAN_POINT('',(-0.117609472469646,-5.87439815582097E-5,-2.07521328852638));
#45546=CARTESIAN_POINT('',(-0.117775,1.13296574333067E-13,-3.06008671147362));
#45547=CARTESIAN_POINT('Ctrl Pts',(-0.117723193797192,0.00010565600080692,
-2.08508671147362));
#45548=CARTESIAN_POINT('Ctrl Pts',(-0.117477437827794,-0.028255491134646,
-2.08317198722949));
#45549=CARTESIAN_POINT('Ctrl Pts',(-0.0929469453665676,-0.0962366779196943,
-2.07860816588271));
#45550=CARTESIAN_POINT('Ctrl Pts',(0.0207721664357911,-0.137698333400896,
-2.07139524743328));
#45551=CARTESIAN_POINT('Ctrl Pts',(0.127017504190175,-0.0570864918270448,
-2.06344795612532));
#45552=CARTESIAN_POINT('Ctrl Pts',(0.116764283495866,0.0758842277388233,
-2.05550066481737));
#45553=CARTESIAN_POINT('Ctrl Pts',(-0.000583394708775192,0.139255066588021,
-2.04755337350942));
#45554=CARTESIAN_POINT('Ctrl Pts',(-0.100600990582941,0.0841555705722101,
-2.04074872239483));
#45555=CARTESIAN_POINT('Ctrl Pts',(-0.117521863513378,0.022331392440132,
-2.0365931683829));
#45556=CARTESIAN_POINT('Ctrl Pts',(-0.117595734395081,-4.33641902384211E-5,
-2.03508671147362));
#45557=CARTESIAN_POINT('Ctrl Pts',(-0.117609472469646,-5.87439815582062E-5,
-2.07521328852638));
#45558=CARTESIAN_POINT('Ctrl Pts',(-0.11768113966839,-0.0159703079548739,
-2.07414167527074));
#45559=CARTESIAN_POINT('Ctrl Pts',(-0.107255162124516,-0.0711262908138071,
-2.07042096491246));
#45560=CARTESIAN_POINT('Ctrl Pts',(-0.0233018516916921,-0.1372928889066,
-2.06405115745151));
#45561=CARTESIAN_POINT('Ctrl Pts',(0.102814620106721,-0.0939226678118359,
-2.05610386614357));
#45562=CARTESIAN_POINT('Ctrl Pts',(0.134631057384304,0.035592021917362,
-2.04815657483561));
#45563=CARTESIAN_POINT('Ctrl Pts',(0.0429658988952774,0.132462240539342,
-2.04020928352766));
#45564=CARTESIAN_POINT('Ctrl Pts',(-0.0831668745964641,0.108768066411958,
-2.03256152142458));
#45565=CARTESIAN_POINT('Ctrl Pts',(-0.117654335285522,0.0345866759678852,
-2.02756285642416));
#45566=CARTESIAN_POINT('Ctrl Pts',(-0.117909228031939,-7.41777123463737E-5,
-2.02521328852638));
#45567=CARTESIAN_POINT('Origin',(0.,0.,-3.06008671147362));
#45568=CARTESIAN_POINT('',(-0.117967850519022,-1.0412081018357E-5,-2.13508671147362));
#45569=CARTESIAN_POINT('',(-0.117693964354226,0.000100292661075557,-2.12521328852638));
#45570=CARTESIAN_POINT('',(-0.117775,1.13296574333067E-13,-3.06008671147362));
#45571=CARTESIAN_POINT('Ctrl Pts',(-0.117967850519022,-1.04120810183751E-5,
-2.13508671147362));
#45572=CARTESIAN_POINT('Ctrl Pts',(-0.117968551785685,-0.000565995771811528,
-2.13504900028137));
#45573=CARTESIAN_POINT('Ctrl Pts',(-0.117713150989245,-0.0401489893130429,
-2.13236219198648));
#45574=CARTESIAN_POINT('Ctrl Pts',(-0.0737223134758439,-0.118141163087173,
-2.12702628658893));
#45575=CARTESIAN_POINT('Ctrl Pts',(0.0594145941073171,-0.125945305299099,
-2.11907899528099));
#45576=CARTESIAN_POINT('Ctrl Pts',(0.138057323045987,-0.0182342938771007,
-2.11113170397303));
#45577=CARTESIAN_POINT('Ctrl Pts',(0.0900759365079238,0.106200939647636,
-2.10318441266508));
#45578=CARTESIAN_POINT('Ctrl Pts',(-0.0405217541450246,0.133230256926986,
-2.09523712135713));
#45579=CARTESIAN_POINT('Ctrl Pts',(-0.111443182865655,0.060991274530224,
-2.08920455429331));
#45580=CARTESIAN_POINT('Ctrl Pts',(-0.117817450980334,0.010983283291857,
-2.08582108433214));
#45581=CARTESIAN_POINT('Ctrl Pts',(-0.117723193797192,0.00010565600080692,
-2.08508671147362));
#45582=CARTESIAN_POINT('Ctrl Pts',(-0.117693964354226,0.000100292661075554,
-2.12521328852638));
#45583=CARTESIAN_POINT('Ctrl Pts',(-0.117473453135155,-0.0272259720969255,
-2.12336959121998));
#45584=CARTESIAN_POINT('Ctrl Pts',(-0.0943817212641257,-0.0941517958408477,
-2.11887679681093));
#45585=CARTESIAN_POINT('Ctrl Pts',(0.0170780778737081,-0.138205111673633,
-2.11173490529922));
#45586=CARTESIAN_POINT('Ctrl Pts',(0.125443576141085,-0.0604667085388119,
-2.10378761399128));
#45587=CARTESIAN_POINT('Ctrl Pts',(0.118754099267359,0.0727308568888059,
-2.09584032268332));
#45588=CARTESIAN_POINT('Ctrl Pts',(0.00314513556600165,0.139220766262987,
-2.08789303137537));
#45589=CARTESIAN_POINT('Ctrl Pts',(-0.0993708103736951,0.0862718543664017,
-2.08101735332306));
#45590=CARTESIAN_POINT('Ctrl Pts',(-0.117503973729512,0.0233641047155024,
-2.07679077237339));
#45591=CARTESIAN_POINT('Ctrl Pts',(-0.117609472469646,-5.87439815582062E-5,
-2.07521328852638));
#45592=CARTESIAN_POINT('Origin',(0.,0.,-3.06008671147362));
#45593=CARTESIAN_POINT('',(-0.117692226381986,-9.98710273162283E-5,-2.18508671147362));
#45594=CARTESIAN_POINT('',(-0.11796809735242,9.20234616148905E-6,-2.17521328852638));
#45595=CARTESIAN_POINT('',(-0.117775,1.13296574333067E-13,-3.06008671147362));
#45596=CARTESIAN_POINT('Ctrl Pts',(-0.117692226381986,-9.98710273162218E-5,
-2.18508671147362));
#45597=CARTESIAN_POINT('Ctrl Pts',(-0.117788571289341,-0.0121026577886401,
-2.18427691623061));
#45598=CARTESIAN_POINT('Ctrl Pts',(-0.110576187009896,-0.063257325136989,
-2.18081802388496));
#45599=CARTESIAN_POINT('Ctrl Pts',(-0.0367176736873534,-0.134328427217807,
-2.17471003443665));
#45600=CARTESIAN_POINT('Ctrl Pts',(0.093058792097453,-0.103597177245249,
-2.16676274312869));
#45601=CARTESIAN_POINT('Ctrl Pts',(0.137483123155237,0.022151856971875,
-2.15881545182074));
#45602=CARTESIAN_POINT('Ctrl Pts',(0.0558099863031745,0.127583538705665,
-2.1508681605128));
#45603=CARTESIAN_POINT('Ctrl Pts',(-0.0764207885802381,0.116052481208713,
-2.14295858039708));
#45604=CARTESIAN_POINT('Ctrl Pts',(-0.117919289925354,0.0384620767452394,
-2.13769809738402));
#45605=CARTESIAN_POINT('Ctrl Pts',(-0.117967850519022,-1.04120810183751E-5,
-2.13508671147362));
#45606=CARTESIAN_POINT('Ctrl Pts',(-0.11796809735242,9.20234616149382E-6,
-2.17521328852638));
#45607=CARTESIAN_POINT('Ctrl Pts',(-0.117924925187486,-0.0385278244848899,
-2.17259750716922));
#45608=CARTESIAN_POINT('Ctrl Pts',(-0.0763018717954651,-0.116172667440745,
-2.1673326287094));
#45609=CARTESIAN_POINT('Ctrl Pts',(0.0560213207628474,-0.127490883033133,
-2.15941865314694));
#45610=CARTESIAN_POINT('Ctrl Pts',(0.137519639994184,-0.0219240108659811,
-2.15147136183898));
#45611=CARTESIAN_POINT('Ctrl Pts',(0.0928869986161953,0.103751236737962,
-2.14352407053103));
#45612=CARTESIAN_POINT('Ctrl Pts',(-0.0369402110727147,0.134267399030759,
-2.13557677922308));
#45613=CARTESIAN_POINT('Ctrl Pts',(-0.110627789111854,0.0631252406314027,
-2.12947318522153));
#45614=CARTESIAN_POINT('Ctrl Pts',(-0.117790292363326,0.01203748429871,
-2.12601868832263));
#45615=CARTESIAN_POINT('Ctrl Pts',(-0.117693964354226,0.000100292661075554,
-2.12521328852638));
#45616=CARTESIAN_POINT('Origin',(0.,0.,-3.06008671147362));
#45617=CARTESIAN_POINT('',(-0.117610460329433,5.96508612474619E-5,-2.23508671147362));
#45618=CARTESIAN_POINT('',(-0.117721328622872,-0.000105405280874327,-2.22521328852638));
#45619=CARTESIAN_POINT('',(-0.117775,1.13296574333067E-13,-3.06008671147362));
#45620=CARTESIAN_POINT('Ctrl Pts',(-0.117610460329433,5.96508612474792E-5,
-2.23508671147362));
#45621=CARTESIAN_POINT('Ctrl Pts',(-0.117502981482352,-0.0234279695405327,
-2.23350483217985));
#45622=CARTESIAN_POINT('Ctrl Pts',(-0.0992933102918214,-0.0864026580678686,
-2.22927385578343));
#45623=CARTESIAN_POINT('Ctrl Pts',(0.00337582615670157,-0.139215364516925,
-2.22239378228436));
#45624=CARTESIAN_POINT('Ctrl Pts',(0.118874455301411,-0.0725339768426726,
-2.21444649097641));
#45625=CARTESIAN_POINT('Ctrl Pts',(0.125343208860993,0.0606744914461575,
-2.20649919966845));
#45626=CARTESIAN_POINT('Ctrl Pts',(0.0168490426502724,0.138233222061811,
-2.19855190836051));
#45627=CARTESIAN_POINT('Ctrl Pts',(-0.0944690535724636,0.0940224986942619,
-2.19141441229555));
#45628=CARTESIAN_POINT('Ctrl Pts',(-0.117473396537287,0.0271622649282534,
-2.18692601333326));
#45629=CARTESIAN_POINT('Ctrl Pts',(-0.117692226381986,-9.98710273162218E-5,
-2.18508671147362));
#45630=CARTESIAN_POINT('Ctrl Pts',(-0.117721328622872,-0.00010540528087433,
-2.22521328852638));
#45631=CARTESIAN_POINT('Ctrl Pts',(-0.117815809071607,-0.0110485780997072,
-2.2244745202211));
#45632=CARTESIAN_POINT('Ctrl Pts',(-0.111393725741073,-0.0611233075246441,
-2.22108665481318));
#45633=CARTESIAN_POINT('Ctrl Pts',(-0.0403009298698327,-0.133297219356626,
-2.2150496923026));
#45634=CARTESIAN_POINT('Ctrl Pts',(0.0902517917743938,-0.106051533313259,
-2.20710240099464));
#45635=CARTESIAN_POINT('Ctrl Pts',(0.13802691747888,0.0184630357162695,
-2.19915510968669));
#45636=CARTESIAN_POINT('Ctrl Pts',(0.059205815238823,0.12604358404333,-2.19120781837874));
#45637=CARTESIAN_POINT('Ctrl Pts',(-0.0739179767846482,0.118018838939578,
-2.18326052707079));
#45638=CARTESIAN_POINT('Ctrl Pts',(-0.117743386247816,0.0400181840074988,
-2.17792901712));
#45639=CARTESIAN_POINT('Ctrl Pts',(-0.11796864721216,0.00050002692296339,
-2.17524660427187));
#45640=CARTESIAN_POINT('Ctrl Pts',(-0.11796809735242,9.20234616149382E-6,
-2.17521328852638));
#45641=CARTESIAN_POINT('Origin',(0.,0.,-3.06008671147362));
#45642=CARTESIAN_POINT('',(-0.117910775228005,7.33173023513087E-5,-2.28508671147362));
#45643=CARTESIAN_POINT('',(-0.117596460302673,4.43517738773561E-5,-2.27521328852638));
#45644=CARTESIAN_POINT('',(-0.117775,1.13296574333067E-13,-3.06008671147362));
#45645=CARTESIAN_POINT('Ctrl Pts',(-0.117910775228005,7.33173023513014E-5,
-2.28508671147362));
#45646=CARTESIAN_POINT('Ctrl Pts',(-0.117657693388436,-0.0346511833667682,
-2.28273274812909));
#45647=CARTESIAN_POINT('Ctrl Pts',(-0.0830590431455795,-0.108892231259704,
-2.2777296876819));
#45648=CARTESIAN_POINT('Ctrl Pts',(0.0431853359348615,-0.132390863279962,
-2.27007753013206));
#45649=CARTESIAN_POINT('Ctrl Pts',(0.134689851066473,-0.0353688837753169,
-2.26213023882412));
#45650=CARTESIAN_POINT('Ctrl Pts',(0.102658845743989,0.0940929078641549,
-2.25418294751616));
#45651=CARTESIAN_POINT('Ctrl Pts',(-0.0235293201795658,0.137254089234922,
-2.24623565620821));
#45652=CARTESIAN_POINT('Ctrl Pts',(-0.107315019292188,0.0709942209893211,
-2.23987024419403));
#45653=CARTESIAN_POINT('Ctrl Pts',(-0.117682971133598,0.015905617667775,
-2.2361539292825));
#45654=CARTESIAN_POINT('Ctrl Pts',(-0.117610460329433,5.96508612474792E-5,
-2.23508671147362));
#45655=CARTESIAN_POINT('Ctrl Pts',(-0.117596460302673,4.43517738773439E-5,
-2.27521328852638));
#45656=CARTESIAN_POINT('Ctrl Pts',(-0.117520659904767,-0.0223953420072019,
-2.27370243617034));
#45657=CARTESIAN_POINT('Ctrl Pts',(-0.100526067276438,-0.0842866703776684,
-2.26954248671165));
#45658=CARTESIAN_POINT('Ctrl Pts',(-0.00035264218412894,-0.139255841098576,
-2.2627334401503));
#45659=CARTESIAN_POINT('Ctrl Pts',(0.116889865813058,-0.0756906394925223,
-2.25478614884235));
#45660=CARTESIAN_POINT('Ctrl Pts',(0.126922734073552,0.0572968865810018,
-2.2468388575344));
#45661=CARTESIAN_POINT('Ctrl Pts',(0.020543965621383,0.137732563735411,
-2.23889156622645));
#45662=CARTESIAN_POINT('Ctrl Pts',(-0.09303702865732,0.0961079088722858,
-2.23168304322378));
#45663=CARTESIAN_POINT('Ctrl Pts',(-0.117477018301604,0.028191772631412,
-2.22712361732375));
#45664=CARTESIAN_POINT('Ctrl Pts',(-0.117721328622872,-0.00010540528087433,
-2.22521328852638));
#45665=CARTESIAN_POINT('Origin',(0.,0.,-3.06008671147362));
#45666=CARTESIAN_POINT('',(-0.117837633641763,-0.000100407954100913,-2.33508671147362));
#45667=CARTESIAN_POINT('',(-0.117884197500364,8.6037916559329E-5,-2.32521328852638));
#45668=CARTESIAN_POINT('',(-0.117775,1.13296574333067E-13,-3.06008671147362));
#45669=CARTESIAN_POINT('Ctrl Pts',(-0.117837633641763,-0.000100407954100916,
-2.33508671147362));
#45670=CARTESIAN_POINT('Ctrl Pts',(-0.117901463481007,-0.00714751330050535,
-2.33460976118097));
#45671=CARTESIAN_POINT('Ctrl Pts',(-0.114115041181782,-0.0532674687213532,
-2.33148371378567));
#45672=CARTESIAN_POINT('Ctrl Pts',(-0.0532402693961469,-0.128677067243725,
-2.32570856928773));
#45673=CARTESIAN_POINT('Ctrl Pts',(0.0793618960797965,-0.114429032026143,
-2.31776127797978));
#45674=CARTESIAN_POINT('Ctrl Pts',(0.139174515358953,0.00477160291947143,
-2.30981398667182));
#45675=CARTESIAN_POINT('Ctrl Pts',(0.0713383470518088,0.11959579490825,
-2.30186669536388));
#45676=CARTESIAN_POINT('Ctrl Pts',(-0.0619282880767048,0.124728509394241,
-2.29391940405591));
#45677=CARTESIAN_POINT('Ctrl Pts',(-0.115745950361329,0.0478264738904903,
-2.2883260760925));
#45678=CARTESIAN_POINT('Ctrl Pts',(-0.117942505966122,0.00442698423816777,
-2.28538184523174));
#45679=CARTESIAN_POINT('Ctrl Pts',(-0.117910775228005,7.33173023513014E-5,
-2.28508671147362));
#45680=CARTESIAN_POINT('Ctrl Pts',(-0.117884197500364,8.60379165593343E-5,
-2.32521328852638));
#45681=CARTESIAN_POINT('Ctrl Pts',(-0.117607682544816,-0.0336105716919928,
-2.32293035211958));
#45682=CARTESIAN_POINT('Ctrl Pts',(-0.0847791412331816,-0.106878836889164,
-2.31799831861012));
#45683=CARTESIAN_POINT('Ctrl Pts',(0.0396253113885193,-0.133499619227714,
-2.31041718799801));
#45684=CARTESIAN_POINT('Ctrl Pts',(0.13369462523368,-0.0389622999861087,
-2.30246989669006));
#45685=CARTESIAN_POINT('Ctrl Pts',(0.105141224899681,0.0913106590885011,
-2.29452260538211));
#45686=CARTESIAN_POINT('Ctrl Pts',(-0.0198461371346163,0.137834844931954,
-2.28657531407416));
#45687=CARTESIAN_POINT('Ctrl Pts',(-0.106330160380951,0.0731279015670244,
-2.28013887512225));
#45688=CARTESIAN_POINT('Ctrl Pts',(-0.117653566746173,0.0169499504312584,
-2.27635153327299));
#45689=CARTESIAN_POINT('Ctrl Pts',(-0.117596460302673,4.43517738773439E-5,
-2.27521328852638));
#45690=CARTESIAN_POINT('Origin',(0.,0.,-3.06008671147362));
#45691=CARTESIAN_POINT('',(-0.117583321031667,-1.84167202121336E-5,-2.38508671147362));
#45692=CARTESIAN_POINT('',(-0.117868059206978,-9.19955489654817E-5,-2.37521328852638));
#45693=CARTESIAN_POINT('',(-0.117775,1.13296574333067E-13,-3.06008671147362));
#45694=CARTESIAN_POINT('Ctrl Pts',(-0.117583321031667,-1.84167202121367E-5,
-2.38508671147362));
#45695=CARTESIAN_POINT('Ctrl Pts',(-0.117609178758956,-0.0185746748110054,
-2.38383767713021));
#45696=CARTESIAN_POINT('Ctrl Pts',(-0.104717853734675,-0.0764532318113364,
-2.37993954568415));
#45697=CARTESIAN_POINT('Ctrl Pts',(-0.0140735972308577,-0.138543306517508,
-2.37339231713544));
#45698=CARTESIAN_POINT('Ctrl Pts',(0.10886216750279,-0.086840902842008,
-2.36544502582749));
#45699=CARTESIAN_POINT('Ctrl Pts',(0.13195117753492,0.044510680369643,-2.35749773451953));
#45700=CARTESIAN_POINT('Ctrl Pts',(0.0340165375872002,0.135037732098843,
-2.34955044321158));
#45701=CARTESIAN_POINT('Ctrl Pts',(-0.0873676836443551,0.103710317580185,
-2.34208010219627));
#45702=CARTESIAN_POINT('Ctrl Pts',(-0.11754693713977,0.0319938115777102,
-2.33725885828362));
#45703=CARTESIAN_POINT('Ctrl Pts',(-0.117837633641763,-0.000100407954100916,
-2.33508671147362));
#45704=CARTESIAN_POINT('Ctrl Pts',(-0.117868059206978,-9.19955489654947E-5,
-2.37521328852638));
#45705=CARTESIAN_POINT('Ctrl Pts',(-0.117919547374431,-0.00608564309425205,
-2.37480736517147));
#45706=CARTESIAN_POINT('Ctrl Pts',(-0.114776697578318,-0.0511402889575705,
-2.3717523447139));
#45707=CARTESIAN_POINT('Ctrl Pts',(-0.0566662969110845,-0.127205520442183,
-2.36604822715368));
#45708=CARTESIAN_POINT('Ctrl Pts',(0.0762698010119113,-0.116512793675996,
-2.35810093584572));
#45709=CARTESIAN_POINT('Ctrl Pts',(0.13925237616884,0.00104372789252618,
-2.35015364453777));
#45710=CARTESIAN_POINT('Ctrl Pts',(0.0745147509671164,0.117642957821071,
-2.34220635322982));
#45711=CARTESIAN_POINT('Ctrl Pts',(-0.0585666913028059,0.126341823266975,
-2.33425906192187));
#45712=CARTESIAN_POINT('Ctrl Pts',(-0.115133288835063,0.0499503388447956,
-2.32859470702072));
#45713=CARTESIAN_POINT('Ctrl Pts',(-0.117928547797741,0.00549064488900448,
-2.32557944922223));
#45714=CARTESIAN_POINT('Ctrl Pts',(-0.117884197500364,8.60379165593343E-5,
-2.32521328852638));
#45715=CARTESIAN_POINT('Origin',(0.,0.,-3.06008671147362));
#45716=CARTESIAN_POINT('',(-0.117769879638916,0.000108303546025554,-2.43508671147362));
#45717=CARTESIAN_POINT('',(-0.117590495046852,-3.52740045776734E-5,-2.42521328852638));
#45718=CARTESIAN_POINT('',(-0.117775,1.13296574333067E-13,-3.06008671147362));
#45719=CARTESIAN_POINT('Ctrl Pts',(-0.117769879638916,0.000108303546025553,
-2.43508671147362));
#45720=CARTESIAN_POINT('Ctrl Pts',(-0.117495009512743,-0.0297985645403461,
-2.43306559307944));
#45721=CARTESIAN_POINT('Ctrl Pts',(-0.0907137933584123,-0.0993425203592325,
-2.42839537758262));
#45722=CARTESIAN_POINT('Ctrl Pts',(0.0262770108420999,-0.136754643873708,
-2.42107606498315));
#45723=CARTESIAN_POINT('Ctrl Pts',(0.129204451314017,-0.0519473163932888,
-2.41312877367519));
#45724=CARTESIAN_POINT('Ctrl Pts',(0.113627498086771,0.0805053141001346,
-2.40518148236725));
#45725=CARTESIAN_POINT('Ctrl Pts',(-0.00616689990636303,0.139119672459956,
-2.39723419105929));
#45726=CARTESIAN_POINT('Ctrl Pts',(-0.102366602030147,0.0809774201074958,
-2.39053593409475));
#45727=CARTESIAN_POINT('Ctrl Pts',(-0.117554336687715,0.0207815925356226,
-2.38648677423286));
#45728=CARTESIAN_POINT('Ctrl Pts',(-0.117583321031667,-1.84167202121367E-5,
-2.38508671147362));
#45729=CARTESIAN_POINT('Ctrl Pts',(-0.117590495046852,-3.52740045776734E-5,
-2.42521328852638));
#45730=CARTESIAN_POINT('Ctrl Pts',(-0.117637364608106,-0.0175336573692995,
-2.4240352811207));
#45731=CARTESIAN_POINT('Ctrl Pts',(-0.105762263505043,-0.0743218437255907,
-2.42020817661237));
#45732=CARTESIAN_POINT('Ctrl Pts',(-0.0177778171272468,-0.138116844934903,
-2.41373197500138));
#45733=CARTESIAN_POINT('Ctrl Pts',(0.106498123211473,-0.0897243745534934,
-2.40578468369343));
#45734=CARTESIAN_POINT('Ctrl Pts',(0.133095574977059,0.0409619525670818,
-2.39783739238548));
#45735=CARTESIAN_POINT('Ctrl Pts',(0.0376197525149271,0.134078588362562,
-2.38989010107753));
#45736=CARTESIAN_POINT('Ctrl Pts',(-0.08572135907778,0.105745412574563,
-2.3823487331245));
#45737=CARTESIAN_POINT('Ctrl Pts',(-0.117583530356522,0.0330295104295094,
-2.37745646227412));
#45738=CARTESIAN_POINT('Ctrl Pts',(-0.117868059206978,-9.19955489654947E-5,
-2.37521328852638));
#45739=CARTESIAN_POINT('Origin',(0.,0.,-3.06008671147362));
#45740=CARTESIAN_POINT('',(-0.117953497684312,-3.88090381494036E-5,-2.48508671147362));
#45741=CARTESIAN_POINT('',(-0.11773841333479,0.000107271409016091,-2.47521328852638));
#45742=CARTESIAN_POINT('',(-0.117775,1.13296574333067E-13,-3.06008671147362));
#45743=CARTESIAN_POINT('Ctrl Pts',(-0.117953497684312,-3.88090381494167E-5,
-2.48508671147362));
#45744=CARTESIAN_POINT('Ctrl Pts',(-0.117962605253777,-0.00216254596668706,
-2.48494260613133));
#45745=CARTESIAN_POINT('Ctrl Pts',(-0.116947344620421,-0.0433181804821695,
-2.4821494036864));
#45746=CARTESIAN_POINT('Ctrl Pts',(-0.0689256895917136,-0.121002327391366,
-2.47670710413881));
#45747=CARTESIAN_POINT('Ctrl Pts',(0.0644170755712456,-0.123461549863384,
-2.46875981283085));
#45748=CARTESIAN_POINT('Ctrl Pts',(0.138677460778961,-0.0126836821041933,
-2.46081252152291));
#45749=CARTESIAN_POINT('Ctrl Pts',(0.0857449494400285,0.109727469511273,
-2.45286523021495));
#45750=CARTESIAN_POINT('Ctrl Pts',(-0.0458315493375432,0.131498224342159,
-2.444917938907));
#45751=CARTESIAN_POINT('Ctrl Pts',(-0.112600512780524,0.0577966553949038,
-2.43899176599322));
#45752=CARTESIAN_POINT('Ctrl Pts',(-0.117855284129485,0.00940062231845771,
-2.43571469018209));
#45753=CARTESIAN_POINT('Ctrl Pts',(-0.117769879638916,0.000108303546025553,
-2.43508671147362));
#45754=CARTESIAN_POINT('Ctrl Pts',(-0.11773841333479,0.00010727140901609,
-2.47521328852638));
#45755=CARTESIAN_POINT('Ctrl Pts',(-0.117481668772501,-0.0287682554493046,
-2.47326319706994));
#45756=CARTESIAN_POINT('Ctrl Pts',(-0.0922158471109609,-0.0972715125940092,
-2.46866400851084));
#45757=CARTESIAN_POINT('Ctrl Pts',(0.0226062146261162,-0.137409143425246,
-2.46141572284909));
#45758=CARTESIAN_POINT('Ctrl Pts',(0.127767332108225,-0.0553879272272235,
-2.45346843154115));
#45759=CARTESIAN_POINT('Ctrl Pts',(0.115742160170272,0.0774342688717387,
-2.44552114023319));
#45760=CARTESIAN_POINT('Ctrl Pts',(-0.00243999302426519,0.139234909669319,
-2.43757384892524));
#45761=CARTESIAN_POINT('Ctrl Pts',(-0.101198093853741,0.0831000893788111,
-2.43080456502297));
#45762=CARTESIAN_POINT('Ctrl Pts',(-0.117531964575542,0.0218166187401381,
-2.42668437822335));
#45763=CARTESIAN_POINT('Ctrl Pts',(-0.117590495046852,-3.52740045776734E-5,
-2.42521328852638));
#45764=CARTESIAN_POINT('Origin',(0.,0.,-3.06008671147362));
#45765=CARTESIAN_POINT('',(-0.117653224368514,-8.67076276465346E-5,-2.53508671147362));
#45766=CARTESIAN_POINT('',(-0.117964807649162,-2.00728089981839E-5,-2.52521328852639));
#45767=CARTESIAN_POINT('',(-0.117775,1.13296574333067E-13,-3.06008671147362));
#45768=CARTESIAN_POINT('Ctrl Pts',(-0.117653224368514,-8.67076276465321E-5,
-2.53508671147362));
#45769=CARTESIAN_POINT('Ctrl Pts',(-0.117745757901207,-0.0136778186926029,
-2.53417052208057));
#45770=CARTESIAN_POINT('Ctrl Pts',(-0.109285840550885,-0.0664550385671571,
-2.53060523558487));
#45771=CARTESIAN_POINT('Ctrl Pts',(-0.0313017206303005,-0.135692727164734,
-2.52439085198651));
#45772=CARTESIAN_POINT('Ctrl Pts',(0.0971380788063926,-0.0997823008635477,
-2.51644356067857));
#45773=CARTESIAN_POINT('Ctrl Pts',(0.136484282651119,0.0276469620217102,
-2.50849626937061));
#45774=CARTESIAN_POINT('Ctrl Pts',(0.0506491401835047,0.129718844114848,
-2.50054897806267));
#45775=CARTESIAN_POINT('Ctrl Pts',(-0.0792418750448042,0.113121058725188,
-2.49274579209699));
#45776=CARTESIAN_POINT('Ctrl Pts',(-0.117795180261066,0.0368782366644444,
-2.48759170323398));
#45777=CARTESIAN_POINT('Ctrl Pts',(-0.117953497684312,-3.88090381494167E-5,
-2.48508671147362));
#45778=CARTESIAN_POINT('Ctrl Pts',(-0.117964807649162,-2.00728089981873E-5,
-2.52521328852638));
#45779=CARTESIAN_POINT('Ctrl Pts',(-0.117967343283893,-0.00109678191988592,
-2.52514021012183));
#45780=CARTESIAN_POINT('Ctrl Pts',(-0.117465836079,-0.0412018472256403,
-2.52241803461462));
#45781=CARTESIAN_POINT('Ctrl Pts',(-0.0721406159404224,-0.119113580956658,
-2.51704676200475));
#45782=CARTESIAN_POINT('Ctrl Pts',(0.0610885073433754,-0.125141951028183,
-2.50909947069681));
#45783=CARTESIAN_POINT('Ctrl Pts',(0.1382881637544,-0.0163919920088414,
-2.50115217938885));
#45784=CARTESIAN_POINT('Ctrl Pts',(0.0886519810374287,0.107392457345575,
-2.4932048880809));
#45785=CARTESIAN_POINT('Ctrl Pts',(-0.0422944750968055,0.132678148211631,
-2.48525759677295));
#45786=CARTESIAN_POINT('Ctrl Pts',(-0.111836348204514,0.0599290334960457,
-2.47926039692144));
#45787=CARTESIAN_POINT('Ctrl Pts',(-0.11783044281273,0.0104576353595844,
-2.47591229417259));
#45788=CARTESIAN_POINT('Ctrl Pts',(-0.11773841333479,0.00010727140901609,
-2.47521328852638));
#45789=CARTESIAN_POINT('Origin',(0.,0.,-3.06008671147362));
#45790=CARTESIAN_POINT('',(-0.117638891309021,7.96281316254408E-5,-2.58508671147362));
#45791=CARTESIAN_POINT('',(-0.117678576059632,-9.61137264129941E-5,-2.57521328852638));
#45792=CARTESIAN_POINT('',(-0.117775,1.13296574333067E-13,-3.06008671147362));
#45793=CARTESIAN_POINT('Ctrl Pts',(-0.117638891309021,7.96281316254328E-5,
-2.58508671147362));
#45794=CARTESIAN_POINT('Ctrl Pts',(-0.117483508336674,-0.0249725458388271,
-2.58339843802981));
#45795=CARTESIAN_POINT('Ctrl Pts',(-0.0973679568000036,-0.0895623381818424,
-2.57906106748334));
#45796=CARTESIAN_POINT('Ctrl Pts',(0.00895549343668939,-0.138968028902788,
-2.57207459983422));
#45797=CARTESIAN_POINT('Ctrl Pts',(0.121687378843393,-0.0677089045107432,
-2.56412730852628));
#45798=CARTESIAN_POINT('Ctrl Pts',(0.122809417189726,0.0656518161922446,
-2.55618001721832));
#45799=CARTESIAN_POINT('Ctrl Pts',(0.011292491656669,0.138797671277311,
-2.54823272591037));
#45800=CARTESIAN_POINT('Ctrl Pts',(-0.096531683990788,0.0908838025098833,
-2.54120162399547));
#45801=CARTESIAN_POINT('Ctrl Pts',(-0.117478203708577,0.0256199217277792,
-2.53681961918322));
#45802=CARTESIAN_POINT('Ctrl Pts',(-0.117653224368514,-8.67076276465321E-5,
-2.53508671147362));
#45803=CARTESIAN_POINT('Ctrl Pts',(-0.117678576059632,-9.61137264130253E-5,
-2.57521328852638));
#45804=CARTESIAN_POINT('Ctrl Pts',(-0.117774563927174,-0.0126267819892236,
-2.57436812607106));
#45805=CARTESIAN_POINT('Ctrl Pts',(-0.110156077978415,-0.0643201985882453,
-2.57087386651309));
#45806=CARTESIAN_POINT('Ctrl Pts',(-0.0349234451532213,-0.134806033304195,
-2.56473050985246));
#45807=CARTESIAN_POINT('Ctrl Pts',(0.0944317530776,-0.102347240545473,-2.55678321854452));
#45808=CARTESIAN_POINT('Ctrl Pts',(0.137175557268965,0.0239829131785638,
-2.54883592723656));
#45809=CARTESIAN_POINT('Ctrl Pts',(0.0541039883893578,0.128316297004496,
-2.54088863592861));
#45810=CARTESIAN_POINT('Ctrl Pts',(-0.077370769783318,0.11508270631958,
-2.53301442302521));
#45811=CARTESIAN_POINT('Ctrl Pts',(-0.117875426353606,0.0379339960955099,
-2.52778930722448));
#45812=CARTESIAN_POINT('Ctrl Pts',(-0.117964807649162,-2.00728089981873E-5,
-2.52521328852638));
#45813=CARTESIAN_POINT('Origin',(0.,0.,-3.06008671147362));
#45814=CARTESIAN_POINT('',(-0.117943238001422,4.98985662682079E-5,-2.63508671147362));
#45815=CARTESIAN_POINT('',(-0.117618959460295,6.6729458887721E-5,-2.62521328852638));
#45816=CARTESIAN_POINT('',(-0.117775,1.13296574333067E-13,-3.06008671147362));
#45817=CARTESIAN_POINT('Ctrl Pts',(-0.117943238001422,4.98985662681943E-5,
-2.63508671147362));
#45818=CARTESIAN_POINT('Ctrl Pts',(-0.117749962726917,-0.0362177372561391,
-2.63262635397904));
#45819=CARTESIAN_POINT('Ctrl Pts',(-0.0803927491711805,-0.111879153836378,
-2.62751689938181));
#45820=CARTESIAN_POINT('Ctrl Pts',(0.0484593300923006,-0.130552699117355,
-2.61975834768194));
#45821=CARTESIAN_POINT('Ctrl Pts',(0.135999775339708,-0.0299395228313577,
-2.61181105637398));
#45822=CARTESIAN_POINT('Ctrl Pts',(0.0988032571470193,0.0981337367930133,
-2.60386376506603));
#45823=CARTESIAN_POINT('Ctrl Pts',(-0.0290141333502425,0.136200198185447,
-2.59591647375808));
#45824=CARTESIAN_POINT('Ctrl Pts',(-0.108720603964012,0.0677966676599294,
-2.58965745589394));
#45825=CARTESIAN_POINT('Ctrl Pts',(-0.117727322265842,0.0143372245798384,
-2.58604753513246));
#45826=CARTESIAN_POINT('Ctrl Pts',(-0.117638891309021,7.96281316254328E-5,
-2.58508671147362));
#45827=CARTESIAN_POINT('Ctrl Pts',(-0.117618959460295,6.6729458887714E-5,
-2.62521328852638));
#45828=CARTESIAN_POINT('Ctrl Pts',(-0.117495510368196,-0.0239416772140386,
-2.6235960420203));
#45829=CARTESIAN_POINT('Ctrl Pts',(-0.0986638469305919,-0.0874544040157706,
-2.61932969841156));
#45830=CARTESIAN_POINT('Ctrl Pts',(0.00523164691012173,-0.139157980393471,
-2.61241425770018));
#45831=CARTESIAN_POINT('Ctrl Pts',(0.119830964215785,-0.0709426081540357,
-2.60446696639222));
#45832=CARTESIAN_POINT('Ctrl Pts',(0.12452311024091,0.0623402650981849,
-2.59651967508427));
#45833=CARTESIAN_POINT('Ctrl Pts',(0.0150045187058493,0.138445577953893,
-2.58857238377632));
#45834=CARTESIAN_POINT('Ctrl Pts',(-0.0951656069162575,0.0929810151014424,
-2.58147025492369));
#45835=CARTESIAN_POINT('Ctrl Pts',(-0.117473697294737,0.0266496396978196,
-2.57701722317371));
#45836=CARTESIAN_POINT('Ctrl Pts',(-0.117678576059632,-9.61137264130253E-5,
-2.57521328852638));
#45837=CARTESIAN_POINT('Origin',(0.,0.,-3.06008671147362));
#45838=CARTESIAN_POINT('',(-0.117789991982999,-0.00010740623187117,-2.68508671147362));
#45839=CARTESIAN_POINT('',(-0.11792267289879,6.60661965921575E-5,-2.67521328852638));
#45840=CARTESIAN_POINT('',(-0.117775,1.13296574333067E-13,-3.06008671147362));
#45841=CARTESIAN_POINT('Ctrl Pts',(-0.117789991982999,-0.000107406231871198,
-2.68508671147362));
#45842=CARTESIAN_POINT('Ctrl Pts',(-0.11786993715536,-0.0087354930933903,
-2.68450336703093));
#45843=CARTESIAN_POINT('Ctrl Pts',(-0.113063580952104,-0.0564573476549392,
-2.68127092548559));
#45844=CARTESIAN_POINT('Ctrl Pts',(-0.0480376407722225,-0.130708450334381,
-2.67538938683759));
#45845=CARTESIAN_POINT('Ctrl Pts',(0.0838865444021125,-0.111154674162296,
-2.66744209552965));
#45846=CARTESIAN_POINT('Ctrl Pts',(0.138871243492067,0.0103485095922432,
-2.65949480422169));
#45847=CARTESIAN_POINT('Ctrl Pts',(0.0664853114242254,0.122360194853714,
-2.65154751291374));
#45848=CARTESIAN_POINT('Ctrl Pts',(-0.0668799556441275,0.12214493625552,
-2.64360022160579));
#45849=CARTESIAN_POINT('Ctrl Pts',(-0.116606427544758,0.0446493968714564,
-2.63811328779242));
#45850=CARTESIAN_POINT('Ctrl Pts',(-0.117958064586437,0.00283207123262861,
-2.63527545108169));
#45851=CARTESIAN_POINT('Ctrl Pts',(-0.117943238001422,4.98985662681943E-5,
-2.63508671147362));
#45852=CARTESIAN_POINT('Ctrl Pts',(-0.11792267289879,6.60661965921502E-5,
-2.67521328852638));
#45853=CARTESIAN_POINT('Ctrl Pts',(-0.117685998143791,-0.0351708055618756,
-2.67282395796953));
#45854=CARTESIAN_POINT('Ctrl Pts',(-0.0821847093582401,-0.109889137046738,
-2.66778553031004));
#45855=CARTESIAN_POINT('Ctrl Pts',(0.0449466287065965,-0.131803316363808,
-2.66009800554788));
#45856=CARTESIAN_POINT('Ctrl Pts',(0.135149441973695,-0.0335699563714237,
-2.65215071423994));
#45857=CARTESIAN_POINT('Ctrl Pts',(0.10139520486838,0.0954532663992196,
-2.64420342293198));
#45858=CARTESIAN_POINT('Ctrl Pts',(-0.0253572002932921,0.136928178363215,
-2.63625613162403));
#45859=CARTESIAN_POINT('Ctrl Pts',(-0.107791450141899,0.0699314320822719,
-2.62992608682216));
#45860=CARTESIAN_POINT('Ctrl Pts',(-0.11769772359356,0.0153847954771589,
-2.62624513912295));
#45861=CARTESIAN_POINT('Ctrl Pts',(-0.117618959460295,6.6729458887714E-5,
-2.62521328852638));
#45862=CARTESIAN_POINT('Origin',(0.,0.,-3.06008671147362));
#45863=CARTESIAN_POINT('',(-0.117581146632055,7.56075370698167E-6,-2.73508671147362));
#45864=CARTESIAN_POINT('',(-0.117821958574713,-0.000103490888977639,-2.72521328852638));
#45865=CARTESIAN_POINT('',(-0.117775,1.13296574333067E-13,-3.06008671147362));
#45866=CARTESIAN_POINT('Ctrl Pts',(-0.117581146632055,7.56075370697551E-6,
-2.73508671147362));
#45867=CARTESIAN_POINT('Ctrl Pts',(-0.117569638646798,-0.0201302688798466,
-2.73373128298016));
#45868=CARTESIAN_POINT('Ctrl Pts',(-0.103080207415897,-0.0796417091885475,
-2.72972675738406));
#45869=CARTESIAN_POINT('Ctrl Pts',(-0.00850684444458044,-0.138996214030495,
-2.72307313468531));
#45870=CARTESIAN_POINT('Ctrl Pts',(0.112256835707494,-0.0824058053669272,
-2.71512584337735));
#45871=CARTESIAN_POINT('Ctrl Pts',(0.130060222154785,0.0497659776633264,
-2.70717855206941));
#45872=CARTESIAN_POINT('Ctrl Pts',(0.02857431466928,0.136293148986501,-2.69923126076145));
#45873=CARTESIAN_POINT('Ctrl Pts',(-0.0897465865227608,0.100638692211853,
-2.69186731389619));
#45874=CARTESIAN_POINT('Ctrl Pts',(-0.117506888313243,0.0304465719673242,
-2.68715246413358));
#45875=CARTESIAN_POINT('Ctrl Pts',(-0.117789991982999,-0.000107406231871198,
-2.68508671147362));
#45876=CARTESIAN_POINT('Ctrl Pts',(-0.117821958574713,-0.000103490888977657,
-2.72521328852638));
#45877=CARTESIAN_POINT('Ctrl Pts',(-0.117891546518806,-0.00767575694883443,
-2.72470097102142));
#45878=CARTESIAN_POINT('Ctrl Pts',(-0.113773620055613,-0.0543273988107319,
-2.72153955641381));
#45879=CARTESIAN_POINT('Ctrl Pts',(-0.0515199201897912,-0.12937546699384,
-2.71572904470355));
#45880=CARTESIAN_POINT('Ctrl Pts',(0.0808804927988873,-0.113360749474457,
-2.7077817533956));
#45881=CARTESIAN_POINT('Ctrl Pts',(0.139098525352115,0.0066267549690055,
-2.69983446208764));
#45882=CARTESIAN_POINT('Ctrl Pts',(0.0697374672192116,0.120536298692083,
-2.69188717077969));
#45883=CARTESIAN_POINT('Ctrl Pts',(-0.0635857546542645,0.123891748884511,
-2.68393987947174));
#45884=CARTESIAN_POINT('Ctrl Pts',(-0.116039537486793,0.0467697666635364,
-2.67838191872063));
#45885=CARTESIAN_POINT('Ctrl Pts',(-0.117948404032311,0.00389699718071681,
-2.67547305507218));
#45886=CARTESIAN_POINT('Ctrl Pts',(-0.11792267289879,6.60661965921502E-5,
-2.67521328852638));
#45887=CARTESIAN_POINT('Origin',(0.,0.,-3.06008671147362));
#45888=CARTESIAN_POINT('',(-0.117817815448454,0.000104175268542342,-2.78508671147362));
#45889=CARTESIAN_POINT('',(-0.117581447556463,-9.82433484120193E-6,-2.77521328852638));
#45890=CARTESIAN_POINT('',(-0.117775,1.13296574333067E-13,-3.06008671147362));
#45891=CARTESIAN_POINT('Ctrl Pts',(-0.117817815448454,0.00010417526854233,
-2.78508671147362));
#45892=CARTESIAN_POINT('Ctrl Pts',(-0.117528053916134,-0.0313441947429135,
-2.7829591989294));
#45893=CARTESIAN_POINT('Ctrl Pts',(-0.088378335258817,-0.102424947763681,
-2.77818258928254));
#45894=CARTESIAN_POINT('Ctrl Pts',(0.0317395866552255,-0.135590974706457,
-2.77075688253302));
#45895=CARTESIAN_POINT('Ctrl Pts',(0.131183564369451,-0.0467245803901248,
-2.76280959122507));
#45896=CARTESIAN_POINT('Ctrl Pts',(0.110307935021035,0.0849969022889005,
-2.75486229991711));
#45897=CARTESIAN_POINT('Ctrl Pts',(-0.0117404851910752,0.138760494767705,
-2.74691500860916));
#45898=CARTESIAN_POINT('Ctrl Pts',(-0.104041614331916,0.0777915559561233,
-2.74032314579466));
#45899=CARTESIAN_POINT('Ctrl Pts',(-0.11759213025779,0.01922781337502,-2.73638038008281));
#45900=CARTESIAN_POINT('Ctrl Pts',(-0.117581146632055,7.56075370697551E-6,
-2.73508671147362));
#45901=CARTESIAN_POINT('Ctrl Pts',(-0.117581447556463,-9.82433484119326E-6,
-2.77521328852638));
#45902=CARTESIAN_POINT('Ctrl Pts',(-0.117595619370663,-0.0190922725530593,
-2.77392888697066));
#45903=CARTESIAN_POINT('Ctrl Pts',(-0.104183290718898,-0.077513766930232,
-2.76999538831228));
#45904=CARTESIAN_POINT('Ctrl Pts',(-0.0122251857505716,-0.138718630510878,
-2.76341279255126));
#45905=CARTESIAN_POINT('Ctrl Pts',(0.110010316820066,-0.0853817535458526,
-2.7554655012433));
#45906=CARTESIAN_POINT('Ctrl Pts',(0.131345999238215,0.0462659931371576,
-2.74751820993535));
#45907=CARTESIAN_POINT('Ctrl Pts',(0.0322130921955051,0.135479261605527,
-2.7395709186274));
#45908=CARTESIAN_POINT('Ctrl Pts',(-0.0881700120753839,0.102692212606021,
-2.73213594482441));
#45909=CARTESIAN_POINT('Ctrl Pts',(-0.117531720396742,0.031479001351202,
-2.72735006812407));
#45910=CARTESIAN_POINT('Ctrl Pts',(-0.117821958574713,-0.000103490888977657,
-2.72521328852638));
#45911=CARTESIAN_POINT('Origin',(0.,0.,-3.06008671147362));
#45912=CARTESIAN_POINT('',(-0.117925628517856,-6.40596713930419E-5,-2.83508671147362));
#45913=CARTESIAN_POINT('',(-0.117785807801612,0.00010769544346639,-2.82521328852638));
#45914=CARTESIAN_POINT('',(-0.117775,1.13296574333067E-13,-3.06008671147362));
#45915=CARTESIAN_POINT('Ctrl Pts',(-0.117925628517856,-6.40596713930531E-5,
-2.83508671147362));
#45916=CARTESIAN_POINT('Ctrl Pts',(-0.117949840251135,-0.00375807816172122,
-2.83483621198129));
#45917=CARTESIAN_POINT('Ctrl Pts',(-0.116115236168781,-0.0464929399061779,
-2.83193661538631));
#45918=CARTESIAN_POINT('Ctrl Pts',(-0.064018173970134,-0.123668891311378,
-2.82638792168868));
#45919=CARTESIAN_POINT('Ctrl Pts',(0.0693159272014078,-0.120779176949328,
-2.81844063038073));
#45920=CARTESIAN_POINT('Ctrl Pts',(0.139074531908459,-0.00711267889956292,
-2.81049333907277));
#45921=CARTESIAN_POINT('Ctrl Pts',(0.0812760328298283,0.113077501111085,
-2.80254604776482));
#45922=CARTESIAN_POINT('Ctrl Pts',(-0.0510676198065011,0.129554664787932,
-2.79459875645687));
#45923=CARTESIAN_POINT('Ctrl Pts',(-0.113682833675918,0.0546052015218531,
-2.78877897769313));
#45924=CARTESIAN_POINT('Ctrl Pts',(-0.117888853873725,0.00781411062496882,
-2.78560829603205));
#45925=CARTESIAN_POINT('Ctrl Pts',(-0.117817815448454,0.00010417526854233,
-2.78508671147362));
#45926=CARTESIAN_POINT('Ctrl Pts',(-0.117785807801612,0.000107695443466389,
-2.82521328852638));
#45927=CARTESIAN_POINT('Ctrl Pts',(-0.117504191843327,-0.0303119846466792,
-2.82315680291989));
#45928=CARTESIAN_POINT('Ctrl Pts',(-0.0899488852292908,-0.100369933896061,
-2.81845122021076));
#45929=CARTESIAN_POINT('Ctrl Pts',(0.0280979867448407,-0.136392139869556,
-2.81109654039897));
#45930=CARTESIAN_POINT('Ctrl Pts',(0.129885566115495,-0.0502200523954337,
-2.80314924909101));
#45931=CARTESIAN_POINT('Ctrl Pts',(0.112544041625198,0.082013123462066,
-2.79520195778306));
#45932=CARTESIAN_POINT('Ctrl Pts',(-0.00802119657383768,0.139025083726287,
-2.78725466647511));
#45933=CARTESIAN_POINT('Ctrl Pts',(-0.10293335038447,0.0799191353882865,
-2.78059177672288));
#45934=CARTESIAN_POINT('Ctrl Pts',(-0.117566389795404,0.0202655576060691,
-2.77657798407331));
#45935=CARTESIAN_POINT('Ctrl Pts',(-0.117581447556463,-9.82433484119326E-6,
-2.77521328852638));
#45936=CARTESIAN_POINT('Origin',(0.,0.,-3.06008671147362));
#45937=CARTESIAN_POINT('',(-0.117620976551725,-6.92605765801207E-5,-2.88508671147362));
#45938=CARTESIAN_POINT('',(-0.117945584131744,-4.75337169963674E-5,-2.87521328852638));
#45939=CARTESIAN_POINT('',(-0.117775,1.13296574333067E-13,-3.06008671147362));
#45940=CARTESIAN_POINT('Ctrl Pts',(-0.117620976551725,-6.92605765801272E-5,
-2.88508671147362));
#45941=CARTESIAN_POINT('Ctrl Pts',(-0.117701550786951,-0.0152483239620161,
-2.88406412793052));
#45942=CARTESIAN_POINT('Ctrl Pts',(-0.10791599027619,-0.0696504806793931,
-2.88039244728478));
#45943=CARTESIAN_POINT('Ctrl Pts',(-0.0258344786463291,-0.136840632652599,
-2.87407166953639));
#45944=CARTESIAN_POINT('Ctrl Pts',(0.101060618120367,-0.0958059291879449,
-2.86612437822844));
#45945=CARTESIAN_POINT('Ctrl Pts',(0.13526615819552,0.0330970741869585,
-2.85817708692048));
#45946=CARTESIAN_POINT('Ctrl Pts',(0.0454066843029653,0.131645762308753,
-2.85022979561253));
#45947=CARTESIAN_POINT('Ctrl Pts',(-0.081953579115799,0.11014957429056,
-2.84253300379691));
#45948=CARTESIAN_POINT('Ctrl Pts',(-0.117693794891987,0.035307125479465,
-2.83748530908394));
#45949=CARTESIAN_POINT('Ctrl Pts',(-0.117925628517856,-6.40596713930531E-5,
-2.83508671147362));
#45950=CARTESIAN_POINT('Ctrl Pts',(-0.117945584131744,-4.75337169963657E-5,
-2.87521328852638));
#45951=CARTESIAN_POINT('Ctrl Pts',(-0.117959142789025,-0.00269295294045094,
-2.87503381597178));
#45952=CARTESIAN_POINT('Ctrl Pts',(-0.116678262851619,-0.0443726330815549,
-2.87220524631453));
#45953=CARTESIAN_POINT('Ctrl Pts',(-0.0673061831817785,-0.121910832782649,
-2.86672757955463));
#45954=CARTESIAN_POINT('Ctrl Pts',(0.0660573824567498,-0.12259156477827,
-2.85878028824667));
#45955=CARTESIAN_POINT('Ctrl Pts',(0.138834266016569,-0.0108336871046625,
-2.85083299693873));
#45956=CARTESIAN_POINT('Ctrl Pts',(0.0842743478026822,0.110860972835297,
-2.84288570563077));
#45957=CARTESIAN_POINT('Ctrl Pts',(-0.0475806987781872,0.130875452878429,
-2.83493841432283));
#45958=CARTESIAN_POINT('Ctrl Pts',(-0.112968516313132,0.0567353707931715,
-2.82904760862136));
#45959=CARTESIAN_POINT('Ctrl Pts',(-0.117866960256001,0.00887364647862188,
-2.82580590002254));
#45960=CARTESIAN_POINT('Ctrl Pts',(-0.117785807801612,0.000107695443466389,
-2.82521328852638));
#45961=CARTESIAN_POINT('Origin',(0.,0.,-3.06008671147362));
#45962=CARTESIAN_POINT('',(-0.117558445841294,-3.12605290917906E-5,-2.93508671147362));
#45963=CARTESIAN_POINT('',(-0.117640397146581,-8.56657636452568E-5,-2.92521328852638));
#45964=CARTESIAN_POINT('',(-0.117775,1.13296574333067E-13,-3.06008671147362));
#45965=CARTESIAN_POINT('Ctrl Pts',(-0.117558445841294,-3.12605290917947E-5,
-2.93508671147362));
#45966=CARTESIAN_POINT('Ctrl Pts',(-0.117410007759293,-0.0266293090558454,
-2.93329204387976));
#45967=CARTESIAN_POINT('Ctrl Pts',(-0.095425295455791,-0.0925554651998461,
-2.92884827918326));
#45968=CARTESIAN_POINT('Ctrl Pts',(0.0145658909989512,-0.138586676302172,
-2.92175541738409));
#45969=CARTESIAN_POINT('Ctrl Pts',(0.12428129992797,-0.0627284744858215,
-2.91380812607615));
#45970=CARTESIAN_POINT('Ctrl Pts',(0.120090271076318,0.0704991524890691,
-2.9058608347682));
#45971=CARTESIAN_POINT('Ctrl Pts',(0.00571135947086689,0.139151690834859,
-2.89791354346024));
#45972=CARTESIAN_POINT('Ctrl Pts',(-0.0984950632345573,0.0877255235924107,
-2.89098883569539));
#45973=CARTESIAN_POINT('Ctrl Pts',(-0.117492815789671,0.0240744415048385,
-2.88671322503318));
#45974=CARTESIAN_POINT('Ctrl Pts',(-0.117620976551725,-6.92605765801272E-5,
-2.88508671147362));
#45975=CARTESIAN_POINT('Ctrl Pts',(-0.117640397146581,-8.56657636452533E-5,
-2.92521328852638));
#45976=CARTESIAN_POINT('Ctrl Pts',(-0.117731162646286,-0.0142003580566992,
-2.92426173192102));
#45977=CARTESIAN_POINT('Ctrl Pts',(-0.108844415761643,-0.0675005170391406,
-2.920661078213));
#45978=CARTESIAN_POINT('Ctrl Pts',(-0.0294856614640362,-0.136111750350814,
-2.91441132740234));
#45979=CARTESIAN_POINT('Ctrl Pts',(0.0984576432878249,-0.0984710734890703,
-2.90646403609439));
#45980=CARTESIAN_POINT('Ctrl Pts',(0.136104684613073,0.0294603972989506,
-2.89851674478643));
#45981=CARTESIAN_POINT('Ctrl Pts',(0.0489145289672211,0.130384614459911,
-2.89056945347848));
#45982=CARTESIAN_POINT('Ctrl Pts',(-0.0801550832889095,0.112136573427275,
-2.88280163472513));
#45983=CARTESIAN_POINT('Ctrl Pts',(-0.117759010797814,0.0363546463746542,
-2.87768291307443));
#45984=CARTESIAN_POINT('Ctrl Pts',(-0.117945584131744,-4.75337169963657E-5,
-2.87521328852638));
#45985=CARTESIAN_POINT('Origin',(3.28582941601228E-18,0.,-0.0136500000000002));
#45986=CARTESIAN_POINT('',(-0.00798678478681935,0.146131905375825,-0.0136500000000002));
#45987=CARTESIAN_POINT('Ctrl Pts',(0.106356886625425,-0.0510349087439493,
-0.0136500000000001));
#45988=CARTESIAN_POINT('Ctrl Pts',(0.10797749373506,-0.048506909295007,
-0.0136500000000001));
#45989=CARTESIAN_POINT('Ctrl Pts',(0.109491831180351,-0.0459180783966364,
-0.01365));
#45990=CARTESIAN_POINT('Ctrl Pts',(0.110894447333282,-0.0432730197048374,
-0.0136500000000002));
#45991=CARTESIAN_POINT('Ctrl Pts',(0.114260347727643,-0.036925592381097,
-0.0136500000000004));
#45992=CARTESIAN_POINT('Ctrl Pts',(0.116984348240791,-0.0302554581673266,
-0.0136499999999999));
#45993=CARTESIAN_POINT('Ctrl Pts',(0.119089796519242,-0.0233578112726241,
-0.0136499999999997));
#45994=CARTESIAN_POINT('Ctrl Pts',(0.120241782982297,-0.0195837951018374,
-0.0136499999999996));
#45995=CARTESIAN_POINT('Ctrl Pts',(0.121205726309446,-0.0157487895062339,
-0.0136500000000004));
#45996=CARTESIAN_POINT('Ctrl Pts',(0.121984207803306,-0.0118757879252627,
-0.0136500000000002));
#45997=CARTESIAN_POINT('Ctrl Pts',(0.123386384522449,-0.00489985761365873,
-0.0136499999999998));
#45998=CARTESIAN_POINT('Ctrl Pts',(0.124190160703931,0.00220615526225158,
-0.0136499999999999));
#45999=CARTESIAN_POINT('Ctrl Pts',(0.124410018311042,0.00935781521445493,
-0.0136499999999999));
#46000=CARTESIAN_POINT('Ctrl Pts',(0.124518362026204,0.012882084485723,
-0.0136499999999999));
#46001=CARTESIAN_POINT('Ctrl Pts',(0.124484221856685,0.0164097982231168,
-0.0136500000000001));
#46002=CARTESIAN_POINT('Ctrl Pts',(0.124310440415547,0.0199246610494899,
-0.0136500000000001));
#46003=CARTESIAN_POINT('Ctrl Pts',(0.123841403627022,0.0294112895489918,
-0.01365));
#46004=CARTESIAN_POINT('Ctrl Pts',(0.122359308962272,0.0388174407805119,
-0.0136499999999999));
#46005=CARTESIAN_POINT('Ctrl Pts',(0.119889589499077,0.0479553918623724,
-0.0136500000000002));
#46006=CARTESIAN_POINT('Ctrl Pts',(0.118986999919028,0.0512949693133307,
-0.0136500000000003));
#46007=CARTESIAN_POINT('Ctrl Pts',(0.117952005112996,0.0545988186576902,
-0.0136500000000003));
#46008=CARTESIAN_POINT('Ctrl Pts',(0.116784106418537,0.0578577665921829,
-0.0136500000000002));
#46009=CARTESIAN_POINT('Ctrl Pts',(0.115748002753435,0.0607489487771823,
-0.01365));
#46010=CARTESIAN_POINT('Ctrl Pts',(0.114608972805582,0.0635995076652492,
-0.0136500000000001));
#46011=CARTESIAN_POINT('Ctrl Pts',(0.113370868331345,0.0663963390231016,
-0.0136500000000001));
#46012=CARTESIAN_POINT('Ctrl Pts',(0.111623408852175,0.0703437841455626,
-0.01365));
#46013=CARTESIAN_POINT('Ctrl Pts',(0.109677163187892,0.074188513161514,
-0.0136500000000003));
#46014=CARTESIAN_POINT('Ctrl Pts',(0.107534292680181,0.0779135678957582,
-0.0136500000000004));
#46015=CARTESIAN_POINT('Ctrl Pts',(0.104293166260343,0.0835477736356994,
-0.0136500000000005));
#46016=CARTESIAN_POINT('Ctrl Pts',(0.100602795829931,0.0889085421797832,
-0.0136500000000002));
#46017=CARTESIAN_POINT('Ctrl Pts',(0.0965158424099242,0.0939776949692943,
-0.0136500000000003));
#46018=CARTESIAN_POINT('Ctrl Pts',(0.0944562159089865,0.0965323023625348,
-0.0136500000000003));
#46019=CARTESIAN_POINT('Ctrl Pts',(0.0922956872886706,0.0990127808204909,
-0.0136500000000004));
#46020=CARTESIAN_POINT('Ctrl Pts',(0.090040009153852,0.101416277916268,
-0.0136500000000003));
#46021=CARTESIAN_POINT('Ctrl Pts',(0.087748564367495,0.103857885521595,
-0.0136500000000002));
#46022=CARTESIAN_POINT('Ctrl Pts',(0.0853639556028889,0.10621444018175,
-0.0136500000000006));
#46023=CARTESIAN_POINT('Ctrl Pts',(0.0828986900609891,0.108478986224309,
-0.0136500000000005));
#46024=CARTESIAN_POINT('Ctrl Pts',(0.0767583099038693,0.114119422659364,
-0.0136500000000003));
#46025=CARTESIAN_POINT('Ctrl Pts',(0.0701100271741426,0.119199823308631,
-0.0136500000000007));
#46026=CARTESIAN_POINT('Ctrl Pts',(0.0630566235181073,0.123682391417081,
-0.0136500000000005));
#46027=CARTESIAN_POINT('Ctrl Pts',(0.0583782755736549,0.126655567817966,
-0.0136500000000003));
#46028=CARTESIAN_POINT('Ctrl Pts',(0.0535211481662564,0.129365518098269,
-0.0136500000000002));
#46029=CARTESIAN_POINT('Ctrl Pts',(0.0485105898935787,0.131797135777499,
-0.0136500000000002));
#46030=CARTESIAN_POINT('Ctrl Pts',(0.0456575463118391,0.133181714268642,
-0.0136500000000002));
#46031=CARTESIAN_POINT('Ctrl Pts',(0.0427550251642698,0.134475492007146,
-0.0136500000000003));
#46032=CARTESIAN_POINT('Ctrl Pts',(0.0398205425663953,0.135670768783895,
-0.0136500000000003));
#46033=CARTESIAN_POINT('Ctrl Pts',(0.0302520139346001,0.139568232708038,
-0.0136500000000002));
#46034=CARTESIAN_POINT('Ctrl Pts',(0.0203132057297043,0.142438162792591,
-0.0136500000000004));
#46035=CARTESIAN_POINT('Ctrl Pts',(0.0101716141419635,0.144199039300689,
-0.0136500000000002));
#46036=CARTESIAN_POINT('Ctrl Pts',(0.00417993901636529,0.145239369103121,
-0.01365));
#46037=CARTESIAN_POINT('Ctrl Pts',(-0.00188321839195679,0.14589189591373,
-0.0136500000000001));
#46038=CARTESIAN_POINT('Ctrl Pts',(-0.00798678478681931,0.146131905375825,
-0.0136500000000002));
#46039=CARTESIAN_POINT('',(-0.14635,-1.79227059055215E-17,-0.0136500000000001));
#46040=CARTESIAN_POINT('Origin',(0.,0.,-0.0136500000000002));
#46041=CARTESIAN_POINT('',(-0.119330942213657,0.085138415363241,-0.013650000000002));
#46042=CARTESIAN_POINT('Origin',(0.,0.,-0.0136500000000002));
#46043=CARTESIAN_POINT('Ctrl Pts',(-0.119330942213682,0.0851384153632074,
-0.0136499999999997));
#46044=CARTESIAN_POINT('Ctrl Pts',(-0.121198726066873,0.0819569309101861,
-0.0136499999999997));
#46045=CARTESIAN_POINT('Ctrl Pts',(-0.122934816712479,0.0787053437274808,
-0.0136499999999999));
#46046=CARTESIAN_POINT('Ctrl Pts',(-0.124531604043384,0.0753872965898214,
-0.0136499999999998));
#46047=CARTESIAN_POINT('Ctrl Pts',(-0.127644196141878,0.0689194801791971,
-0.0136499999999995));
#46048=CARTESIAN_POINT('Ctrl Pts',(-0.130228216974403,0.0621991413433847,
-0.0136499999999996));
#46049=CARTESIAN_POINT('Ctrl Pts',(-0.132285959409066,0.0552930525211129,
-0.0136499999999993));
#46050=CARTESIAN_POINT('Ctrl Pts',(-0.133637403415453,0.0507574059847852,
-0.0136499999999992));
#46051=CARTESIAN_POINT('Ctrl Pts',(-0.134761526400422,0.0461391411278747,
-0.0136499999999996));
#46052=CARTESIAN_POINT('Ctrl Pts',(-0.135653414685908,0.0414802748139204,
-0.0136499999999996));
#46053=CARTESIAN_POINT('Ctrl Pts',(-0.13686902110764,0.0351304349276935,
-0.0136499999999997));
#46054=CARTESIAN_POINT('Ctrl Pts',(-0.137656705017299,0.0286962406659602,
-0.0136499999999995));
#46055=CARTESIAN_POINT('Ctrl Pts',(-0.13801608155741,0.0222270992451787,
-0.0136499999999991));
#46056=CARTESIAN_POINT('Ctrl Pts',(-0.138199023739623,0.0189339548228916,
-0.0136499999999989));
#46057=CARTESIAN_POINT('Ctrl Pts',(-0.138270844463559,0.0156317713083359,
-0.0136499999999985));
#46058=CARTESIAN_POINT('Ctrl Pts',(-0.138230698014712,0.0123273216632419,
-0.0136499999999984));
#46059=CARTESIAN_POINT('Ctrl Pts',(-0.138188662178769,0.00886735678074606,
-0.0136499999999982));
#46060=CARTESIAN_POINT('Ctrl Pts',(-0.138023945600157,0.00541434562535705,
-0.0136499999999993));
#46061=CARTESIAN_POINT('Ctrl Pts',(-0.137737265449259,0.0019780480046521,
-0.0136499999999993));
#46062=CARTESIAN_POINT('Ctrl Pts',(-0.136918974928002,-0.0078304084316795,
-0.0136499999999994));
#46063=CARTESIAN_POINT('Ctrl Pts',(-0.135110265356286,-0.0175107005685719,
-0.0136499999999995));
#46064=CARTESIAN_POINT('Ctrl Pts',(-0.132295379661141,-0.0268797270541801,
-0.0136499999999994));
#46065=CARTESIAN_POINT('Ctrl Pts',(-0.131155623417163,-0.0306732759202626,
-0.0136499999999994));
#46066=CARTESIAN_POINT('Ctrl Pts',(-0.129850387617751,-0.0344155153559583,
-0.0136500000000002));
#46067=CARTESIAN_POINT('Ctrl Pts',(-0.128376581127422,-0.0380927221985045,
-0.0136500000000004));
#46068=CARTESIAN_POINT('Ctrl Pts',(-0.127294239500948,-0.0407932083620289,
-0.0136500000000005));
#46069=CARTESIAN_POINT('Ctrl Pts',(-0.126122089187759,-0.0434552743016918,
-0.0136500000000001));
#46070=CARTESIAN_POINT('Ctrl Pts',(-0.124863185252744,-0.0460663274824253,
-0.01365));
#46071=CARTESIAN_POINT('Ctrl Pts',(-0.122907807025548,-0.0501219161557532,
-0.0136499999999999));
#46072=CARTESIAN_POINT('Ctrl Pts',(-0.120741025491108,-0.0540601902277737,
-0.0136499999999991));
#46073=CARTESIAN_POINT('Ctrl Pts',(-0.118360761739933,-0.0578624096065901,
-0.0136499999999992));
#46074=CARTESIAN_POINT('Ctrl Pts',(-0.114440131085056,-0.0641252020579709,
-0.0136499999999994));
#46075=CARTESIAN_POINT('Ctrl Pts',(-0.109940665047455,-0.0700197682606754,
-0.0136499999999996));
#46076=CARTESIAN_POINT('Ctrl Pts',(-0.10493387405501,-0.075499387422339,
-0.0136499999999995));
#46077=CARTESIAN_POINT('Ctrl Pts',(-0.102913339621813,-0.077710735811688,
-0.0136499999999994));
#46078=CARTESIAN_POINT('Ctrl Pts',(-0.100808353999335,-0.0798559352178832,
-0.0136499999999995));
#46079=CARTESIAN_POINT('Ctrl Pts',(-0.0986289428089273,-0.0819258236072475,
-0.0136499999999996));
#46080=CARTESIAN_POINT('Ctrl Pts',(-0.0918665361750953,-0.088348396381554,
-0.01365));
#46081=CARTESIAN_POINT('Ctrl Pts',(-0.0844256807446546,-0.0940174328437391,
-0.0136499999999999));
#46082=CARTESIAN_POINT('Ctrl Pts',(-0.0764567779821786,-0.0988447114068085,
-0.01365));
#46083=CARTESIAN_POINT('Ctrl Pts',(-0.071808772676882,-0.101660308113164,
-0.01365));
#46084=CARTESIAN_POINT('Ctrl Pts',(-0.0669805865634173,-0.104188713709908,
-0.0136499999999998));
#46085=CARTESIAN_POINT('Ctrl Pts',(-0.0620003236069234,-0.106404393078832,
-0.0136499999999997));
#46086=CARTESIAN_POINT('Ctrl Pts',(-0.0592527274166011,-0.107626776765439,
-0.0136499999999996));
#46087=CARTESIAN_POINT('Ctrl Pts',(-0.0564585789255776,-0.108753606517434,
-0.0136499999999994));
#46088=CARTESIAN_POINT('Ctrl Pts',(-0.0536364829015093,-0.109775780828203,
-0.0136499999999995));
#46089=CARTESIAN_POINT('Ctrl Pts',(-0.0454122711661217,-0.112754622756523,
-0.0136499999999999));
#46090=CARTESIAN_POINT('Ctrl Pts',(-0.0369224943427728,-0.114861623947457,
-0.0136500000000008));
#46091=CARTESIAN_POINT('Ctrl Pts',(-0.0282900439033421,-0.115996210102783,
-0.0136500000000007));
#46092=CARTESIAN_POINT('Ctrl Pts',(-0.023506892932931,-0.116624872486418,
-0.0136500000000006));
#46093=CARTESIAN_POINT('Ctrl Pts',(-0.0186799033642427,-0.116954139727108,
-0.0136500000000002));
#46094=CARTESIAN_POINT('Ctrl Pts',(-0.0138313775859597,-0.116960008631475,
-0.0136500000000002));
#46095=CARTESIAN_POINT('Ctrl Pts',(0.103670563470606,-0.0558870726974231,
-2.95414778394209));
#46096=CARTESIAN_POINT('Ctrl Pts',(0.122275110647363,-0.0213756231646796,
-2.95149868683944));
#46097=CARTESIAN_POINT('Ctrl Pts',(0.121984618190939,0.0670884644041237,
-2.94620049263415));
#46098=CARTESIAN_POINT('Ctrl Pts',(0.00941180899824742,0.139031834987488,
-2.93825320132619));
#46099=CARTESIAN_POINT('Ctrl Pts',(-0.111685438487879,0.0831087463150725,
-2.93030591001824));
#46100=CARTESIAN_POINT('Ctrl Pts',(-0.13039962705173,-0.0488645184779689,
-2.92235861871029));
#46101=CARTESIAN_POINT('Ctrl Pts',(-0.0294856614640362,-0.136111750350814,
-2.91441132740234));
#46102=CARTESIAN_POINT('Ctrl Pts',(0.0984576432878249,-0.0984710734890703,
-2.90646403609439));
#46103=CARTESIAN_POINT('Ctrl Pts',(0.136104684613073,0.0294603972989506,
-2.89851674478643));
#46104=CARTESIAN_POINT('Ctrl Pts',(0.0489145289672211,0.130384614459911,
-2.89056945347848));
#46105=CARTESIAN_POINT('Ctrl Pts',(-0.0831371885321713,0.111714959246436,
-2.88262216217053));
#46106=CARTESIAN_POINT('Ctrl Pts',(-0.138937831621556,-0.0094142740234505,
-2.87467487086258));
#46107=CARTESIAN_POINT('Ctrl Pts',(-0.0673061831817785,-0.121910832782649,
-2.86672757955463));
#46108=CARTESIAN_POINT('Ctrl Pts',(0.0660573824567498,-0.12259156477827,
-2.85878028824667));
#46109=CARTESIAN_POINT('Ctrl Pts',(0.138834266016569,-0.0108336871046625,
-2.85083299693873));
#46110=CARTESIAN_POINT('Ctrl Pts',(0.0842743478026822,0.110860972835297,
-2.84288570563077));
#46111=CARTESIAN_POINT('Ctrl Pts',(-0.0475806987781872,0.130875452878429,
-2.83493841432283));
#46112=CARTESIAN_POINT('Ctrl Pts',(-0.135795462645268,0.030853000978399,
-2.82699112301486));
#46113=CARTESIAN_POINT('Ctrl Pts',(-0.0994606430770848,-0.0974674046326144,
-2.81904383170692));
#46114=CARTESIAN_POINT('Ctrl Pts',(0.0280979867448407,-0.136392139869556,
-2.81109654039897));
#46115=CARTESIAN_POINT('Ctrl Pts',(0.129885566115495,-0.0502200523954337,
-2.80314924909101));
#46116=CARTESIAN_POINT('Ctrl Pts',(0.112544041625198,0.082013123462066,
-2.79520195778306));
#46117=CARTESIAN_POINT('Ctrl Pts',(-0.00802119657383768,0.139025083726287,
-2.78725466647511));
#46118=CARTESIAN_POINT('Ctrl Pts',(-0.121229513542639,0.0685253145656341,
-2.77930737516716));
#46119=CARTESIAN_POINT('Ctrl Pts',(-0.123247930400552,-0.0648248509142736,
-2.77136008385921));
#46120=CARTESIAN_POINT('Ctrl Pts',(-0.0122251857505716,-0.138718630510878,
-2.76341279255126));
#46121=CARTESIAN_POINT('Ctrl Pts',(0.110010316820066,-0.0853817535458526,
-2.7554655012433));
#46122=CARTESIAN_POINT('Ctrl Pts',(0.131345999238215,0.0462659931371576,
-2.74751820993535));
#46123=CARTESIAN_POINT('Ctrl Pts',(0.0322130921955051,0.135479261605527,
-2.7395709186274));
#46124=CARTESIAN_POINT('Ctrl Pts',(-0.0964651820724651,0.100432974095761,
-2.73162362731945));
#46125=CARTESIAN_POINT('Ctrl Pts',(-0.136667031580617,-0.0267289377911359,
-2.7236763360115));
#46126=CARTESIAN_POINT('Ctrl Pts',(-0.0515199201897912,-0.12937546699384,
-2.71572904470355));
#46127=CARTESIAN_POINT('Ctrl Pts',(0.0808804927988873,-0.113360749474457,
-2.7077817533956));
#46128=CARTESIAN_POINT('Ctrl Pts',(0.139098525352115,0.0066267549690055,
-2.69983446208764));
#46129=CARTESIAN_POINT('Ctrl Pts',(0.0697374672192116,0.120536298692083,
-2.69188717077969));
#46130=CARTESIAN_POINT('Ctrl Pts',(-0.0635857546542645,0.123891748884511,
-2.68393987947174));
#46131=CARTESIAN_POINT('Ctrl Pts',(-0.138589071705656,0.0136155367260933,
-2.67599258816378));
#46132=CARTESIAN_POINT('Ctrl Pts',(-0.0864805613488348,-0.109148642434832,
-2.66804529685584));
#46133=CARTESIAN_POINT('Ctrl Pts',(0.0449466287065965,-0.131803316363808,
-2.66009800554788));
#46134=CARTESIAN_POINT('Ctrl Pts',(0.135149441973695,-0.0335699563714237,
-2.65215071423994));
#46135=CARTESIAN_POINT('Ctrl Pts',(0.10139520486838,0.0954532663992196,
-2.64420342293198));
#46136=CARTESIAN_POINT('Ctrl Pts',(-0.0253572002932921,0.136928178363215,
-2.63625613162403));
#46137=CARTESIAN_POINT('Ctrl Pts',(-0.128852359933585,0.05281460949517,
-2.62830884031608));
#46138=CARTESIAN_POINT('Ctrl Pts',(-0.114166058832061,-0.0797397306700743,
-2.62036154900813));
#46139=CARTESIAN_POINT('Ctrl Pts',(0.00523164691012173,-0.139157980393471,
-2.61241425770018));
#46140=CARTESIAN_POINT('Ctrl Pts',(0.119830964215785,-0.0709426081540357,
-2.60446696639222));
#46141=CARTESIAN_POINT('Ctrl Pts',(0.12452311024091,0.0623402650981849,
-2.59651967508427));
#46142=CARTESIAN_POINT('Ctrl Pts',(0.0150045187058493,0.138445577953893,
-2.58857238377632));
#46143=CARTESIAN_POINT('Ctrl Pts',(-0.108275993366011,0.0875706737280534,
-2.58062509246837));
#46144=CARTESIAN_POINT('Ctrl Pts',(-0.132247380902922,-0.0436227449950054,
-2.57267780116042));
#46145=CARTESIAN_POINT('Ctrl Pts',(-0.0349234451532213,-0.134806033304195,
-2.56473050985246));
#46146=CARTESIAN_POINT('Ctrl Pts',(0.0944317530776,-0.102347240545473,-2.55678321854452));
#46147=CARTESIAN_POINT('Ctrl Pts',(0.137175557268965,0.0239829131785638,
-2.54883592723656));
#46148=CARTESIAN_POINT('Ctrl Pts',(0.0541039883893578,0.128316297004496,
-2.54088863592861));
#46149=CARTESIAN_POINT('Ctrl Pts',(-0.0785909508585415,0.114959889003652,
-2.53294134462066));
#46150=CARTESIAN_POINT('Ctrl Pts',(-0.139203443356235,-0.00383601281920323,
-2.52499405331271));
#46151=CARTESIAN_POINT('Ctrl Pts',(-0.0721406159404224,-0.119113580956658,
-2.51704676200475));
#46152=CARTESIAN_POINT('Ctrl Pts',(0.0610885073433754,-0.125141951028183,
-2.50909947069681));
#46153=CARTESIAN_POINT('Ctrl Pts',(0.1382881637544,-0.0163919920088414,
-2.50115217938885));
#46154=CARTESIAN_POINT('Ctrl Pts',(0.0886519810374287,0.107392457345575,
-2.4932048880809));
#46155=CARTESIAN_POINT('Ctrl Pts',(-0.0422944750968055,0.132678148211631,
-2.48525759677295));
#46156=CARTESIAN_POINT('Ctrl Pts',(-0.134449070136487,0.0362734224469619,
-2.477310305465));
#46157=CARTESIAN_POINT('Ctrl Pts',(-0.103288985396153,-0.0934007448172382,
-2.46936301415705));
#46158=CARTESIAN_POINT('Ctrl Pts',(0.0226062146261162,-0.137409143425246,
-2.46141572284909));
#46159=CARTESIAN_POINT('Ctrl Pts',(0.127767332108225,-0.0553879272272235,
-2.45346843154115));
#46160=CARTESIAN_POINT('Ctrl Pts',(0.115742160170272,0.0774342688717387,
-2.44552114023319));
#46161=CARTESIAN_POINT('Ctrl Pts',(-0.00243999302426519,0.139234909669319,
-2.43757384892524));
#46162=CARTESIAN_POINT('Ctrl Pts',(-0.118384221046488,0.0733313701208286,
-2.42962655761729));
#46163=CARTESIAN_POINT('Ctrl Pts',(-0.125748209022913,-0.0598306072517374,
-2.42167926630934));
#46164=CARTESIAN_POINT('Ctrl Pts',(-0.0177778171272468,-0.138116844934903,
-2.41373197500138));
#46165=CARTESIAN_POINT('Ctrl Pts',(0.106498123211473,-0.0897243745534934,
-2.40578468369343));
#46166=CARTESIAN_POINT('Ctrl Pts',(0.133095574977059,0.0409619525670818,
-2.39783739238548));
#46167=CARTESIAN_POINT('Ctrl Pts',(0.0376197525149271,0.134078588362562,
-2.38989010107753));
#46168=CARTESIAN_POINT('Ctrl Pts',(-0.09236034528412,0.104220344729711,
-2.38194280976958));
#46169=CARTESIAN_POINT('Ctrl Pts',(-0.137628913345395,-0.0212272430604503,
-2.37399551846163));
#46170=CARTESIAN_POINT('Ctrl Pts',(-0.0566662969110845,-0.127205520442183,
-2.36604822715368));
#46171=CARTESIAN_POINT('Ctrl Pts',(0.0762698010119113,-0.116512793675996,
-2.35810093584572));
#46172=CARTESIAN_POINT('Ctrl Pts',(0.13925237616884,0.00104372789252618,
-2.35015364453777));
#46173=CARTESIAN_POINT('Ctrl Pts',(0.0745147509671164,0.117642957821071,
-2.34220635322982));
#46174=CARTESIAN_POINT('Ctrl Pts',(-0.0585666913028059,0.126341823266975,
-2.33425906192187));
#46175=CARTESIAN_POINT('Ctrl Pts',(-0.137931638721192,0.0191618547189039,
-2.32631177061392));
#46176=CARTESIAN_POINT('Ctrl Pts',(-0.0907877464490561,-0.105593080887356,
-2.31836447930597));
#46177=CARTESIAN_POINT('Ctrl Pts',(0.0396253113885193,-0.133499619227714,
-2.31041718799801));
#46178=CARTESIAN_POINT('Ctrl Pts',(0.13369462523368,-0.0389622999861087,
-2.30246989669006));
#46179=CARTESIAN_POINT('Ctrl Pts',(0.105141224899681,0.0913106590885011,
-2.29452260538211));
#46180=CARTESIAN_POINT('Ctrl Pts',(-0.0198461371346163,0.137834844931954,
-2.28657531407416));
#46181=CARTESIAN_POINT('Ctrl Pts',(-0.126630918495495,0.0579389689032257,
-2.27862802276621));
#46182=CARTESIAN_POINT('Ctrl Pts',(-0.117271712035045,-0.0750976643641544,
-2.27068073145826));
#46183=CARTESIAN_POINT('Ctrl Pts',(-0.00035264218412894,-0.139255841098576,
-2.2627334401503));
#46184=CARTESIAN_POINT('Ctrl Pts',(0.116889865813058,-0.0756906394925223,
-2.25478614884235));
#46185=CARTESIAN_POINT('Ctrl Pts',(0.126922734073552,0.0572968865810018,
-2.2468388575344));
#46186=CARTESIAN_POINT('Ctrl Pts',(0.020543965621383,0.137732563735411,
-2.23889156622645));
#46187=CARTESIAN_POINT('Ctrl Pts',(-0.10467742137356,0.0918419898040323,
-2.2309442749185));
#46188=CARTESIAN_POINT('Ctrl Pts',(-0.133890240337692,-0.0382846859579246,
-2.22299698361055));
#46189=CARTESIAN_POINT('Ctrl Pts',(-0.0403009298698327,-0.133297219356626,
-2.2150496923026));
#46190=CARTESIAN_POINT('Ctrl Pts',(0.0902517917743938,-0.106051533313259,
-2.20710240099464));
#46191=CARTESIAN_POINT('Ctrl Pts',(0.13802691747888,0.0184630357162695,
-2.19915510968669));
#46192=CARTESIAN_POINT('Ctrl Pts',(0.059205815238823,0.12604358404333,-2.19120781837874));
#46193=CARTESIAN_POINT('Ctrl Pts',(-0.0739179767846482,0.118018838939578,
-2.18326052707079));
#46194=CARTESIAN_POINT('Ctrl Pts',(-0.139245304110133,0.00174897680326264,
-2.17531323576284));
#46195=CARTESIAN_POINT('Ctrl Pts',(-0.0768589174636237,-0.116125020744462,
-2.16736594445488));
#46196=CARTESIAN_POINT('Ctrl Pts',(0.0560213207628474,-0.127490883033133,
-2.15941865314694));
#46197=CARTESIAN_POINT('Ctrl Pts',(0.137519639994184,-0.0219240108659811,
-2.15147136183898));
#46198=CARTESIAN_POINT('Ctrl Pts',(0.0928869986161953,0.103751236737962,
-2.14352407053103));
#46199=CARTESIAN_POINT('Ctrl Pts',(-0.0369402110727147,0.134267399030759,
-2.13557677922308));
#46200=CARTESIAN_POINT('Ctrl Pts',(-0.132886410689829,0.0416355075693321,
-2.12762948791513));
#46201=CARTESIAN_POINT('Ctrl Pts',(-0.106951178440612,-0.0891838498089545,
-2.11968219660718));
#46202=CARTESIAN_POINT('Ctrl Pts',(0.0170780778737081,-0.138205111673633,
-2.11173490529922));
#46203=CARTESIAN_POINT('Ctrl Pts',(0.125443576141085,-0.0604667085388119,
-2.10378761399128));
#46204=CARTESIAN_POINT('Ctrl Pts',(0.118754099267359,0.0727308568888059,
-2.09584032268332));
#46205=CARTESIAN_POINT('Ctrl Pts',(0.00314513556600165,0.139220766262987,
-2.08789303137537));
#46206=CARTESIAN_POINT('Ctrl Pts',(-0.115348499519044,0.0780194674122224,
-2.07994574006742));
#46207=CARTESIAN_POINT('Ctrl Pts',(-0.128046213019386,-0.0547401221041357,
-2.07199844875947));
#46208=CARTESIAN_POINT('Ctrl Pts',(-0.0233018516916921,-0.1372928889066,
-2.06405115745151));
#46209=CARTESIAN_POINT('Ctrl Pts',(0.102814620106721,-0.0939226678118359,
-2.05610386614357));
#46210=CARTESIAN_POINT('Ctrl Pts',(0.134631057384304,0.035592021917362,
-2.04815657483561));
#46211=CARTESIAN_POINT('Ctrl Pts',(0.0429658988952774,0.132462240539342,
-2.04020928352766));
#46212=CARTESIAN_POINT('Ctrl Pts',(-0.0881069405717808,0.10784006982408,
-2.03226199221971));
#46213=CARTESIAN_POINT('Ctrl Pts',(-0.138369409599115,-0.0156914028618916,
-2.02431470091176));
#46214=CARTESIAN_POINT('Ctrl Pts',(-0.0617215220226959,-0.124830955118446,
-2.0163674096038));
#46215=CARTESIAN_POINT('Ctrl Pts',(0.0715364240393441,-0.11947741908932,
-2.00842011829585));
#46216=CARTESIAN_POINT('Ctrl Pts',(0.139182230024373,-0.00454097809115471,
-2.0004728269879));
#46217=CARTESIAN_POINT('Ctrl Pts',(0.0791721726471583,0.114560380214585,
-1.99252553567995));
#46218=CARTESIAN_POINT('Ctrl Pts',(-0.0534534194270322,0.128588668194905,
-1.984578244372));
#46219=CARTESIAN_POINT('Ctrl Pts',(-0.137052333272063,0.02467734955916,
-1.97663095306404));
#46220=CARTESIAN_POINT('Ctrl Pts',(-0.0949488932563241,-0.101867665654913,
-1.9686836617561));
#46221=CARTESIAN_POINT('Ctrl Pts',(0.0342402540498007,-0.13498117883315,
-1.96073637044814));
#46222=CARTESIAN_POINT('Ctrl Pts',(0.132024751554693,-0.0442919700792729,
-1.95278907914019));
#46223=CARTESIAN_POINT('Ctrl Pts',(0.108718118087273,0.0870211723441102,
-1.94484178783224));
#46224=CARTESIAN_POINT('Ctrl Pts',(-0.0143031501084346,0.138519794735472,
-1.93689449652429));
#46225=CARTESIAN_POINT('Ctrl Pts',(-0.12420578257333,0.0629701295212927,
-1.92894720521634));
#46226=CARTESIAN_POINT('Ctrl Pts',(-0.120188725676985,-0.0703347983342829,
-1.92099991390838));
#46227=CARTESIAN_POINT('Ctrl Pts',(-0.00593636402933215,-0.139129699269039,
-1.91305262260043));
#46228=CARTESIAN_POINT('Ctrl Pts',(0.113760742075024,-0.0803169172660493,
-1.90510533129248));
#46229=CARTESIAN_POINT('Ctrl Pts',(0.129118194016824,0.052161342107116,
-1.89715803998453));
#46230=CARTESIAN_POINT('Ctrl Pts',(0.0260503661646103,0.136797997277999,
-1.88921074867658));
#46231=CARTESIAN_POINT('Ctrl Pts',(-0.10091046859706,0.0959655717645845,
-1.88126345736863));
#46232=CARTESIAN_POINT('Ctrl Pts',(-0.135317728173232,-0.0328850433877962,
-1.87331616606068));
#46233=CARTESIAN_POINT('Ctrl Pts',(-0.0456135877873082,-0.131573987724592,
-1.86536887475272));
#46234=CARTESIAN_POINT('Ctrl Pts',(0.085926654297937,-0.109585234944059,
-1.85742158344477));
#46235=CARTESIAN_POINT('Ctrl Pts',(0.138656251961757,0.0129134591995952,
-1.84947429213682));
#46236=CARTESIAN_POINT('Ctrl Pts',(0.0642124054894162,0.123568121365685,
-1.84152700082887));
#46237=CARTESIAN_POINT('Ctrl Pts',(-0.0691261005948764,0.120887947509786,
-1.83357970952092));
#46238=CARTESIAN_POINT('Ctrl Pts',(-0.139063179278854,0.00733115307704587,
-1.82563241821296));
#46239=CARTESIAN_POINT('Ctrl Pts',(-0.0814535861669311,-0.112949665502506,
-1.81768512690502));
#46240=CARTESIAN_POINT('Ctrl Pts',(0.0508640200603842,-0.129634737242294,
-1.80973783559706));
#46241=CARTESIAN_POINT('Ctrl Pts',(0.136529906497424,-0.0274207634537505,
-1.80179054428911));
#46242=CARTESIAN_POINT('Ctrl Pts',(0.0969726011114629,0.0999431251775667,
-1.79384325298116));
#46243=CARTESIAN_POINT('Ctrl Pts',(-0.0315265261952861,0.13564067156513,
-1.78589596167321));
#46244=CARTESIAN_POINT('Ctrl Pts',(-0.131109994372513,0.0469306191331561,
-1.77794867036525));
#46245=CARTESIAN_POINT('Ctrl Pts',(-0.110441333207432,-0.0848234964850357,
-1.77000137905731));
#46246=CARTESIAN_POINT('Ctrl Pts',(0.0115224698662327,-0.138778767557446,
-1.76205408774935));
#46247=CARTESIAN_POINT('Ctrl Pts',(0.122918035611167,-0.0654482250185099,
-1.7541067964414));
#46248=CARTESIAN_POINT('Ctrl Pts',(0.121575014282259,0.06791045235345,-1.74615950513345));
#46249=CARTESIAN_POINT('Ctrl Pts',(0.00872520499083007,0.138982676742282,
-1.7382122138255));
#46250=CARTESIAN_POINT('Ctrl Pts',(-0.112127232049285,0.0825820650598395,
-1.73026492251755));
#46251=CARTESIAN_POINT('Ctrl Pts',(-0.130138245933848,-0.0495615837301763,
-1.7223176312096));
#46252=CARTESIAN_POINT('Ctrl Pts',(-0.0287884036356622,-0.136248087886369,
-1.71437033990164));
#46253=CARTESIAN_POINT('Ctrl Pts',(0.0989657326610272,-0.0979698800420198,
-1.70642304859369));
#46254=CARTESIAN_POINT('Ctrl Pts',(0.135949976537486,0.0301648390686699,
-1.69847575728574));
#46255=CARTESIAN_POINT('Ctrl Pts',(0.0482429316917392,0.130632818152132,
-1.69052846597779));
#46256=CARTESIAN_POINT('Ctrl Pts',(-0.0837118098258903,0.111286326798289,
-1.68258117466984));
#46257=CARTESIAN_POINT('Ctrl Pts',(-0.138887329203821,-0.0101303219697604,
-1.67463388336189));
#46258=CARTESIAN_POINT('Ctrl Pts',(-0.0666774638491984,-0.122255590674703,
-1.66668659205393));
#46259=CARTESIAN_POINT('Ctrl Pts',(0.0666879758411977,-0.122249856911105,
-1.65873930074598));
#46260=CARTESIAN_POINT('Ctrl Pts',(0.138888199753706,-0.0101183796013297,
-1.65079200943803));
#46261=CARTESIAN_POINT('Ctrl Pts',(0.0837022404783003,0.111293524409529,
-1.64284471813008));
#46262=CARTESIAN_POINT('Ctrl Pts',(-0.0482541640740641,0.130628669464612,
-1.63489742682213));
#46263=CARTESIAN_POINT('Ctrl Pts',(-0.135952569781179,0.030153149196646,
-1.62695013551418));
#46264=CARTESIAN_POINT('Ctrl Pts',(-0.0989573082816934,-0.097978389322461,
-1.61900284420623));
#46265=CARTESIAN_POINT('Ctrl Pts',(0.0288001189230785,-0.136245611990252,
-1.61105555289827));
#46266=CARTESIAN_POINT('Ctrl Pts',(0.130142507042637,-0.0495503935124521,
-1.60310826159032));
#46267=CARTESIAN_POINT('Ctrl Pts',(0.112120130754087,0.0825917060985434,
-1.59516097028237));
#46268=CARTESIAN_POINT('Ctrl Pts',(-0.00873715548808248,0.138981925985211,
-1.58721367897442));
#46269=CARTESIAN_POINT('Ctrl Pts',(-0.121580853163911,0.0678999983837808,
-1.57926638766647));
#46270=CARTESIAN_POINT('Ctrl Pts',(-0.122912407542141,-0.0654587939758788,
-1.57131909635852));
#46271=CARTESIAN_POINT('Ctrl Pts',(-0.0115105368274101,-0.138779757812609,
-1.56337180505056));
#46272=CARTESIAN_POINT('Ctrl Pts',(0.110448626411003,-0.0848139997907445,
-1.55542451374261));
#46273=CARTESIAN_POINT('Ctrl Pts',(0.131105958523409,0.0469418925506857,
-1.54747722243466));
#46274=CARTESIAN_POINT('Ctrl Pts',(0.0315148629140466,0.135643381895656,
-1.53952993112671));
#46275=CARTESIAN_POINT('Ctrl Pts',(-0.0969811944374197,0.0999347865463928,
-1.53158263981876));
#46276=CARTESIAN_POINT('Ctrl Pts',(-0.136527548197828,-0.0274325029786067,
-1.5236353485108));
#46277=CARTESIAN_POINT('Ctrl Pts',(-0.0508528731324187,-0.129639110343907,
-1.51568805720286));
#46278=CARTESIAN_POINT('Ctrl Pts',(0.0814632979273637,-0.112942661237371,
-1.5077407658949));
#46279=CARTESIAN_POINT('Ctrl Pts',(0.139062548390083,0.0073431105015257,
-1.49979347458695));
#46280=CARTESIAN_POINT('Ctrl Pts',(0.0691157056986611,0.120893890922402,
-1.491846183279));
#46281=CARTESIAN_POINT('Ctrl Pts',(-0.0642230303494631,0.123562599557122,
-1.48389889197105));
#46282=CARTESIAN_POINT('Ctrl Pts',(-0.138657361822632,0.0129015366902274,
-1.4759516006631));
#46283=CARTESIAN_POINT('Ctrl Pts',(-0.0859172312118186,-0.109592623006646,
-1.46800430935514));
#46284=CARTESIAN_POINT('Ctrl Pts',(0.045624901106524,-0.131570065119699,
-1.46005701804719));
#46285=CARTESIAN_POINT('Ctrl Pts',(0.135320555318067,-0.0328734078700636,
-1.45210972673924));
#46286=CARTESIAN_POINT('Ctrl Pts',(0.100902216552484,0.0959742482720097,
-1.44416243543129));
#46287=CARTESIAN_POINT('Ctrl Pts',(-0.0260621287465163,0.13679575681205,
-1.43621514412334));
#46288=CARTESIAN_POINT('Ctrl Pts',(-0.129122678671555,0.052150239589711,
-1.42826785281539));
#46289=CARTESIAN_POINT('Ctrl Pts',(-0.113753835544216,-0.0803266987717117,
-1.42032056150743));
#46290=CARTESIAN_POINT('Ctrl Pts',(0.0059483271787393,-0.139129188312001,
-1.41237327019948));
#46291=CARTESIAN_POINT('Ctrl Pts',(0.120194773022965,-0.0703244635567145,
-1.40442597889153));
#46292=CARTESIAN_POINT('Ctrl Pts',(0.12420036758044,0.0629808092157078,
-1.39647868758358));
#46293=CARTESIAN_POINT('Ctrl Pts',(0.0142912393273046,0.138521024090466,
-1.38853139627563));
#46294=CARTESIAN_POINT('Ctrl Pts',(-0.108725600266021,0.0870118238136351,
-1.38058410496768));
#46295=CARTESIAN_POINT('Ctrl Pts',(-0.13202094258842,-0.0443033221626407,
-1.37263681365972));
#46296=CARTESIAN_POINT('Ctrl Pts',(-0.0342286474655051,-0.134984122508034,
-1.36468952235177));
#46297=CARTESIAN_POINT('Ctrl Pts',(0.0949576520728147,-0.10185950102666,
-1.35674223104382));
#46298=CARTESIAN_POINT('Ctrl Pts',(0.137050210865036,0.0246891340154153,
-1.34879493973587));
#46299=CARTESIAN_POINT('Ctrl Pts',(0.0534423624365219,0.12859326395183,
-1.34084764842792));
#46300=CARTESIAN_POINT('Ctrl Pts',(-0.0791820229145371,0.114553572112542,
-1.33290035711997));
#46301=CARTESIAN_POINT('Ctrl Pts',(-0.139181839050446,-0.00455294576261637,
-1.32495306581201));
#46302=CARTESIAN_POINT('Ctrl Pts',(-0.0715261504195623,-0.119483569760616,
-1.31700577450407));
#46303=CARTESIAN_POINT('Ctrl Pts',(0.0617322554776575,-0.124825647485695,
-1.30905848319611));
#46304=CARTESIAN_POINT('Ctrl Pts',(0.138370758324617,-0.0156795050066074,
-1.30111119188816));
#46305=CARTESIAN_POINT('Ctrl Pts',(0.0880976675369301,0.107847645366666,
-1.29316390058021));
#46306=CARTESIAN_POINT('Ctrl Pts',(-0.0429772886013641,0.132458545594676,
-1.28521660927226));
#46307=CARTESIAN_POINT('Ctrl Pts',(-0.134634117293255,0.0355804454335238,
-1.27726931796431));
#46308=CARTESIAN_POINT('Ctrl Pts',(-0.10280654371573,-0.0939315080567081,
-1.26932202665635));
#46309=CARTESIAN_POINT('Ctrl Pts',(0.0233136568373885,-0.137290884771896,
-1.2613747353484));
#46310=CARTESIAN_POINT('Ctrl Pts',(0.128050919416408,-0.0547291117522856,
-1.25342744404045));
#46311=CARTESIAN_POINT('Ctrl Pts',(0.115341790530312,0.0780293854508893,
-1.2454801527325));
#46312=CARTESIAN_POINT('Ctrl Pts',(-0.003157106556191,0.139220495311483,
-1.23753286142455));
#46313=CARTESIAN_POINT('Ctrl Pts',(-0.118760352645532,0.0727206454598038,
-1.2295855701166));
#46314=CARTESIAN_POINT('Ctrl Pts',(-0.125438376402145,-0.0604774946750888,
-1.22163827880865));
#46315=CARTESIAN_POINT('Ctrl Pts',(-0.01706619414058,-0.138206579634031,
-1.21369098750069));
#46316=CARTESIAN_POINT('Ctrl Pts',(0.106958846585331,-0.0891746532021148,
-1.20574369619274));
#46317=CARTESIAN_POINT('Ctrl Pts',(0.132882830138289,0.0416469337529245,
-1.19779640488479));
#46318=CARTESIAN_POINT('Ctrl Pts',(0.036928665853329,0.134270574866107,
-1.18984911357684));
#46319=CARTESIAN_POINT('Ctrl Pts',(-0.0928959194005778,0.103743249396301,
-1.18190182226889));
#46320=CARTESIAN_POINT('Ctrl Pts',(-0.137517754333317,-0.0219358355141317,
-1.17395453096093));
#46321=CARTESIAN_POINT('Ctrl Pts',(-0.0560103581567255,-0.127495699597034,
-1.16600723965299));
#46322=CARTESIAN_POINT('Ctrl Pts',(0.0768689022763401,-0.116118411543615,
-1.15805994834503));
#46323=CARTESIAN_POINT('Ctrl Pts',(0.139245153208294,0.00176094990851802,
-1.15011265703708));
#46324=CARTESIAN_POINT('Ctrl Pts',(0.0739078285731691,0.118025194395861,
-1.14216536572913));
#46325=CARTESIAN_POINT('Ctrl Pts',(-0.0592166529718895,0.126038492721028,
-1.13421807442118));
#46326=CARTESIAN_POINT('Ctrl Pts',(-0.138028504526574,0.0184511673001812,
-1.12627078311322));
#46327=CARTESIAN_POINT('Ctrl Pts',(-0.0902426725202642,-0.106059293289094,
-1.11832349180528));
#46328=CARTESIAN_POINT('Ctrl Pts',(0.0403123913820496,-0.13329375355823,
-1.11037620049732));
#46329=CARTESIAN_POINT('Ctrl Pts',(0.133893531780113,-0.0382731731638424,
-1.10242890918937));
#46330=CARTESIAN_POINT('Ctrl Pts',(0.10466952388434,0.0918509902309573,
-1.09448161788142));
#46331=CARTESIAN_POINT('Ctrl Pts',(-0.0205558085830443,0.137730796737981,
-1.08653432657347));
#46332=CARTESIAN_POINT('Ctrl Pts',(-0.126927660320036,0.0572859728228762,
-1.07858703526552));
#46333=CARTESIAN_POINT('Ctrl Pts',(-0.116883357064639,-0.0757006900753334,
-1.07063974395756));
#46334=CARTESIAN_POINT('Ctrl Pts',(0.00036461620057585,-0.139255810261576,
-1.06269245264961));
#46335=CARTESIAN_POINT('Ctrl Pts',(0.117278168930411,-0.0750875803905805,
-1.05474516134166));
#46336=CARTESIAN_POINT('Ctrl Pts',(0.126625936101752,0.0579498571433683,
-1.04679787003371));
#46337=CARTESIAN_POINT('Ctrl Pts',(0.0198342852289171,0.137836550907369,
-1.03885057872576));
#46338=CARTESIAN_POINT('Ctrl Pts',(-0.105149075926379,0.0913016181040087,
-1.03090328741781));
#46339=CARTESIAN_POINT('Ctrl Pts',(-0.133691274536908,-0.0389737956745147,
-1.02295599610985));
#46340=CARTESIAN_POINT('Ctrl Pts',(-0.0396138321773288,-0.133503025946263,
-1.0150087048019));
#46341=CARTESIAN_POINT('Ctrl Pts',(0.0907968256135503,-0.105585274044654,
-1.00706141349395));
#46342=CARTESIAN_POINT('Ctrl Pts',(0.137929990564865,0.0191737148032896,
-0.999114122186));
#46343=CARTESIAN_POINT('Ctrl Pts',(0.0585558274900352,0.126346858700717,
-0.991166830878047));
#46344=CARTESIAN_POINT('Ctrl Pts',(-0.0745248663094564,0.117636550179523,
-0.983219539570098));
#46345=CARTESIAN_POINT('Ctrl Pts',(-0.139252465399779,0.00103175416884905,
-0.975272248262143));
#46346=CARTESIAN_POINT('Ctrl Pts',(-0.0762597822901658,-0.116519351361215,
-0.967324956954194));
#46347=CARTESIAN_POINT('Ctrl Pts',(0.0566772345635106,-0.127200647477969,
-0.959377665646241));
#46348=CARTESIAN_POINT('Ctrl Pts',(0.137630738076998,-0.0212154088568283,
-0.95143037433829));
#46349=CARTESIAN_POINT('Ctrl Pts',(0.0923513834783183,0.104228286017869,
-0.943483083030339));
#46350=CARTESIAN_POINT('Ctrl Pts',(-0.0376312812236582,0.13407535310432,
-0.935535791722386));
#46351=CARTESIAN_POINT('Ctrl Pts',(-0.133099096629194,0.0409505080929924,
-0.927588500414435));
#46352=CARTESIAN_POINT('Ctrl Pts',(-0.106490407800252,-0.0897335315426603,
-0.919641209106483));
#46353=CARTESIAN_POINT('Ctrl Pts',(0.017789693141843,-0.1381153157854,-0.911693917798532));
#46354=CARTESIAN_POINT('Ctrl Pts',(0.125753353137608,-0.0598197944766599,
-0.90374662649058));
#46355=CARTESIAN_POINT('Ctrl Pts',(0.118377915156088,0.0733415492056153,
-0.895799335182628));
#46356=CARTESIAN_POINT('Ctrl Pts',(0.00242802079729554,0.139235118959227,
-0.887852043874677));
#46357=CARTESIAN_POINT('Ctrl Pts',(-0.115748817985984,0.0774243164091847,
-0.879904752566726));
#46358=CARTESIAN_POINT('Ctrl Pts',(-0.127762569063506,-0.0553989131921782,
-0.871957461258773));
#46359=CARTESIAN_POINT('Ctrl Pts',(-0.0225943993144704,-0.137411086729565,
-0.864010169950823));
#46360=CARTESIAN_POINT('Ctrl Pts',(0.103297016147289,-0.0933918630912153,
-0.856062878642869));
#46361=CARTESIAN_POINT('Ctrl Pts',(0.134445950642072,0.0362849830168238,
-0.848115587334919));
#46362=CARTESIAN_POINT('Ctrl Pts',(0.0422830665105441,0.132681784443256,
-0.840168296026967));
#46363=CARTESIAN_POINT('Ctrl Pts',(-0.0886612149305494,0.107384834141608,
-0.832221004719016));
#46364=CARTESIAN_POINT('Ctrl Pts',(-0.138286753765475,-0.0164038827595369,
-0.824273713411065));
#46365=CARTESIAN_POINT('Ctrl Pts',(-0.0610777466931965,-0.1251472033066,
-0.816326422103112));
#46366=CARTESIAN_POINT('Ctrl Pts',(0.0721508577441712,-0.119107377451451,
-0.808379130795161));
#46367=CARTESIAN_POINT('Ctrl Pts',(0.139203772684067,-0.00382404329272468,
-0.800431839487209));
#46368=CARTESIAN_POINT('Ctrl Pts',(0.0785810656558809,0.114966646280423,
-0.792484548179258));
#46369=CARTESIAN_POINT('Ctrl Pts',(-0.0541150215622158,0.12831164435819,
-0.784537256871306));
#46370=CARTESIAN_POINT('Ctrl Pts',(-0.137177618950604,0.0239711179469101,
-0.776589965563354));
#46371=CARTESIAN_POINT('Ctrl Pts',(-0.0944229523244023,-0.102355359952107,
-0.768642674255403));
#46372=CARTESIAN_POINT('Ctrl Pts',(0.0349350364218175,-0.134803029887269,
-0.760695382947452));
#46373=CARTESIAN_POINT('Ctrl Pts',(0.132251131348421,-0.0436113734436843,
-0.752748091639499));
#46374=CARTESIAN_POINT('Ctrl Pts',(0.108268463135797,0.087579983596677,
-0.744800800331548));
#46375=CARTESIAN_POINT('Ctrl Pts',(-0.0150164229970535,0.138444287267318,
-0.736853509023596));
#46376=CARTESIAN_POINT('Ctrl Pts',(-0.124528470154946,0.0623295576548628,
-0.728906217715645));
#46377=CARTESIAN_POINT('Ctrl Pts',(-0.119824863719519,-0.0709529116469537,
-0.720958926407693));
#46378=CARTESIAN_POINT('Ctrl Pts',(-0.00521968128764912,-0.139158429726111,
-0.713011635099741));
#46379=CARTESIAN_POINT('Ctrl Pts',(0.114172914890457,-0.0797299137212506,
-0.705064343791791));
#46380=CARTESIAN_POINT('Ctrl Pts',(0.128847818153508,0.0528256887665676,
-0.697117052483838));
#46381=CARTESIAN_POINT('Ctrl Pts',(0.0253454263276182,0.136930358214871,
-0.689169761175887));
#46382=CARTESIAN_POINT('Ctrl Pts',(-0.101403412114119,0.0954445475037516,
-0.681222469867934));
#46383=CARTESIAN_POINT('Ctrl Pts',(-0.135146554936249,-0.0335815771732833,
-0.673275178559984));
#46384=CARTESIAN_POINT('Ctrl Pts',(-0.0449352953335994,-0.131807180646063,
-0.665327887252032));
#46385=CARTESIAN_POINT('Ctrl Pts',(0.086489946256864,-0.109141205935553,
-0.657380595944081));
#46386=CARTESIAN_POINT('Ctrl Pts',(0.138587900451223,0.0136274533609135,
-0.649433304636128));
#46387=CARTESIAN_POINT('Ctrl Pts',(0.0635751014943803,0.123897215895116,
-0.641486013328178));
#46388=CARTESIAN_POINT('Ctrl Pts',(-0.0697478313652302,0.120530301818377,
-0.633538722020224));
#46389=CARTESIAN_POINT('Ctrl Pts',(-0.139099094644512,0.00661479445324233,
-0.625591430712274));
#46390=CARTESIAN_POINT('Ctrl Pts',(-0.0808707450907354,-0.113367703624317,
-0.617644139404322));
#46391=CARTESIAN_POINT('Ctrl Pts',(0.0515310444452701,-0.129371036538173,
-0.609696848096371));
#46392=CARTESIAN_POINT('Ctrl Pts',(0.136669329383979,-0.0267171862724199,
-0.601749556788419));
#46393=CARTESIAN_POINT('Ctrl Pts',(0.0964565459097508,0.100441268349926,
-0.593802265480467));
#46394=CARTESIAN_POINT('Ctrl Pts',(-0.0322247413590565,0.135476491248201,
-0.585854974172516));
#46395=CARTESIAN_POINT('Ctrl Pts',(-0.131349976974611,0.0462546990623779,
-0.577907682864563));
#46396=CARTESIAN_POINT('Ctrl Pts',(-0.110002974788192,-0.0853912125123539,
-0.569960391556613));
#46397=CARTESIAN_POINT('Ctrl Pts',(0.0122371135094518,-0.13871757887715,
-0.562013100248661));
#46398=CARTESIAN_POINT('Ctrl Pts',(0.123253503998567,-0.0648142529746122,
-0.554065808940709));
#46399=CARTESIAN_POINT('Ctrl Pts',(0.121223620817521,0.0685357380676061,
-0.546118517632758));
#46400=CARTESIAN_POINT('Ctrl Pts',(0.00800924251344417,0.139025773405302,
-0.538171226324806));
#46401=CARTESIAN_POINT('Ctrl Pts',(-0.112551093444511,0.0820034450558435,
-0.530223935016855));
#46402=CARTESIAN_POINT('Ctrl Pts',(-0.129881246903541,-0.0502312187724236,
-0.522276643708902));
#46403=CARTESIAN_POINT('Ctrl Pts',(-0.0280862598533812,-0.136394558703894,
-0.514329352400952));
#46404=CARTESIAN_POINT('Ctrl Pts',(0.0994690254013135,-0.0974588457878242,
-0.506382061092999));
#46405=CARTESIAN_POINT('Ctrl Pts',(0.135792805648636,0.0308646654064759,
-0.498434769785048));
#46406=CARTESIAN_POINT('Ctrl Pts',(0.0475694519664141,0.130879566305045,
-0.490487478477097));
#46407=CARTESIAN_POINT('Ctrl Pts',(-0.0842838928387955,0.110853683044453,
-0.482540187169144));
#46408=CARTESIAN_POINT('Ctrl Pts',(-0.138833309506175,-0.0108455432387773,
-0.474592895861194));
#46409=CARTESIAN_POINT('Ctrl Pts',(-0.0660468875011581,-0.122597399189343,
-0.466645604553241));
#46410=CARTESIAN_POINT('Ctrl Pts',(0.0673167536278285,-0.121904751005003,
-0.45869831324529));
#46411=CARTESIAN_POINT('Ctrl Pts',(0.138938473380797,-0.00940288525907187,
-0.450751021937338));
#46412=CARTESIAN_POINT('Ctrl Pts',(0.0831278997256812,0.111723166459686,
-0.442803730629387));
#46413=CARTESIAN_POINT('Ctrl Pts',(-0.0489263424431069,0.1303783979489,
-0.434856439321435));
#46414=CARTESIAN_POINT('Ctrl Pts',(-0.136106073802305,0.0294525094126708,
-0.426909148013483));
#46415=CARTESIAN_POINT('Ctrl Pts',(-0.0984513463585633,-0.0984867810255157,
-0.418961856705532));
#46416=CARTESIAN_POINT('Ctrl Pts',(0.0295014860686701,-0.136095466332724,
-0.41101456539758));
#46417=CARTESIAN_POINT('Ctrl Pts',(0.130395995936294,-0.0488794218497269,
-0.403067274089629));
#46418=CARTESIAN_POINT('Ctrl Pts',(0.111693245167184,0.083168098575145,
-0.395119982781677));
#46419=CARTESIAN_POINT('Ctrl Pts',(-0.00945288246871811,0.138935080701795,
-0.387172691473725));
#46420=CARTESIAN_POINT('Ctrl Pts',(-0.121928967437574,0.0672728811348881,
-0.379225400165774));
#46421=CARTESIAN_POINT('Ctrl Pts',(-0.122573623894439,-0.0660910006125364,
-0.371278108857823));
#46422=CARTESIAN_POINT('Ctrl Pts',(-0.0107955825619163,-0.138837203348852,
-0.363330817549871));
#46423=CARTESIAN_POINT('Ctrl Pts',(0.11088400591638,-0.0842439960384028,
-0.35538352624192));
#46424=CARTESIAN_POINT('Ctrl Pts',(0.130862439686628,0.0476165466602282,
-0.347436234933967));
#46425=CARTESIAN_POINT('Ctrl Pts',(0.0308157975764226,0.135803903685831,
-0.339488943626016));
#46426=CARTESIAN_POINT('Ctrl Pts',(-0.0974946339853923,0.099433947827876,
-0.331541652318064));
#46427=CARTESIAN_POINT('Ctrl Pts',(-0.136384442868491,-0.0281353404108124,
-0.323594361010113));
#46428=CARTESIAN_POINT('Ctrl Pts',(-0.0501844769972613,-0.129899314490461,
-0.315647069702161));
#46429=CARTESIAN_POINT('Ctrl Pts',(0.0820439419124697,-0.112521576739974,
-0.30769977839421));
#46430=CARTESIAN_POINT('Ctrl Pts',(0.139022882231082,0.00805927122877484,
-0.299752487086258));
#46431=CARTESIAN_POINT('Ctrl Pts',(0.0684921106044416,0.12124827595279,
-0.291805195778306));
#46432=CARTESIAN_POINT('Ctrl Pts',(-0.0648586022690144,0.123230172231987,
-0.283857904470355));
#46433=CARTESIAN_POINT('Ctrl Pts',(-0.138721973491842,0.0121871943886424,
-0.275910613162403));
#46434=CARTESIAN_POINT('Ctrl Pts',(-0.0853516217728486,-0.110033696190289,
-0.267963321854451));
#46435=CARTESIAN_POINT('Ctrl Pts',(0.0463019631218519,-0.131333323447874,
-0.2600160305465));
#46436=CARTESIAN_POINT('Ctrl Pts',(0.135488078736147,-0.0321759872672793,
-0.252068739238548));
#46437=CARTESIAN_POINT('Ctrl Pts',(0.100406551398842,0.0964926840371405,
-0.244121447930597));
#46438=CARTESIAN_POINT('Ctrl Pts',(-0.0267663657998475,0.136659706204361,
-0.236174156622645));
#46439=CARTESIAN_POINT('Ctrl Pts',(-0.129389571901277,0.051484486179617,
-0.228226865314693));
#46440=CARTESIAN_POINT('Ctrl Pts',(-0.113338594488273,-0.080911535866496,
-0.220279574006742));
#46441=CARTESIAN_POINT('Ctrl Pts',(0.00666484966802229,-0.139096705296418,
-0.21233228269879));
#46442=CARTESIAN_POINT('Ctrl Pts',(0.12055539313165,-0.0697044532603406,
-0.204384991390839));
#46443=CARTESIAN_POINT('Ctrl Pts',(0.123874330089505,0.0636196824021741,
-0.196437700082887));
#46444=CARTESIAN_POINT('Ctrl Pts',(0.0135775806509123,0.138592795605587,
-0.188490408774936));
#46445=CARTESIAN_POINT('Ctrl Pts',(-0.109172322466555,0.0864506651613264,
-0.180543117466983));
#46446=CARTESIAN_POINT('Ctrl Pts',(-0.131791002478216,-0.0449827232515467,
-0.172595826159032));
#46447=CARTESIAN_POINT('Ctrl Pts',(-0.0335329405968919,-0.135158632142634,
-0.16464853485108));
#46448=CARTESIAN_POINT('Ctrl Pts',(0.0954810297919763,-0.101369056556591,
-0.156701243543129));
#46449=CARTESIAN_POINT('Ctrl Pts',(0.136921232711689,0.0253946947183125,
-0.148753952235177));
#46450=CARTESIAN_POINT('Ctrl Pts',(0.0527793109988149,0.128866829226554,
-0.140806660927226));
#46451=CARTESIAN_POINT('Ctrl Pts',(-0.0797709797129985,0.114144197653596,
-0.132859369619274));
#46452=CARTESIAN_POINT('Ctrl Pts',(-0.139156570159351,-0.00526972267221474,
-0.124912078311322));
#46453=CARTESIAN_POINT('Ctrl Pts',(-0.0709097346571945,-0.11985045568327,
-0.116964787003371));
#46454=CARTESIAN_POINT('Ctrl Pts',(0.0623742658464559,-0.124505905450053,
-0.109017495695419));
#46455=CARTESIAN_POINT('Ctrl Pts',(0.138449871985116,-0.0149668430727117,
-0.101070204387468));
#46456=CARTESIAN_POINT('Ctrl Pts',(0.0875406563815945,0.108300429783857,
-0.093122913079516));
#46457=CARTESIAN_POINT('Ctrl Pts',(-0.0436582776930319,0.132234560631268,
-0.0851756217715646));
#46458=CARTESIAN_POINT('Ctrl Pts',(-0.134816891517839,0.0348881726866265,
-0.0772283304636131));
#46459=CARTESIAN_POINT('Ctrl Pts',(-0.102318909486457,-0.0944629077688085,
-0.0692810391556614));
#46460=CARTESIAN_POINT('Ctrl Pts',(0.0240158013170603,-0.137163045762996,
-0.0613337478477098));
#46461=CARTESIAN_POINT('Ctrl Pts',(0.128339992499329,-0.0540801177957914,
-0.0533864565397582));
#46462=CARTESIAN_POINT('Ctrl Pts',(0.114921489370477,0.0786438502502632,
-0.0454391652318065));
#46463=CARTESIAN_POINT('Ctrl Pts',(-0.0038420162804081,0.139161560048721,
-0.0374918739238548));
#46464=CARTESIAN_POINT('Ctrl Pts',(-0.119195118024918,0.0721869595400255,
-0.0295445826159032));
#46465=CARTESIAN_POINT('Ctrl Pts',(-0.125001006615905,-0.0612850510018785,
-0.0215972913079518));
#46466=CARTESIAN_POINT('Ctrl Pts',(-0.0527668217477812,-0.112355607212729,
-0.0162990971026507));
#46467=CARTESIAN_POINT('Ctrl Pts',(-0.0138313775859597,-0.116960008631475,
-0.0136500000000002));
#46468=CARTESIAN_POINT('Ctrl Pts',(0.112054873528411,-0.0604069144927277,
-2.94864852262806));
#46469=CARTESIAN_POINT('Ctrl Pts',(0.132164055066097,-0.0231043670461693,
-2.94599942552541));
#46470=CARTESIAN_POINT('Ctrl Pts',(0.131850069163285,0.0725142137010918,
-2.94070123132011));
#46471=CARTESIAN_POINT('Ctrl Pts',(0.0101729848055668,0.150275971928739,
-2.93275394001216));
#46472=CARTESIAN_POINT('Ctrl Pts',(-0.120717947947423,0.0898301286852705,
-2.92480664870421));
#46473=CARTESIAN_POINT('Ctrl Pts',(-0.14094563806992,-0.0528164143684709,
-2.91685935739625));
#46474=CARTESIAN_POINT('Ctrl Pts',(-0.0318703010347745,-0.147119726764245,
-2.90891206608831));
#46475=CARTESIAN_POINT('Ctrl Pts',(0.106420360777253,-0.106434877139951,
-2.90096477478035));
#46476=CARTESIAN_POINT('Ctrl Pts',(0.147112089588147,0.0318429936417547,
-2.8930174834724));
#46477=CARTESIAN_POINT('Ctrl Pts',(0.0528704694334625,0.140929411341517,
-2.88507019216445));
#46478=CARTESIAN_POINT('Ctrl Pts',(-0.0898608711538647,0.120749856183999,
-2.8771229008565));
#46479=CARTESIAN_POINT('Ctrl Pts',(-0.150174366082989,-0.0101756491885928,
-2.86917560954855));
#46480=CARTESIAN_POINT('Ctrl Pts',(-0.0727495403866633,-0.131770316393393,
-2.8612283182406));
#46481=CARTESIAN_POINT('Ctrl Pts',(0.0713997434663159,-0.13250610228209,
-2.85328102693264));
#46482=CARTESIAN_POINT('Ctrl Pts',(0.150062424656416,-0.0117098566624688,
-2.8453337356247));
#46483=CARTESIAN_POINT('Ctrl Pts',(0.0910899976674201,0.119826804007082,
-2.83738644431673));
#46484=CARTESIAN_POINT('Ctrl Pts',(-0.0514287663295641,0.141459946095722,
-2.82943915300879));
#46485=CARTESIAN_POINT('Ctrl Pts',(-0.146777859433181,0.0333482235155928,
-2.82149186170084));
#46486=CARTESIAN_POINT('Ctrl Pts',(-0.107504477722029,-0.105350037017472,
-2.81354457039289));
#46487=CARTESIAN_POINT('Ctrl Pts',(0.0303703987486264,-0.147422792658834,
-2.80559727908493));
#46488=CARTESIAN_POINT('Ctrl Pts',(0.140390002687352,-0.0542815764800469,
-2.79764998777698));
#46489=CARTESIAN_POINT('Ctrl Pts',(0.121645990226168,0.0886458978282491,
-2.78970269646903));
#46490=CARTESIAN_POINT('Ctrl Pts',(-0.00866990722862085,0.150268674662333,
-2.78175540516108));
#46491=CARTESIAN_POINT('Ctrl Pts',(-0.131033895767171,0.0740672684712725,
-2.77380811385313));
#46492=CARTESIAN_POINT('Ctrl Pts',(-0.133215551178006,-0.0700675314913027,
-2.76586082254518));
#46493=CARTESIAN_POINT('Ctrl Pts',(-0.0132138921336998,-0.149937437181362,
-2.75791353123723));
#46494=CARTESIAN_POINT('Ctrl Pts',(0.118907351570326,-0.0922869643505502,
-2.74996623992927));
#46495=CARTESIAN_POINT('Ctrl Pts',(0.141968547680105,0.0500077344628434,
-2.74201894862132));
#46496=CARTESIAN_POINT('Ctrl Pts',(0.0348183114963835,0.146436085776981,
-2.73407165731337));
#46497=CARTESIAN_POINT('Ctrl Pts',(-0.104266760159845,0.108555445573249,
-2.72612436600542));
#46498=CARTESIAN_POINT('Ctrl Pts',(-0.147719916113032,-0.0288906285783304,
-2.71817707469747));
#46499=CARTESIAN_POINT('Ctrl Pts',(-0.0556865704959391,-0.139838649529325,
-2.71022978338951));
#46500=CARTESIAN_POINT('Ctrl Pts',(0.0874216661710837,-0.122528748954342,
-2.70228249208156));
#46501=CARTESIAN_POINT('Ctrl Pts',(0.150348055846523,0.00716269078799115,
-2.69433520077361));
#46502=CARTESIAN_POINT('Ctrl Pts',(0.0753774534239399,0.130284617478266,
-2.68638790946566));
#46503=CARTESIAN_POINT('Ctrl Pts',(-0.0687282238801868,0.133911438191447,
-2.67844061815771));
#46504=CARTESIAN_POINT('Ctrl Pts',(-0.149797400366207,0.0147166871172186,
-2.67049332684976));
#46505=CARTESIAN_POINT('Ctrl Pts',(-0.0934746377389571,-0.117975989657863,
-2.6625460355418));
#46506=CARTESIAN_POINT('Ctrl Pts',(0.0485816670290888,-0.142462850121947,
-2.65459874423386));
#46507=CARTESIAN_POINT('Ctrl Pts',(0.146079592131197,-0.0362849114504862,
-2.6466514529259));
#46508=CARTESIAN_POINT('Ctrl Pts',(0.109595496325569,0.103173006262973,
-2.63870416161795));
#46509=CARTESIAN_POINT('Ctrl Pts',(-0.0274079524291007,0.148002183023876,
-2.63075687031));
#46510=CARTESIAN_POINT('Ctrl Pts',(-0.139273236421531,0.0570859672148926,
-2.62280957900205));
#46511=CARTESIAN_POINT('Ctrl Pts',(-0.12339918734299,-0.0861886454196691,
-2.61486228769409));
#46512=CARTESIAN_POINT('Ctrl Pts',(0.00565475399413943,-0.15041231928753,
-2.60691499638615));
#46513=CARTESIAN_POINT('Ctrl Pts',(0.129522239394354,-0.076680059588263,
-2.59896770507819));
#46514=CARTESIAN_POINT('Ctrl Pts',(0.134593860612755,0.0673820059180649,
-2.59102041377024));
#46515=CARTESIAN_POINT('Ctrl Pts',(0.0162180023880564,0.149642301621998,
-2.58307312246229));
#46516=CARTESIAN_POINT('Ctrl Pts',(-0.11703276548923,0.0946529124651258,
-2.57512583115434));
#46517=CARTESIAN_POINT('Ctrl Pts',(-0.142942828180357,-0.0471507148194896,
-2.56717853984639));
#46518=CARTESIAN_POINT('Ctrl Pts',(-0.0377478630269907,-0.145708410440453,
-2.55923124853843));
#46519=CARTESIAN_POINT('Ctrl Pts',(0.102068878512243,-0.110624527458611,
-2.55128395723048));
#46520=CARTESIAN_POINT('Ctrl Pts',(0.148269568587044,0.0259225204638712,
-2.54333666592253));
#46521=CARTESIAN_POINT('Ctrl Pts',(0.058479624045545,0.138693819644855,
-2.53538937461458));
#46522=CARTESIAN_POINT('Ctrl Pts',(-0.0849469585590607,0.124257218171634,
-2.52744208330663));
#46523=CARTESIAN_POINT('Ctrl Pts',(-0.1504614590469,-0.00414624862564929,
-2.51949479199867));
#46524=CARTESIAN_POINT('Ctrl Pts',(-0.0779749557139858,-0.128746838087737,
-2.51154750069073));
#46525=CARTESIAN_POINT('Ctrl Pts',(0.0660290128194679,-0.135262749869557,
-2.50360020938277));
#46526=CARTESIAN_POINT('Ctrl Pts',(0.149472156620126,-0.0177176869685779,
-2.49565291807483));
#46527=CARTESIAN_POINT('Ctrl Pts',(0.0958216700153998,0.116077773891679,
-2.48770562676686));
#46528=CARTESIAN_POINT('Ctrl Pts',(-0.0457150216924184,0.143408433600851,
-2.47975833545893));
#46529=CARTESIAN_POINT('Ctrl Pts',(-0.145322578037573,0.0392070191254258,
-2.47181104415096));
#46530=CARTESIAN_POINT('Ctrl Pts',(-0.111642435499295,-0.100954487923884,
-2.46386375284302));
#46531=CARTESIAN_POINT('Ctrl Pts',(0.0244344820369845,-0.148522045918349,
-2.45591646153506));
#46532=CARTESIAN_POINT('Ctrl Pts',(0.138100457460221,-0.0598674008577744,
-2.44796917022712));
#46533=CARTESIAN_POINT('Ctrl Pts',(0.125102755165994,0.0836967304383223,
-2.44002187891916));
#46534=CARTESIAN_POINT('Ctrl Pts',(-0.00263732635950105,0.150495470183861,
-2.43207458761121));
#46535=CARTESIAN_POINT('Ctrl Pts',(-0.127958491523826,0.0792620116016167,
-2.42412729630325));
#46536=CARTESIAN_POINT('Ctrl Pts',(-0.135918038706145,-0.0646693806253223,
-2.41618000499531));
#46537=CARTESIAN_POINT('Ctrl Pts',(-0.0192155900683274,-0.149286982468378,
-2.40823271368735));
#46538=CARTESIAN_POINT('Ctrl Pts',(0.115111110887891,-0.0969807928733496,
-2.4002854223794));
#46539=CARTESIAN_POINT('Ctrl Pts',(0.143859619567644,0.0442747320041667,
-2.39233813107145));
#46540=CARTESIAN_POINT('Ctrl Pts',(0.0406622330303461,0.144922133717295,
-2.3843908397635));
#46541=CARTESIAN_POINT('Ctrl Pts',(-0.0998299465478195,0.112649118098844,
-2.37644354845555));
#46542=CARTESIAN_POINT('Ctrl Pts',(-0.148759589631659,-0.0229439867679609,
-2.3684962571476));
#46543=CARTESIAN_POINT('Ctrl Pts',(-0.0612491581131811,-0.137493209529105,
-2.36054896583964));
#46544=CARTESIAN_POINT('Ctrl Pts',(0.0824380867655902,-0.125935713308882,
-2.35260167453169));
#46545=CARTESIAN_POINT('Ctrl Pts',(0.150514349278652,0.0011281389150487,
-2.34465438322374));
#46546=CARTESIAN_POINT('Ctrl Pts',(0.0805410978400582,0.127157278969417,
-2.33670709191579));
#46547=CARTESIAN_POINT('Ctrl Pts',(-0.063303246044138,0.136559661234433,
-2.32875980060784));
#46548=CARTESIAN_POINT('Ctrl Pts',(-0.149086797785675,0.020711561075909,
-2.32081250929989));
#46549=CARTESIAN_POINT('Ctrl Pts',(-0.0981301644913087,-0.11413287367405,
-2.31286521799193));
#46550=CARTESIAN_POINT('Ctrl Pts',(0.0428299905732093,-0.144296340714818,
-2.30491792668398));
#46551=CARTESIAN_POINT('Ctrl Pts',(0.144507117743561,-0.0421133584226735,
-2.29697063537603));
#46552=CARTESIAN_POINT('Ctrl Pts',(0.113644474037177,0.0986953674546136,
-2.28902334406808));
#46553=CARTESIAN_POINT('Ctrl Pts',(-0.0214511845233532,0.148982175842391,
-2.28107605276013));
#46554=CARTESIAN_POINT('Ctrl Pts',(-0.136872136909167,0.0626247568786199,
-2.27312876145218));
#46555=CARTESIAN_POINT('Ctrl Pts',(-0.126756008847893,-0.0811711540951639,
-2.26518147014422));
#46556=CARTESIAN_POINT('Ctrl Pts',(-0.000381161961692621,-0.150518094433018,
-2.25723417883628));
#46557=CARTESIAN_POINT('Ctrl Pts',(0.126343280984955,-0.081812085819546,
-2.24928688752832));
#46558=CARTESIAN_POINT('Ctrl Pts',(0.13718755294046,0.0619307464382313,
-2.24133959622038));
#46559=CARTESIAN_POINT('Ctrl Pts',(0.0222054495741949,0.148871622700217,
-2.23339230491242));
#46560=CARTESIAN_POINT('Ctrl Pts',(-0.113143160610104,0.0992696693020791,
-2.22544501360447));
#46561=CARTESIAN_POINT('Ctrl Pts',(-0.144718553130867,-0.0413809426656339,
-2.21749772229651));
#46562=CARTESIAN_POINT('Ctrl Pts',(-0.0435602493944256,-0.144077571845459,
-2.20955043098857));
#46563=CARTESIAN_POINT('Ctrl Pts',(0.0975508647241037,-0.114628403233089,
-2.20160313968061));
#46564=CARTESIAN_POINT('Ctrl Pts',(0.14918978216991,0.0199562254016758,
-2.19365584837266));
#46565=CARTESIAN_POINT('Ctrl Pts',(0.0639940588401701,0.136237302048113,
-2.18570855706471));
#46566=CARTESIAN_POINT('Ctrl Pts',(-0.0798960598147894,0.127563559303821,
-2.17776126575676));
#46567=CARTESIAN_POINT('Ctrl Pts',(-0.150506705270388,0.00189042451330132,
-2.1698139744488));
#46568=CARTESIAN_POINT('Ctrl Pts',(-0.0830748477445828,-0.125516579416435,
-2.16186668314085));
#46569=CARTESIAN_POINT('Ctrl Pts',(0.0605520198099057,-0.13780165069087,
-2.1539193918329));
#46570=CARTESIAN_POINT('Ctrl Pts',(0.148641478847462,-0.0236971053554501,
-2.14597210052495));
#46571=CARTESIAN_POINT('Ctrl Pts',(0.100399192730552,0.112142071209878,
-2.138024809217));
#46572=CARTESIAN_POINT('Ctrl Pts',(-0.0399277339805376,0.14512621436311,
-2.13007751790905));
#46573=CARTESIAN_POINT('Ctrl Pts',(-0.143633539213038,0.0450027604633815,
-2.1221302266011));
#46574=CARTESIAN_POINT('Ctrl Pts',(-0.115600806754312,-0.0963965534339281,
-2.11418293529314));
#46575=CARTESIAN_POINT('Ctrl Pts',(0.0184592597183131,-0.149382387739786,
-2.1062356439852));
#46576=CARTESIAN_POINT('Ctrl Pts',(0.13558876877742,-0.0653569263170418,
-2.09828835267724));
#46577=CARTESIAN_POINT('Ctrl Pts',(0.128358283478957,0.0786129321328472,
-2.09034106136929));
#46578=CARTESIAN_POINT('Ctrl Pts',(0.00339949698620866,0.150480182935922,
-2.08239377006134));
#46579=CARTESIAN_POINT('Ctrl Pts',(-0.124677257387179,0.0843292566467827,
-2.07444647875338));
#46580=CARTESIAN_POINT('Ctrl Pts',(-0.138401892739269,-0.0591672047875833,
-2.06649918744544));
#46581=CARTESIAN_POINT('Ctrl Pts',(-0.0251863784364351,-0.148396389367951,
-2.05855189613748));
#46582=CARTESIAN_POINT('Ctrl Pts',(0.111129706131067,-0.101518621205228,
-2.05060460482953));
#46583=CARTESIAN_POINT('Ctrl Pts',(0.145519283421962,0.038470510635376,
-2.04265731352158));
#46584=CARTESIAN_POINT('Ctrl Pts',(0.0464407465877105,0.143175064492962,
-2.03471002221363));
#46585=CARTESIAN_POINT('Ctrl Pts',(-0.0952325496479617,0.116561586827464,
-2.02676273090568));
#46586=CARTESIAN_POINT('Ctrl Pts',(-0.149559973185881,-0.0169604379904061,
-2.01881543959772));
#46587=CARTESIAN_POINT('Ctrl Pts',(-0.066713222275424,-0.134926602305912,
-2.01086814828978));
#46588=CARTESIAN_POINT('Ctrl Pts',(0.0773219000654605,-0.12914010146525,
-2.00292085698182));
#46589=CARTESIAN_POINT('Ctrl Pts',(0.150438530096393,-0.00490822764595809,
-1.99497356567387));
#46590=CARTESIAN_POINT('Ctrl Pts',(0.0855751863976413,0.12382539928947,
-1.98702627436592));
#46591=CARTESIAN_POINT('Ctrl Pts',(-0.0577764406118648,0.138988218732421,
-1.97907898305797));
#46592=CARTESIAN_POINT('Ctrl Pts',(-0.148136378904979,0.0266731190734859,
-1.97113169175001));
#46593=CARTESIAN_POINT('Ctrl Pts',(-0.102627842169638,-0.110106167165113,
-1.96318440044207));
#46594=CARTESIAN_POINT('Ctrl Pts',(0.0370094191512704,-0.145897720785054,
-1.95523710913411));
#46595=CARTESIAN_POINT('Ctrl Pts',(0.142702193784019,-0.0478740631805581,
-1.94728981782616));
#46596=CARTESIAN_POINT('Ctrl Pts',(0.11751064684788,0.094058970404638,-1.93934252651821));
#46597=CARTESIAN_POINT('Ctrl Pts',(-0.0154599109217152,0.149722520652307,
-1.93139523521026));
#46598=CARTESIAN_POINT('Ctrl Pts',(-0.134250869213207,0.0680628103422581,
-1.92344794390231));
#46599=CARTESIAN_POINT('Ctrl Pts',(-0.129908934652342,-0.0760230934235222,
-1.91550065259436));
#46600=CARTESIAN_POINT('Ctrl Pts',(-0.00641646479246623,-0.150381750939916,
-1.9075533612864));
#46601=CARTESIAN_POINT('Ctrl Pts',(0.122961090776067,-0.0868125117212231,
-1.89960606997845));
#46602=CARTESIAN_POINT('Ctrl Pts',(0.139560569716333,0.0563798671215204,
-1.8916587786705));
#46603=CARTESIAN_POINT('Ctrl Pts',(0.0281571777775729,0.147861473602118,
-1.88371148736255));
#46604=CARTESIAN_POINT('Ctrl Pts',(-0.109071557226972,0.103726744093659,
-1.8757641960546));
#46605=CARTESIAN_POINT('Ctrl Pts',(-0.146261488401206,-0.0355446064382738,
-1.86781690474665));
#46606=CARTESIAN_POINT('Ctrl Pts',(-0.0493025661245861,-0.142214974632486,
-1.85986961343869));
#46607=CARTESIAN_POINT('Ctrl Pts',(0.0928759337051868,-0.118447891389326,
-1.85192232213075));
#46608=CARTESIAN_POINT('Ctrl Pts',(0.149870013795216,0.0139578293874739,
-1.84397503082279));
#46609=CARTESIAN_POINT('Ctrl Pts',(0.0694055548189475,0.133561637443025,
-1.83602773951484));
#46610=CARTESIAN_POINT('Ctrl Pts',(-0.0747166427996508,0.130664705735471,
-1.82808044820689));
#46611=CARTESIAN_POINT('Ctrl Pts',(-0.150309851175531,0.00792405677526355,
-1.82013315689893));
#46612=CARTESIAN_POINT('Ctrl Pts',(-0.0880411082067443,-0.122084418751601,
-1.81218586559099));
#46613=CARTESIAN_POINT('Ctrl Pts',(0.0549776247394447,-0.140118888142166,
-1.80423857428303));
#46614=CARTESIAN_POINT('Ctrl Pts',(0.147571701100593,-0.0296384053293244,
-1.79629128297508));
#46615=CARTESIAN_POINT('Ctrl Pts',(0.104815216484724,0.108025980344769,
-1.78834399166713));
#46616=CARTESIAN_POINT('Ctrl Pts',(-0.0340762197806085,0.146610549694254,
-1.78039670035918));
#46617=CARTESIAN_POINT('Ctrl Pts',(-0.141713456027351,0.0507261117864536,
-1.77244940905122));
#46618=CARTESIAN_POINT('Ctrl Pts',(-0.119373226213588,-0.0916835585017708,
-1.76450211774327));
#46619=CARTESIAN_POINT('Ctrl Pts',(0.012454344419212,-0.150002437784443,
-1.75655482643532));
#46620=CARTESIAN_POINT('Ctrl Pts',(0.132858976296346,-0.0707413206950133,
-1.74860753512737));
#46621=CARTESIAN_POINT('Ctrl Pts',(0.131407338723251,0.073402679555044,
-1.74066024381942));
#46622=CARTESIAN_POINT('Ctrl Pts',(0.00943085200875732,0.150222838032626,
-1.73271295251147));
#46623=CARTESIAN_POINT('Ctrl Pts',(-0.121195471363827,0.0892608523210916,
-1.72476566120351));
#46624=CARTESIAN_POINT('Ctrl Pts',(-0.14066311787203,-0.0535698544585239,
-1.71681836989557));
#46625=CARTESIAN_POINT('Ctrl Pts',(-0.0311166527940441,-0.14726709053649,
-1.70887107858761));
#46626=CARTESIAN_POINT('Ctrl Pts',(0.106969541649328,-0.105893149898945,
-1.70092378727966));
#46627=CARTESIAN_POINT('Ctrl Pts',(0.146944869566731,0.0326044068218462,
-1.69297649597171));
#46628=CARTESIAN_POINT('Ctrl Pts',(0.0521445570312648,0.141197688395388,
-1.68502920466376));
#46629=CARTESIAN_POINT('Ctrl Pts',(-0.0904819646855179,0.120286558279953,
-1.67708191335581));
#46630=CARTESIAN_POINT('Ctrl Pts',(-0.150119779305,-0.0109496071895714,
-1.66913462204785));
#46631=CARTESIAN_POINT('Ctrl Pts',(-0.0720699736616587,-0.132142956424456,
-1.6611873307399));
#46632=CARTESIAN_POINT('Ctrl Pts',(0.0720813358062882,-0.132136758945303,
-1.65324003943195));
#46633=CARTESIAN_POINT('Ctrl Pts',(0.150120720260215,-0.0109366989874593,
-1.645292748124));
#46634=CARTESIAN_POINT('Ctrl Pts',(0.0904716214212405,0.120294337994768,
-1.63734545681605));
#46635=CARTESIAN_POINT('Ctrl Pts',(-0.0521566978274638,0.141193204184629,
-1.6293981655081));
#46636=CARTESIAN_POINT('Ctrl Pts',(-0.146947672537843,0.0325917715366741,
-1.62145087420015));
#46637=CARTESIAN_POINT('Ctrl Pts',(-0.106960435952101,-0.105902347363619,
-1.61350358289219));
#46638=CARTESIAN_POINT('Ctrl Pts',(0.031129315550067,-0.147264414403387,
-1.60555629158424));
#46639=CARTESIAN_POINT('Ctrl Pts',(0.140667723596079,-0.0535577592369685,
-1.59760900027629));
#46640=CARTESIAN_POINT('Ctrl Pts',(0.12118779575457,0.0892712730744692,
-1.58966170896834));
#46641=CARTESIAN_POINT('Ctrl Pts',(-0.0094437689971061,0.150222026558415,
-1.58171441766039));
#46642=CARTESIAN_POINT('Ctrl Pts',(-0.131413649821834,0.0733913801252743,
-1.57376712635244));
#46643=CARTESIAN_POINT('Ctrl Pts',(-0.132852893059766,-0.0707527444120611,
-1.56581983504448));
#46644=CARTESIAN_POINT('Ctrl Pts',(-0.0124414463012357,-0.150003508126047,
-1.55787254373653));
#46645=CARTESIAN_POINT('Ctrl Pts',(0.119381109251721,-0.0916732937665955,
-1.54992525242858));
#46646=CARTESIAN_POINT('Ctrl Pts',(0.141709093780764,0.0507382969365613,
-1.54197796112063));
#46647=CARTESIAN_POINT('Ctrl Pts',(0.0340636132367385,0.146613479221543,
-1.53403066981268));
#46648=CARTESIAN_POINT('Ctrl Pts',(-0.104824504792056,0.108016967330545,
-1.52608337850473));
#46649=CARTESIAN_POINT('Ctrl Pts',(-0.147569152074577,-0.0296510942829791,
-1.51813608719677));
#46650=CARTESIAN_POINT('Ctrl Pts',(-0.0549655763086878,-0.140123614916407,
-1.51018879588882));
#46651=CARTESIAN_POINT('Ctrl Pts',(0.0880516054014386,-0.122076848019669,
-1.50224150458087));
#46652=CARTESIAN_POINT('Ctrl Pts',(0.150309169263914,0.00793698125107607,
-1.49429421327292));
#46653=CARTESIAN_POINT('Ctrl Pts',(0.0747054072208741,0.130671129818913,
-1.48634692196497));
#46654=CARTESIAN_POINT('Ctrl Pts',(-0.0694170389597775,0.133555669060675,
-1.47839963065702));
#46655=CARTESIAN_POINT('Ctrl Pts',(-0.149871213415591,0.0139449426505173,
-1.47045233934906));
#46656=CARTESIAN_POINT('Ctrl Pts',(-0.0928657485312122,-0.118455876958156,
-1.46250504804111));
#46657=CARTESIAN_POINT('Ctrl Pts',(0.0493147944034109,-0.142210734788684,
-1.45455775673316));
#46658=CARTESIAN_POINT('Ctrl Pts',(0.14626454419011,-0.0355320299032718,
-1.44661046542521));
#46659=CARTESIAN_POINT('Ctrl Pts',(0.109062637801998,0.103736122309724,
-1.43866317411726));
#46660=CARTESIAN_POINT('Ctrl Pts',(-0.0281698916530059,0.147859051939493,
-1.43071588280931));
#46661=CARTESIAN_POINT('Ctrl Pts',(-0.139565417065501,0.0563678666930081,
-1.42276859150136));
#46662=CARTESIAN_POINT('Ctrl Pts',(-0.122953625682683,-0.0868230843017613,
-1.4148213001934));
#46663=CARTESIAN_POINT('Ctrl Pts',(0.00642939545620693,-0.150381198659458,
-1.40687400888545));
#46664=CARTESIAN_POINT('Ctrl Pts',(0.129915471074711,-0.0760119228254608,
-1.3989267175775));
#46665=CARTESIAN_POINT('Ctrl Pts',(0.1342450162852,0.0680743537521607,-1.39097942626955));
#46666=CARTESIAN_POINT('Ctrl Pts',(0.0154470368615123,0.149723849430834,
-1.38303213496159));
#46667=CARTESIAN_POINT('Ctrl Pts',(-0.117518734144473,0.0940488658159606,
-1.37508484365365));
#46668=CARTESIAN_POINT('Ctrl Pts',(-0.14269807676931,-0.0478863333585683,
-1.36713755234569));
#46669=CARTESIAN_POINT('Ctrl Pts',(-0.0369968738896843,-0.145900902528321,
-1.35919026103774));
#46670=CARTESIAN_POINT('Ctrl Pts',(0.102637309351477,-0.110097342226219,
-1.35124296972979));
#46671=CARTESIAN_POINT('Ctrl Pts',(0.148134084849236,0.0266858565923466,
-1.34329567842184));
#46672=CARTESIAN_POINT('Ctrl Pts',(0.0577644893922145,0.138993186169123,
-1.33534838711389));
#46673=CARTESIAN_POINT('Ctrl Pts',(-0.0855858333009689,0.123818040585234,
-1.32740109580594));
#46674=CARTESIAN_POINT('Ctrl Pts',(-0.150438107502626,-0.00492116319747254,
-1.31945380449798));
#46675=CARTESIAN_POINT('Ctrl Pts',(-0.0773107955712941,-0.129146749569324,
-1.31150651319003));
#46676=CARTESIAN_POINT('Ctrl Pts',(0.0667248237937332,-0.134920865420747,
-1.30355922188208));
#46677=CARTESIAN_POINT('Ctrl Pts',(0.149561430988952,-0.0169475779014209,
-1.29561193057413));
#46678=CARTESIAN_POINT('Ctrl Pts',(0.0952225266605833,0.116569775038653,
-1.28766463926618));
#46679=CARTESIAN_POINT('Ctrl Pts',(-0.0464530574311598,0.143171070721307,
-1.27971734795822));
#46680=CARTESIAN_POINT('Ctrl Pts',(-0.145522590799675,0.0384579979086082,
-1.27177005665028));
#46681=CARTESIAN_POINT('Ctrl Pts',(-0.111120976565583,-0.101528176400933,
-1.26382276534232));
#46682=CARTESIAN_POINT('Ctrl Pts',(0.0251991383179859,-0.148394223149754,
-1.25587547403437));
#46683=CARTESIAN_POINT('Ctrl Pts',(0.138406979764036,-0.0591553039784738,
-1.24792818272642));
#46684=CARTESIAN_POINT('Ctrl Pts',(0.124670005811998,0.0843399768023711,
-1.23998089141847));
#46685=CARTESIAN_POINT('Ctrl Pts',(-0.00341243612485143,0.150479890071337,
-1.23203360011052));
#46686=CARTESIAN_POINT('Ctrl Pts',(-0.12836504259628,0.0786018948591122,
-1.22408630880257));
#46687=CARTESIAN_POINT('Ctrl Pts',(-0.13558314851193,-0.0653685847772444,
-1.21613901749461));
#46688=CARTESIAN_POINT('Ctrl Pts',(-0.018446414893607,-0.149383974420822,
-1.20819172618666));
#46689=CARTESIAN_POINT('Ctrl Pts',(0.11560909505679,-0.096386613055642,
-1.20024443487871));
#46690=CARTESIAN_POINT('Ctrl Pts',(0.143629669086001,0.0450151107344386,
-1.19229714357076));
#46691=CARTESIAN_POINT('Ctrl Pts',(0.0399152550467209,0.145129647042715,
-1.18434985226281));
#46692=CARTESIAN_POINT('Ctrl Pts',(-0.100408834979363,0.112133437895548,
-1.17640256095486));
#46693=CARTESIAN_POINT('Ctrl Pts',(-0.14863944068462,-0.0237098863167076,
-1.1684552696469));
#46694=CARTESIAN_POINT('Ctrl Pts',(-0.0605401706079386,-0.137806856792214,
-1.16050797833895));
#46695=CARTESIAN_POINT('Ctrl Pts',(0.0830856400745417,-0.125509435699439,
-1.152560687031));
#46696=CARTESIAN_POINT('Ctrl Pts',(0.150506542164431,0.00190336593806516,
-1.14461339572305));
#46697=CARTESIAN_POINT('Ctrl Pts',(0.0798850908712658,0.127570428754776,
-1.1366661044151));
#46698=CARTESIAN_POINT('Ctrl Pts',(-0.064005773070029,0.136231798967407,
-1.12871881310715));
#46699=CARTESIAN_POINT('Ctrl Pts',(-0.149191497569375,0.0199433971327684,
-1.12077152179919));
#46700=CARTESIAN_POINT('Ctrl Pts',(-0.0975410079543931,-0.114636790793483,
-1.11282423049124));
#46701=CARTESIAN_POINT('Ctrl Pts',(0.0435726378512938,-0.144073825752174,
-1.10487693918329));
#46702=CARTESIAN_POINT('Ctrl Pts',(0.144722110767215,-0.0413684987795025,
-1.09692964787534));
#46703=CARTESIAN_POINT('Ctrl Pts',(0.113134624414992,0.099279397634488,
-1.08898235656739));
#46704=CARTESIAN_POINT('Ctrl Pts',(-0.0222182503300599,0.148869712797663,
-1.08103506525944));
#46705=CARTESIAN_POINT('Ctrl Pts',(-0.137192877594915,0.0619189500348204,
-1.07308777395148));
#46706=CARTESIAN_POINT('Ctrl Pts',(-0.126336245844431,-0.0818229492387265,
-1.06514048264353));
#46707=CARTESIAN_POINT('Ctrl Pts',(0.000394104371340178,-0.150518061102089,
-1.05719319133558));
#46708=CARTESIAN_POINT('Ctrl Pts',(0.12676298794177,-0.0811602545847577,
-1.04924590002763));
#46709=CARTESIAN_POINT('Ctrl Pts',(0.136866751566568,0.0626365257002925,
-1.04129860871968));
#46710=CARTESIAN_POINT('Ctrl Pts',(0.0214383741001049,0.1489840197878,-1.03335131741173));
#46711=CARTESIAN_POINT('Ctrl Pts',(-0.113652960012132,0.0986855952845626,
-1.02540402610377));
#46712=CARTESIAN_POINT('Ctrl Pts',(-0.144503496060692,-0.0421257838197151,
-1.01745673479582));
#46713=CARTESIAN_POINT('Ctrl Pts',(-0.0428175829859707,-0.144300022950198,
-1.00950944348787));
#46714=CARTESIAN_POINT('Ctrl Pts',(0.0981399779291522,-0.114124435456451,
-1.00156215217992));
#46715=CARTESIAN_POINT('Ctrl Pts',(0.149085016335446,0.0207243803392913,
-0.993614860871969));
#46716=CARTESIAN_POINT('Ctrl Pts',(0.06329150362539,0.136565103906617,-0.985667569564016));
#46717=CARTESIAN_POINT('Ctrl Pts',(-0.0805520312561653,0.127150353112736,
-0.977720278256066));
#46718=CARTESIAN_POINT('Ctrl Pts',(-0.150514445726104,0.00111519682184853,
-0.969772986948113));
#46719=CARTESIAN_POINT('Ctrl Pts',(-0.0824272577842244,-0.125942801343947,
-0.961825695640163));
#46720=CARTESIAN_POINT('Ctrl Pts',(0.0612609803433331,-0.1374879424661,
-0.953878404332209));
#46721=CARTESIAN_POINT('Ctrl Pts',(0.14876156193761,-0.0229311954784377,
-0.94593111302426));
#46722=CARTESIAN_POINT('Ctrl Pts',(0.0998202599599995,0.112657701635114,
-0.937983821716306));
#46723=CARTESIAN_POINT('Ctrl Pts',(-0.0406746941182161,0.144918636808996,
-0.930036530408357));
#46724=CARTESIAN_POINT('Ctrl Pts',(-0.143863426031812,0.044262361963377,
-0.922089239100402));
#46725=CARTESIAN_POINT('Ctrl Pts',(-0.115102771496254,-0.0969906904299014,
-0.914141947792454));
#46726=CARTESIAN_POINT('Ctrl Pts',(0.0192284265502686,-0.149285329649597,
-0.906194656484499));
#46727=CARTESIAN_POINT('Ctrl Pts',(0.135923598848805,-0.0646576933719181,
-0.89824736517655));
#46728=CARTESIAN_POINT('Ctrl Pts',(0.127951675647373,0.0792730139153126,
-0.890300073868596));
#46729=CARTESIAN_POINT('Ctrl Pts',(0.00262438588405391,0.150495696399996,
-0.882352782560647));
#46730=CARTESIAN_POINT('Ctrl Pts',(-0.12510995142956,0.0836859730748307,
-0.874405491252693));
#46731=CARTESIAN_POINT('Ctrl Pts',(-0.1380953092064,-0.0598792753077094,
-0.866458199944743));
#46732=CARTESIAN_POINT('Ctrl Pts',(-0.0244217111673174,-0.148524146386532,
-0.858510908636791));
#46733=CARTESIAN_POINT('Ctrl Pts',(0.111651115733821,-0.100944887892259,
-0.850563617328839));
#46734=CARTESIAN_POINT('Ctrl Pts',(0.145319206255449,0.0392195146511816,
-0.842616326020887));
#46735=CARTESIAN_POINT('Ctrl Pts',(0.0457026904418683,0.143412363911075,
-0.834669034712937));
#46736=CARTESIAN_POINT('Ctrl Pts',(-0.095831650695478,0.116069534164516,
-0.826721743404984));
#46737=CARTESIAN_POINT('Ctrl Pts',(-0.149470632598979,-0.0177305393783937,
-0.818774452097033));
#46738=CARTESIAN_POINT('Ctrl Pts',(-0.0660173819065402,-0.135268426923631,
-0.810827160789081));
#46739=CARTESIAN_POINT('Ctrl Pts',(0.0779860258190115,-0.128740132876833,
-0.802879869481131));
#46740=CARTESIAN_POINT('Ctrl Pts',(0.150461815008973,-0.00413331106909414,
-0.794932578173178));
#46741=CARTESIAN_POINT('Ctrl Pts',(0.0849362738950762,0.124264521940127,
-0.786985286865226));
#46742=CARTESIAN_POINT('Ctrl Pts',(-0.0584915495213012,0.138688790717869,
-0.779037995557275));
#46743=CARTESIAN_POINT('Ctrl Pts',(-0.148271797006258,0.0259097712981566,
-0.771090704249323));
#46744=CARTESIAN_POINT('Ctrl Pts',(-0.102059366002084,-0.110633303518608,
-0.763143412941372));
#46745=CARTESIAN_POINT('Ctrl Pts',(0.0377603917342272,-0.145705164123532,
-0.75519612163342));
#46746=CARTESIAN_POINT('Ctrl Pts',(0.14294688194145,-0.0471384235990644,
-0.747248830325468));
#46747=CARTESIAN_POINT('Ctrl Pts',(0.11702462625503,0.0946629752651919,
-0.739301539017517));
#46748=CARTESIAN_POINT('Ctrl Pts',(-0.0162308694334636,0.149640906551725,
-0.731354247709565));
#46749=CARTESIAN_POINT('Ctrl Pts',(-0.134599654007431,0.0673704325150745,
-0.723406956401614));
#46750=CARTESIAN_POINT('Ctrl Pts',(-0.129515645523193,-0.0766911963715416,
-0.715459665093661));
#46751=CARTESIAN_POINT('Ctrl Pts',(-0.00564182065732522,-0.150412804959745,
-0.707512373785711));
#46752=CARTESIAN_POINT('Ctrl Pts',(0.123406597882029,-0.0861780345295194,
-0.699565082477759));
#46753=CARTESIAN_POINT('Ctrl Pts',(0.139268327327031,0.0570979425173868,
-0.691617791169807));
#46754=CARTESIAN_POINT('Ctrl Pts',(0.0273952262492426,0.148004539170056,
-0.683670499861856));
#46755=CARTESIAN_POINT('Ctrl Pts',(-0.10960436732862,0.10316358223075,-0.675723208553903));
#46756=CARTESIAN_POINT('Ctrl Pts',(-0.146076471605894,-0.0362974720794752,
-0.667775917245953));
#46757=CARTESIAN_POINT('Ctrl Pts',(-0.0485694170746423,-0.142467026926293,
-0.659828625938001));
#46758=CARTESIAN_POINT('Ctrl Pts',(0.0934847816472068,-0.117967951735047,
-0.651881334630049));
#46759=CARTESIAN_POINT('Ctrl Pts',(0.149796134387099,0.0147295675045261,
-0.643934043322098));
#46760=CARTESIAN_POINT('Ctrl Pts',(0.0687167091507831,0.133917347344078,
-0.635986752014146));
#46761=CARTESIAN_POINT('Ctrl Pts',(-0.0753886557656117,0.130278135610093,
-0.628039460706194));
#46762=CARTESIAN_POINT('Ctrl Pts',(-0.150348671180187,0.00714976297088918,
-0.620092169398244));
#46763=CARTESIAN_POINT('Ctrl Pts',(-0.0874111301214144,-0.122536265517948,
-0.61214487809029));
#46764=CARTESIAN_POINT('Ctrl Pts',(0.0556985944205823,-0.139833860762547,
-0.60419758678234));
#46765=CARTESIAN_POINT('Ctrl Pts',(0.147722399750208,-0.0288779266608177,
-0.596250295474387));
#46766=CARTESIAN_POINT('Ctrl Pts',(0.104257425551351,0.108564410621494,
-0.588303004166437));
#46767=CARTESIAN_POINT('Ctrl Pts',(-0.0348309027808034,0.146433091368251,
-0.580355712858484));
#46768=CARTESIAN_POINT('Ctrl Pts',(-0.141972847114145,0.0499955269848398,
-0.572408421550534));
#46769=CARTESIAN_POINT('Ctrl Pts',(-0.118899415754923,-0.0922971883067176,
-0.564461130242581));
#46770=CARTESIAN_POINT('Ctrl Pts',(0.0132267845447208,-0.149936300497229,
-0.55651383893463));
#46771=CARTESIAN_POINT('Ctrl Pts',(0.133221575538256,-0.0700560764480323,
-0.548566547626678));
#46772=CARTESIAN_POINT('Ctrl Pts',(0.131027526470557,0.0740785349692836,
-0.540619256318727));
#46773=CARTESIAN_POINT('Ctrl Pts',(0.00865698638896329,0.150269420118829,
-0.532671965010775));
#46774=CARTESIAN_POINT('Ctrl Pts',(-0.121653612358199,0.0886354366852716,
-0.524724673702824));
#46775=CARTESIAN_POINT('Ctrl Pts',(-0.140385334161072,-0.0542936459327594,
-0.516777382394872));
#46776=CARTESIAN_POINT('Ctrl Pts',(-0.0303577234500885,-0.147425407115313,
-0.50883009108692));
#46777=CARTESIAN_POINT('Ctrl Pts',(0.107513537962964,-0.105340785979954,
-0.500882799778969));
#46778=CARTESIAN_POINT('Ctrl Pts',(0.146774987553141,0.0333608312990502,
-0.492935508471017));
#46779=CARTESIAN_POINT('Ctrl Pts',(0.0514166099369417,0.141464392193867,
-0.484988217163065));
#46780=CARTESIAN_POINT('Ctrl Pts',(-0.091100314654041,0.119818924657679,
-0.477040925855113));
#46781=CARTESIAN_POINT('Ctrl Pts',(-0.150061390788673,-0.0117226716561039,
-0.469093634547163));
#46782=CARTESIAN_POINT('Ctrl Pts',(-0.0713883997359057,-0.132512408548537,
-0.46114634323921));
#46783=CARTESIAN_POINT('Ctrl Pts',(0.0727609657127887,-0.131763742754713,
-0.45319905193126));
#46784=CARTESIAN_POINT('Ctrl Pts',(0.15017505974422,-0.0101633393630106,
-0.445251760623307));
#46785=CARTESIAN_POINT('Ctrl Pts',(0.0898508311193224,0.120758727151932,
-0.437304469315356));
#46786=CARTESIAN_POINT('Ctrl Pts',(-0.0528832383189022,0.140922692072975,
-0.429357178007404));
#46787=CARTESIAN_POINT('Ctrl Pts',(-0.147113591127436,0.0318344678262087,
-0.421409886699453));
#46788=CARTESIAN_POINT('Ctrl Pts',(-0.106413554586663,-0.106451855016336,
-0.413462595391501));
#46789=CARTESIAN_POINT('Ctrl Pts',(0.0318874054471912,-0.147102125783533,
-0.405515304083549));
#46790=CARTESIAN_POINT('Ctrl Pts',(0.140941713289669,-0.0528325230436766,
-0.397568012775598));
#46791=CARTESIAN_POINT('Ctrl Pts',(0.120726385988382,0.0898942810326212,
-0.389620721467646));
#46792=CARTESIAN_POINT('Ctrl Pts',(-0.0102173800744564,0.150171392683833,
-0.381673430159694));
#46793=CARTESIAN_POINT('Ctrl Pts',(-0.131789917680354,0.0727135450517523,
-0.373726138851743));
#46794=CARTESIAN_POINT('Ctrl Pts',(-0.132486710437372,-0.0714360804752875,
-0.365778847543792));
#46795=CARTESIAN_POINT('Ctrl Pts',(-0.0116686704320159,-0.150065599544122,
-0.35783155623584));
#46796=CARTESIAN_POINT('Ctrl Pts',(0.119851699878208,-0.0910571912178954,
-0.349884264927888));
#46797=CARTESIAN_POINT('Ctrl Pts',(0.141445880467903,0.0514675133928953,
-0.341936973619936));
#46798=CARTESIAN_POINT('Ctrl Pts',(0.0333080113052628,0.146786983139092,
-0.333989682311985));
#46799=CARTESIAN_POINT('Ctrl Pts',(-0.105379468531873,0.107475623506582,
-0.326042391004033));
#46800=CARTESIAN_POINT('Ctrl Pts',(-0.14741447316628,-0.0304107733754844,
-0.318095099696082));
#46801=CARTESIAN_POINT('Ctrl Pts',(-0.0542431239375945,-0.140404862955942,
-0.31014780838813));
#46802=CARTESIAN_POINT('Ctrl Pts',(0.088679208706928,-0.121621708503485,
-0.302200517080178));
#46803=CARTESIAN_POINT('Ctrl Pts',(0.150266295122196,0.00871106115410149,
-0.294253225772228));
#46804=CARTESIAN_POINT('Ctrl Pts',(0.0740313791546959,0.131054175578779,
-0.286305934464275));
#46805=CARTESIAN_POINT('Ctrl Pts',(-0.0701040124716336,0.133196356825569,
-0.278358643156324));
#46806=CARTESIAN_POINT('Ctrl Pts',(-0.149941050524403,0.0131728282375115,
-0.270411351848372));
#46807=CARTESIAN_POINT('Ctrl Pts',(-0.092254395683996,-0.11893262173657,
-0.26246406054042));
#46808=CARTESIAN_POINT('Ctrl Pts',(0.0500466135038247,-0.141954846740938,
-0.254516769232468));
#46809=CARTESIAN_POINT('Ctrl Pts',(0.146445615989062,-0.0347782057238245,
-0.246569477924518));
#46810=CARTESIAN_POINT('Ctrl Pts',(0.108526885952636,0.104296486333508,
-0.238622186616565));
#46811=CARTESIAN_POINT('Ctrl Pts',(-0.0289310835603638,0.147711998300275,
-0.230674895308614));
#46812=CARTESIAN_POINT('Ctrl Pts',(-0.139853895164789,0.0556482707761755,
-0.222727604000662));
#46813=CARTESIAN_POINT('Ctrl Pts',(-0.122504802193644,-0.0874552198327828,
-0.214780312692711));
#46814=CARTESIAN_POINT('Ctrl Pts',(0.00720386637860762,-0.150346088594642,
-0.206833021384759));
#46815=CARTESIAN_POINT('Ctrl Pts',(0.13030525617202,-0.075341769476037,
-0.198885730076808));
#46816=CARTESIAN_POINT('Ctrl Pts',(0.133892610659253,0.0687648955194049,
-0.190938438768856));
#46817=CARTESIAN_POINT('Ctrl Pts',(0.014675661361578,0.149801425434866,
-0.182991147460905));
#46818=CARTESIAN_POINT('Ctrl Pts',(-0.11800158480147,0.0934423237107693,
-0.175043856152952));
#46819=CARTESIAN_POINT('Ctrl Pts',(-0.142449540356412,-0.0486206807040808,
-0.167096564845001));
#46820=CARTESIAN_POINT('Ctrl Pts',(-0.0362449020418857,-0.146089525550903,
-0.159149273537049));
#46821=CARTESIAN_POINT('Ctrl Pts',(0.103203015007595,-0.109567233280859,
-0.151201982229098));
#46822=CARTESIAN_POINT('Ctrl Pts',(0.147994675645917,0.027448479198832,
-0.143254690921146));
#46823=CARTESIAN_POINT('Ctrl Pts',(0.0570478139685668,0.139288875912043,
-0.135307399613195));
#46824=CARTESIAN_POINT('Ctrl Pts',(-0.0862224217148439,0.123375558151578,
-0.127360108305243));
#46825=CARTESIAN_POINT('Ctrl Pts',(-0.150410795001361,-0.00569590911631693,
-0.119412816997291));
#46826=CARTESIAN_POINT('Ctrl Pts',(-0.0766445274621928,-0.12954330722548,
-0.11146552568934));
#46827=CARTESIAN_POINT('Ctrl Pts',(0.0674187564615154,-0.134575264392198,
-0.103518234381388));
#46828=CARTESIAN_POINT('Ctrl Pts',(0.149646942931058,-0.0161772797550832,
-0.0955709430734365));
#46829=CARTESIAN_POINT('Ctrl Pts',(0.0946204674793121,0.117059178191346,
-0.0876236517654852));
#46830=CARTESIAN_POINT('Ctrl Pts',(-0.0471891212084412,0.142928971075017,
-0.0796763604575334));
#46831=CARTESIAN_POINT('Ctrl Pts',(-0.145720146807228,0.0377097379155704,
-0.0717290691495822));
#46832=CARTESIAN_POINT('Ctrl Pts',(-0.110593905137976,-0.10210255282505,
-0.0637817778416302));
#46833=CARTESIAN_POINT('Ctrl Pts',(0.0259580684157336,-0.148256045218673,
-0.0558344865336788));
#46834=CARTESIAN_POINT('Ctrl Pts',(0.138719431502144,-0.0584538229284914,
-0.047887195225727));
#46835=CARTESIAN_POINT('Ctrl Pts',(0.124215712985446,0.0850041361652265,
-0.0399399039177754));
#46836=CARTESIAN_POINT('Ctrl Pts',(-0.004152737614071,0.150416188445784,
-0.0319926126098237));
#46837=CARTESIAN_POINT('Ctrl Pts',(-0.128834969429613,0.0780250473313025,
-0.0240453213018721));
#46838=CARTESIAN_POINT('Ctrl Pts',(-0.135110406641513,-0.0662414518576971,
-0.0160980299939207));
#46839=CARTESIAN_POINT('Ctrl Pts',(-0.0570343146549906,-0.121442316265599,
-0.0107998357886196));
#46840=CARTESIAN_POINT('Ctrl Pts',(-0.0149499840092685,-0.126419096572166,
-0.00815073868596909));
#46841=CARTESIAN_POINT('Ctrl Pts',(0.120439183586217,-0.0649267562880324,
-2.94314926131403));
#46842=CARTESIAN_POINT('Ctrl Pts',(0.14205299948483,-0.024833110927659,
-2.94050016421138));
#46843=CARTESIAN_POINT('Ctrl Pts',(0.141715520135631,0.0779399629980596,
-2.93520197000608));
#46844=CARTESIAN_POINT('Ctrl Pts',(0.0109341606128859,0.161520108869991,
-2.92725467869813));
#46845=CARTESIAN_POINT('Ctrl Pts',(-0.129750457406967,0.0965515110554682,
-2.91930738739018));
#46846=CARTESIAN_POINT('Ctrl Pts',(-0.151491649088109,-0.0567683102589726,
-2.91136009608222));
#46847=CARTESIAN_POINT('Ctrl Pts',(-0.0342549406055127,-0.158127703177675,
-2.90341280477428));
#46848=CARTESIAN_POINT('Ctrl Pts',(0.114383078266682,-0.114398680790832,
-2.89546551346632));
#46849=CARTESIAN_POINT('Ctrl Pts',(0.15811949456322,0.0342255899845588,
-2.88751822215837));
#46850=CARTESIAN_POINT('Ctrl Pts',(0.0568264098997039,0.151474208223123,
-2.87957093085042));
#46851=CARTESIAN_POINT('Ctrl Pts',(-0.0965845537755583,0.129784753121562,
-2.87162363954247));
#46852=CARTESIAN_POINT('Ctrl Pts',(-0.161410900544422,-0.0109370243537351,
-2.86367634823452));
#46853=CARTESIAN_POINT('Ctrl Pts',(-0.0781928975915483,-0.141629800004137,
-2.85572905692656));
#46854=CARTESIAN_POINT('Ctrl Pts',(0.0767421044758823,-0.14242063978591,
-2.84778176561862));
#46855=CARTESIAN_POINT('Ctrl Pts',(0.161290583296262,-0.0125860262202751,
-2.83983447431066));
#46856=CARTESIAN_POINT('Ctrl Pts',(0.0979056475321585,0.128792635178867,
-2.83188718300271));
#46857=CARTESIAN_POINT('Ctrl Pts',(-0.0552768338809414,0.152044439313014,
-2.82393989169476));
#46858=CARTESIAN_POINT('Ctrl Pts',(-0.157760256221094,0.0358434460527866,
-2.81599260038681));
#46859=CARTESIAN_POINT('Ctrl Pts',(-0.115548312366974,-0.113232669402329,
-2.80804530907885));
#46860=CARTESIAN_POINT('Ctrl Pts',(0.0326428107524121,-0.158453445448113,
-2.80009801777091));
#46861=CARTESIAN_POINT('Ctrl Pts',(0.15089443925921,-0.05834310056466,-2.79215072646295));
#46862=CARTESIAN_POINT('Ctrl Pts',(0.130747938827138,0.095278672194432,
-2.784203435155));
#46863=CARTESIAN_POINT('Ctrl Pts',(-0.00931861788340384,0.161512265598379,
-2.77625614384705));
#46864=CARTESIAN_POINT('Ctrl Pts',(-0.140838277991704,0.0796092223769108,
-2.7683088525391));
#46865=CARTESIAN_POINT('Ctrl Pts',(-0.14318317195546,-0.0753102120683318,
-2.76036156123115));
#46866=CARTESIAN_POINT('Ctrl Pts',(-0.0142025985168282,-0.161156243851845,
-2.75241426992319));
#46867=CARTESIAN_POINT('Ctrl Pts',(0.127804386320586,-0.0991921751552476,
-2.74446697861524));
#46868=CARTESIAN_POINT('Ctrl Pts',(0.152591096121994,0.0537494757885291,
-2.73651968730729));
#46869=CARTESIAN_POINT('Ctrl Pts',(0.0374235307972619,0.157392909948435,
-2.72857239599934));
#46870=CARTESIAN_POINT('Ctrl Pts',(-0.112068338247225,0.116677917050738,
-2.72062510469139));
#46871=CARTESIAN_POINT('Ctrl Pts',(-0.158772800645446,-0.0310523193655248,
-2.71267781338343));
#46872=CARTESIAN_POINT('Ctrl Pts',(-0.0598532208020871,-0.150301832064811,
-2.70473052207548));
#46873=CARTESIAN_POINT('Ctrl Pts',(0.0939628395432803,-0.131696748434227,
-2.69678323076753));
#46874=CARTESIAN_POINT('Ctrl Pts',(0.16159758634093,0.00769862660697697,
-2.68883593945958));
#46875=CARTESIAN_POINT('Ctrl Pts',(0.0810174396286684,0.140032936264449,
-2.68088864815163));
#46876=CARTESIAN_POINT('Ctrl Pts',(-0.0738706931061093,0.143931127498383,
-2.67294135684368));
#46877=CARTESIAN_POINT('Ctrl Pts',(-0.161005729026759,0.0158178375083437,
-2.66499406553573));
#46878=CARTESIAN_POINT('Ctrl Pts',(-0.10046871412908,-0.126803336880895,
-2.65704677422778));
#46879=CARTESIAN_POINT('Ctrl Pts',(0.0522167053515813,-0.153122383880087,
-2.64909948291982));
#46880=CARTESIAN_POINT('Ctrl Pts',(0.157009742288698,-0.0389998665295485,
-2.64115219161187));
#46881=CARTESIAN_POINT('Ctrl Pts',(0.117795787782758,0.110892746126725,
-2.63320490030392));
#46882=CARTESIAN_POINT('Ctrl Pts',(-0.0294587045649093,0.159076187684537,
-2.62525760899597));
#46883=CARTESIAN_POINT('Ctrl Pts',(-0.149694112909478,0.061357324934615,
-2.61731031768802));
#46884=CARTESIAN_POINT('Ctrl Pts',(-0.132632315853919,-0.0926375601692635,
-2.60936302638006));
#46885=CARTESIAN_POINT('Ctrl Pts',(0.00607786107815708,-0.161666658181589,
-2.60141573507212));
#46886=CARTESIAN_POINT('Ctrl Pts',(0.139213514572923,-0.0824175110224898,
-2.59346844376416));
#46887=CARTESIAN_POINT('Ctrl Pts',(0.144664610984601,0.0724237467379446,
-2.58552115245621));
#46888=CARTESIAN_POINT('Ctrl Pts',(0.0174314860702634,0.160839025290102,
-2.57757386114826));
#46889=CARTESIAN_POINT('Ctrl Pts',(-0.125789537612448,0.101735151202198,
-2.56962656984031));
#46890=CARTESIAN_POINT('Ctrl Pts',(-0.153638275457792,-0.0506786846439741,
-2.56167927853235));
#46891=CARTESIAN_POINT('Ctrl Pts',(-0.0405722809007601,-0.156610787576711,
-2.5537319872244));
#46892=CARTESIAN_POINT('Ctrl Pts',(0.109706003946886,-0.118901814371748,
-2.54578469591645));
#46893=CARTESIAN_POINT('Ctrl Pts',(0.159363579905122,0.0278621277491786,
-2.5378374046085));
#46894=CARTESIAN_POINT('Ctrl Pts',(0.0628552597017324,0.149071342285214,
-2.52989011330055));
#46895=CARTESIAN_POINT('Ctrl Pts',(-0.09130296625958,0.133554547339616,
-2.5219428219926));
#46896=CARTESIAN_POINT('Ctrl Pts',(-0.161719474737566,-0.0044564844320954,
-2.51399553068464));
#46897=CARTESIAN_POINT('Ctrl Pts',(-0.0838092954875492,-0.138380095218816,
-2.5060482393767));
#46898=CARTESIAN_POINT('Ctrl Pts',(0.0709695182955605,-0.145383548710932,
-2.49810094806874));
#46899=CARTESIAN_POINT('Ctrl Pts',(0.160656149485851,-0.0190433819283141,
-2.49015365676079));
#46900=CARTESIAN_POINT('Ctrl Pts',(0.102991358993371,0.124763090437783,
-2.48220636545284));
#46901=CARTESIAN_POINT('Ctrl Pts',(-0.0491355682880311,0.154138718990071,
-2.47425907414489));
#46902=CARTESIAN_POINT('Ctrl Pts',(-0.156196085938658,0.0421406158038896,
-2.46631178283693));
#46903=CARTESIAN_POINT('Ctrl Pts',(-0.119995885602437,-0.108508231030529,
-2.45836449152899));
#46904=CARTESIAN_POINT('Ctrl Pts',(0.0262627494478528,-0.159634948411453,
-2.45041720022103));
#46905=CARTESIAN_POINT('Ctrl Pts',(0.148433582812218,-0.0643468744883253,
-2.44246990891309));
#46906=CARTESIAN_POINT('Ctrl Pts',(0.134463350161716,0.0899591920049057,
-2.43452261760513));
#46907=CARTESIAN_POINT('Ctrl Pts',(-0.00283465969473679,0.161756030698404,
-2.42657532629718));
#46908=CARTESIAN_POINT('Ctrl Pts',(-0.137532762001164,0.0851926530824045,
-2.41862803498923));
#46909=CARTESIAN_POINT('Ctrl Pts',(-0.146087868389377,-0.069508153998907,
-2.41068074368127));
#46910=CARTESIAN_POINT('Ctrl Pts',(-0.020653363009408,-0.160457120001854,
-2.40273345237332));
#46911=CARTESIAN_POINT('Ctrl Pts',(0.123724098564309,-0.104237211193206,
-2.39478616106537));
#46912=CARTESIAN_POINT('Ctrl Pts',(0.154623664158228,0.0475875114412515,
-2.38683886975742));
#46913=CARTESIAN_POINT('Ctrl Pts',(0.0437047135457649,0.155765679072029,
-2.37889157844947));
#46914=CARTESIAN_POINT('Ctrl Pts',(-0.107299547811519,0.121077891467977,
-2.37094428714151));
#46915=CARTESIAN_POINT('Ctrl Pts',(-0.159890265917922,-0.0246607304754712,
-2.36299699583357));
#46916=CARTESIAN_POINT('Ctrl Pts',(-0.0658320193152775,-0.147780898616028,
-2.35504970452561));
#46917=CARTESIAN_POINT('Ctrl Pts',(0.0886063725192689,-0.135358632941768,
-2.34710241321766));
#46918=CARTESIAN_POINT('Ctrl Pts',(0.161776322388465,0.00121254993757108,
-2.33915512190971));
#46919=CARTESIAN_POINT('Ctrl Pts',(0.0865674447129999,0.136671600117762,
-2.33120783060176));
#46920=CARTESIAN_POINT('Ctrl Pts',(-0.0680398007854702,0.146777499201892,
-2.32326053929381));
#46921=CARTESIAN_POINT('Ctrl Pts',(-0.160241956850158,0.0222612674329143,
-2.31531324798586));
#46922=CARTESIAN_POINT('Ctrl Pts',(-0.105472582533561,-0.122672666460744,
-2.30736595667791));
#46923=CARTESIAN_POINT('Ctrl Pts',(0.0460346697578994,-0.155093062201921,
-2.29941866536995));
#46924=CARTESIAN_POINT('Ctrl Pts',(0.155319610253441,-0.0452644168592387,
-2.291471374062));
#46925=CARTESIAN_POINT('Ctrl Pts',(0.122147723174673,0.106080075820726,
-2.28352408275405));
#46926=CARTESIAN_POINT('Ctrl Pts',(-0.0230562319120901,0.160129506752827,
-2.2755767914461));
#46927=CARTESIAN_POINT('Ctrl Pts',(-0.147113355322838,0.0673105448540142,
-2.26762950013814));
#46928=CARTESIAN_POINT('Ctrl Pts',(-0.13624030566074,-0.0872446438261734,
-2.2596822088302));
#46929=CARTESIAN_POINT('Ctrl Pts',(-0.000409681739256192,-0.16178034776746,
-2.25173491752224));
#46930=CARTESIAN_POINT('Ctrl Pts',(0.135796696156851,-0.0879335321465694,
-2.2437876262143));
#46931=CARTESIAN_POINT('Ctrl Pts',(0.147452371807367,0.0665646062954607,
-2.23584033490634));
#46932=CARTESIAN_POINT('Ctrl Pts',(0.0238669335270067,0.160010681665022,
-2.22789304359839));
#46933=CARTESIAN_POINT('Ctrl Pts',(-0.121608899846648,0.106697348800126,
-2.21994575229043));
#46934=CARTESIAN_POINT('Ctrl Pts',(-0.155546865924041,-0.0444771993733432,
-2.21199846098249));
#46935=CARTESIAN_POINT('Ctrl Pts',(-0.0468195689190186,-0.154857924334291,
-2.20405116967453));
#46936=CARTESIAN_POINT('Ctrl Pts',(0.104849937673813,-0.123205273152918,
-2.19610387836658));
#46937=CARTESIAN_POINT('Ctrl Pts',(0.160352646860941,0.0214494150870821,
-2.18815658705863));
#46938=CARTESIAN_POINT('Ctrl Pts',(0.068782302441517,0.146431020052896,
-2.18020929575068));
#46939=CARTESIAN_POINT('Ctrl Pts',(-0.0858741428449303,0.137108279668065,
-2.17226200444273));
#46940=CARTESIAN_POINT('Ctrl Pts',(-0.161768106430643,0.00203187222333996,
-2.16431471313477));
#46941=CARTESIAN_POINT('Ctrl Pts',(-0.0892907780255418,-0.134908138088409,
-2.15636742182682));
#46942=CARTESIAN_POINT('Ctrl Pts',(0.065082718856964,-0.148112418348608,
-2.14842013051887));
#46943=CARTESIAN_POINT('Ctrl Pts',(0.15976331770074,-0.0254701998449192,
-2.14047283921092));
#46944=CARTESIAN_POINT('Ctrl Pts',(0.107911386844908,0.120532905681794,
-2.13252554790297));
#46945=CARTESIAN_POINT('Ctrl Pts',(-0.0429152568883603,0.155985029695461,
-2.12457825659502));
#46946=CARTESIAN_POINT('Ctrl Pts',(-0.154380667736248,0.048370013357431,
-2.11663096528707));
#46947=CARTESIAN_POINT('Ctrl Pts',(-0.124250435068012,-0.103609257058902,
-2.10868367397912));
#46948=CARTESIAN_POINT('Ctrl Pts',(0.0198404415629177,-0.160559663805939,
-2.10073638267116));
#46949=CARTESIAN_POINT('Ctrl Pts',(0.145733961413755,-0.0702471440952718,
-2.09278909136321));
#46950=CARTESIAN_POINT('Ctrl Pts',(0.137962467690555,0.0844950073768885,
-2.08484180005526));
#46951=CARTESIAN_POINT('Ctrl Pts',(0.00365385840641593,0.161739599608858,
-2.07689450874731));
#46952=CARTESIAN_POINT('Ctrl Pts',(-0.134006015255314,0.0906390458813432,
-2.06894721743935));
#46953=CARTESIAN_POINT('Ctrl Pts',(-0.148757572459151,-0.0635942874710312,
-2.0609999261314));
#46954=CARTESIAN_POINT('Ctrl Pts',(-0.0270709051811781,-0.159499889829302,
-2.05305263482345));
#46955=CARTESIAN_POINT('Ctrl Pts',(0.119444792155413,-0.109114574598621,
-2.0451053435155));
#46956=CARTESIAN_POINT('Ctrl Pts',(0.15640750945962,0.04134899935339,-2.03715805220755));
#46957=CARTESIAN_POINT('Ctrl Pts',(0.0499155942801435,0.153887888446583,
-2.0292107608996));
#46958=CARTESIAN_POINT('Ctrl Pts',(-0.102358158724142,0.125283103830848,
-2.02126346959164));
#46959=CARTESIAN_POINT('Ctrl Pts',(-0.160750536772648,-0.0182294731189203,
-2.0133161782837));
#46960=CARTESIAN_POINT('Ctrl Pts',(-0.0717049225281518,-0.145022249493378,
-2.00536888697574));
#46961=CARTESIAN_POINT('Ctrl Pts',(0.0831073760915768,-0.138802783841179,
-1.99742159566779));
#46962=CARTESIAN_POINT('Ctrl Pts',(0.161694830168414,-0.00527547720076154,
-1.98947430435984));
#46963=CARTESIAN_POINT('Ctrl Pts',(0.0919782001481242,0.133090418364356,
-1.98152701305189));
#46964=CARTESIAN_POINT('Ctrl Pts',(-0.0620994617966974,0.149387769269938,
-1.97357972174394));
#46965=CARTESIAN_POINT('Ctrl Pts',(-0.159220424537894,0.0286688885878118,
-1.96563243043599));
#46966=CARTESIAN_POINT('Ctrl Pts',(-0.110306791082952,-0.118344668675314,
-1.95768513912803));
#46967=CARTESIAN_POINT('Ctrl Pts',(0.03977858425274,-0.156814262736958,
-1.94973784782008));
#46968=CARTESIAN_POINT('Ctrl Pts',(0.153379636013345,-0.0514561562818434,
-1.94179055651213));
#46969=CARTESIAN_POINT('Ctrl Pts',(0.126303175608487,0.101096768465166,
-1.93384326520418));
#46970=CARTESIAN_POINT('Ctrl Pts',(-0.0166166717349957,0.160925246569142,
-1.92589597389623));
#46971=CARTESIAN_POINT('Ctrl Pts',(-0.144295955853084,0.0731554911632232,
-1.91794868258828));
#46972=CARTESIAN_POINT('Ctrl Pts',(-0.139629143627699,-0.0817113885127615,
-1.91000139128032));
#46973=CARTESIAN_POINT('Ctrl Pts',(-0.00689656555560029,-0.161633802610794,
-1.90205409997237));
#46974=CARTESIAN_POINT('Ctrl Pts',(0.132161439477111,-0.0933081061763968,
-1.89410680866442));
#46975=CARTESIAN_POINT('Ctrl Pts',(0.150002945415843,0.0605983921359247,
-1.88615951735647));
#46976=CARTESIAN_POINT('Ctrl Pts',(0.0302639893905353,0.158924949926238,
-1.87821222604852));
#46977=CARTESIAN_POINT('Ctrl Pts',(-0.117232645856884,0.111487916422733,
-1.87026493474057));
#46978=CARTESIAN_POINT('Ctrl Pts',(-0.157205248629181,-0.0382041694887514,
-1.86231764343261));
#46979=CARTESIAN_POINT('Ctrl Pts',(-0.0529915444618639,-0.152855961540379,
-1.85437035212466));
#46980=CARTESIAN_POINT('Ctrl Pts',(0.0998252131124366,-0.127310547834593,
-1.84642306081671));
#46981=CARTESIAN_POINT('Ctrl Pts',(0.161083775628675,0.0150021995753526,
-1.83847576950876));
#46982=CARTESIAN_POINT('Ctrl Pts',(0.0745987041484787,0.143555153520365,
-1.83052847820081));
#46983=CARTESIAN_POINT('Ctrl Pts',(-0.0803071850044249,0.140441463961156,
-1.82258118689286));
#46984=CARTESIAN_POINT('Ctrl Pts',(-0.161556523072208,0.0085169604734811,
-1.81463389558491));
#46985=CARTESIAN_POINT('Ctrl Pts',(-0.0946286302465571,-0.131219172000695,
-1.80668660427695));
#46986=CARTESIAN_POINT('Ctrl Pts',(0.0590912294185051,-0.150603039042038,
-1.798739312969));
#46987=CARTESIAN_POINT('Ctrl Pts',(0.158613495703762,-0.0318560472048982,
-1.79079202166105));
#46988=CARTESIAN_POINT('Ctrl Pts',(0.112657831857984,0.116108835511971,
-1.7828447303531));
#46989=CARTESIAN_POINT('Ctrl Pts',(-0.036625913365931,0.157580427823379,
-1.77489743904515));
#46990=CARTESIAN_POINT('Ctrl Pts',(-0.15231691768219,0.0545216044397509,
-1.76695014773719));
#46991=CARTESIAN_POINT('Ctrl Pts',(-0.128305119219744,-0.0985436205185058,
-1.75900285642925));
#46992=CARTESIAN_POINT('Ctrl Pts',(0.0133862189721914,-0.16122610801144,
-1.75105556512129));
#46993=CARTESIAN_POINT('Ctrl Pts',(0.142799916981525,-0.0760344163715165,
-1.74310827381334));
#46994=CARTESIAN_POINT('Ctrl Pts',(0.141239663164244,0.0788949067566377,
-1.73516098250539));
#46995=CARTESIAN_POINT('Ctrl Pts',(0.0101364990266846,0.161462999322971,
-1.72721369119744));
#46996=CARTESIAN_POINT('Ctrl Pts',(-0.13026371067837,0.0959396395823433,
-1.71926639988948));
#46997=CARTESIAN_POINT('Ctrl Pts',(-0.151187989810213,-0.0575781251868712,
-1.71131910858153));
#46998=CARTESIAN_POINT('Ctrl Pts',(-0.0334449019524261,-0.15828609318661,
-1.70337181727358));
#46999=CARTESIAN_POINT('Ctrl Pts',(0.11497335063763,-0.11381641975587,-1.69542452596563));
#47000=CARTESIAN_POINT('Ctrl Pts',(0.157939762595976,0.0350439745750224,
-1.68747723465768));
#47001=CARTESIAN_POINT('Ctrl Pts',(0.0560461823707901,0.151762558638644,
-1.67952994334973));
#47002=CARTESIAN_POINT('Ctrl Pts',(-0.097252119545145,0.129286789761617,
-1.67158265204178));
#47003=CARTESIAN_POINT('Ctrl Pts',(-0.161352229406179,-0.0117688924093824,
-1.66363536073382));
#47004=CARTESIAN_POINT('Ctrl Pts',(-0.0774624834741187,-0.142030322174209,
-1.65568806942587));
#47005=CARTESIAN_POINT('Ctrl Pts',(0.0774746957713786,-0.142023660979501,
-1.64774077811792));
#47006=CARTESIAN_POINT('Ctrl Pts',(0.161353240766724,-0.0117550183735887,
-1.63979348680997));
#47007=CARTESIAN_POINT('Ctrl Pts',(0.0972410023641809,0.129295151580007,
-1.63184619550202));
#47008=CARTESIAN_POINT('Ctrl Pts',(-0.0560592315808636,0.151757738904646,
-1.62389890419407));
#47009=CARTESIAN_POINT('Ctrl Pts',(-0.157942775294506,0.0350303938767022,
-1.61595161288612));
#47010=CARTESIAN_POINT('Ctrl Pts',(-0.114963563622508,-0.113826305404776,
-1.60800432157816));
#47011=CARTESIAN_POINT('Ctrl Pts',(0.0334585121770555,-0.158283216816521,
-1.60005703027021));
#47012=CARTESIAN_POINT('Ctrl Pts',(0.15119294014952,-0.0575651249614849,
-1.59210973896226));
#47013=CARTESIAN_POINT('Ctrl Pts',(0.130255460755053,0.0959508400503948,
-1.58416244765431));
#47014=CARTESIAN_POINT('Ctrl Pts',(-0.0101503825061297,0.161462127131619,
-1.57621515634636));
#47015=CARTESIAN_POINT('Ctrl Pts',(-0.141246446479757,0.0788827618667677,
-1.5682678650384));
#47016=CARTESIAN_POINT('Ctrl Pts',(-0.142793378577391,-0.0760466948482432,
-1.56032057373045));
#47017=CARTESIAN_POINT('Ctrl Pts',(-0.0133723557750614,-0.161227258439486,
-1.5523732824225));
#47018=CARTESIAN_POINT('Ctrl Pts',(0.128313592092439,-0.0985325877424461,
-1.54442599111455));
#47019=CARTESIAN_POINT('Ctrl Pts',(0.152312229038119,0.0545347013224366,
-1.5364786998066));
#47020=CARTESIAN_POINT('Ctrl Pts',(0.0366123635594306,0.157583576547431,
-1.52853140849865));
#47021=CARTESIAN_POINT('Ctrl Pts',(-0.112667815146693,0.116099148114697,
-1.5205841171907));
#47022=CARTESIAN_POINT('Ctrl Pts',(-0.158610755951326,-0.0318696855873517,
-1.51263682588274));
#47023=CARTESIAN_POINT('Ctrl Pts',(-0.059078279484957,-0.150608119488907,
-1.50468953457479));
#47024=CARTESIAN_POINT('Ctrl Pts',(0.0946399128755136,-0.131211034801968,
-1.49674224326684));
#47025=CARTESIAN_POINT('Ctrl Pts',(0.161555790137746,0.00853085200062658,
-1.48879495195889));
#47026=CARTESIAN_POINT('Ctrl Pts',(0.0802951087430872,0.140448368715423,
-1.48084766065094));
#47027=CARTESIAN_POINT('Ctrl Pts',(-0.0746110475700918,0.143548738564228,
-1.47290036934299));
#47028=CARTESIAN_POINT('Ctrl Pts',(-0.161085065008549,0.0149883486108072,
-1.46495307803503));
#47029=CARTESIAN_POINT('Ctrl Pts',(-0.0998142658506054,-0.127319130909666,
-1.45700578672708));
#47030=CARTESIAN_POINT('Ctrl Pts',(0.0530046877002974,-0.152851404457669,
-1.44905849541913));
#47031=CARTESIAN_POINT('Ctrl Pts',(0.157208533062154,-0.0381906519364803,
-1.44111120411118));
#47032=CARTESIAN_POINT('Ctrl Pts',(0.117223059051512,0.111497996347438,
-1.43316391280323));
#47033=CARTESIAN_POINT('Ctrl Pts',(-0.0302776545594956,0.158922347066935,
-1.42521662149528));
#47034=CARTESIAN_POINT('Ctrl Pts',(-0.150008155459448,0.0605854937963053,
-1.41726933018732));
#47035=CARTESIAN_POINT('Ctrl Pts',(-0.13215341582115,-0.0933194698318111,
-1.40932203887937));
#47036=CARTESIAN_POINT('Ctrl Pts',(0.00691046373367479,-0.161633209006915,
-1.40137474757142));
#47037=CARTESIAN_POINT('Ctrl Pts',(0.139636169126457,-0.0816993820942073,
-1.39342745626347));
#47038=CARTESIAN_POINT('Ctrl Pts',(0.14428966498996,0.0731678982886138,
-1.38548016495552));
#47039=CARTESIAN_POINT('Ctrl Pts',(0.01660283439572,0.160926674771202,-1.37753287364757));
#47040=CARTESIAN_POINT('Ctrl Pts',(-0.126311868022924,0.101085907818286,
-1.36958558233961));
#47041=CARTESIAN_POINT('Ctrl Pts',(-0.1533752109502,-0.0514693445544957,
-1.36163829103166));
#47042=CARTESIAN_POINT('Ctrl Pts',(-0.0397651003138635,-0.156817682548608,
-1.35369099972371));
#47043=CARTESIAN_POINT('Ctrl Pts',(0.11031696663014,-0.118335183425778,
-1.34574370841576));
#47044=CARTESIAN_POINT('Ctrl Pts',(0.159217958833437,0.028682579169278,
-1.33779641710781));
#47045=CARTESIAN_POINT('Ctrl Pts',(0.0620866163479071,0.149393108386416,
-1.32984912579986));
#47046=CARTESIAN_POINT('Ctrl Pts',(-0.0919896436874009,0.133082509057925,
-1.3219018344919));
#47047=CARTESIAN_POINT('Ctrl Pts',(-0.161694375954805,-0.00528938063232889,
-1.31395454318395));
#47048=CARTESIAN_POINT('Ctrl Pts',(-0.0830954407230262,-0.138809929378031,
-1.306007251876));
#47049=CARTESIAN_POINT('Ctrl Pts',(0.0717173921098091,-0.145016083355798,
-1.29805996056805));
#47050=CARTESIAN_POINT('Ctrl Pts',(0.160752103653288,-0.0182156507962345,
-1.2901126692601));
#47051=CARTESIAN_POINT('Ctrl Pts',(0.102347385784237,0.125291904710641,
-1.28216537795215));
#47052=CARTESIAN_POINT('Ctrl Pts',(-0.0499288262609556,0.153883595847937,
-1.2742180866442));
#47053=CARTESIAN_POINT('Ctrl Pts',(-0.156411064306094,0.0413355503836927,
-1.26627079533624));
#47054=CARTESIAN_POINT('Ctrl Pts',(-0.119435409415436,-0.109124844745158,
-1.25832350402829));
#47055=CARTESIAN_POINT('Ctrl Pts',(0.0270846197985837,-0.15949756152761,
-1.25037621272034));
#47056=CARTESIAN_POINT('Ctrl Pts',(0.148763040111663,-0.0635814962046623,
-1.24242892141239));
#47057=CARTESIAN_POINT('Ctrl Pts',(0.133998221093683,0.0906505681538529,
-1.23448163010444));
#47058=CARTESIAN_POINT('Ctrl Pts',(-0.00366776569351205,0.161739284831192,
-1.22653433879648));
#47059=CARTESIAN_POINT('Ctrl Pts',(-0.137969732547029,0.0844831442584205,
-1.21858704748853));
#47060=CARTESIAN_POINT('Ctrl Pts',(-0.145727920621714,-0.0702596748793999,
-1.21063975618058));
#47061=CARTESIAN_POINT('Ctrl Pts',(-0.019826635646634,-0.160561369207613,
-1.20269246487263));
#47062=CARTESIAN_POINT('Ctrl Pts',(0.124259343528249,-0.103598572909169,
-1.19474517356468));
#47063=CARTESIAN_POINT('Ctrl Pts',(0.154376508033714,0.0483832877159527,
-1.18679788225673));
#47064=CARTESIAN_POINT('Ctrl Pts',(0.0429018442401126,0.155988719219323,
-1.17885059094878));
#47065=CARTESIAN_POINT('Ctrl Pts',(-0.107921750558149,0.120523626394796,
-1.17090329964082));
#47066=CARTESIAN_POINT('Ctrl Pts',(-0.159761127035922,-0.0254839371192833,
-1.16295600833287));
#47067=CARTESIAN_POINT('Ctrl Pts',(-0.0650699830591519,-0.148118013987393,
-1.15500871702492));
#47068=CARTESIAN_POINT('Ctrl Pts',(0.0893023778727434,-0.134900459855264,
-1.14706142571697));
#47069=CARTESIAN_POINT('Ctrl Pts',(0.161767931120567,0.00204578196761214,
-1.13911413440902));
#47070=CARTESIAN_POINT('Ctrl Pts',(0.0858623531693627,0.137115663113691,
-1.13116684310107));
#47071=CARTESIAN_POINT('Ctrl Pts',(-0.0687948931681688,0.146425105213786,
-1.12321955179312));
#47072=CARTESIAN_POINT('Ctrl Pts',(-0.160354490612175,0.0214356269653556,
-1.11527226048516));
#47073=CARTESIAN_POINT('Ctrl Pts',(-0.104839343388522,-0.123214288297872,
-1.10732496917721));
#47074=CARTESIAN_POINT('Ctrl Pts',(0.0468328843205382,-0.154853897946118,
-1.09937767786926));
#47075=CARTESIAN_POINT('Ctrl Pts',(0.155550689754317,-0.0444638243951627,
-1.09143038656131));
#47076=CARTESIAN_POINT('Ctrl Pts',(0.121599724945644,0.106707805038019,
-1.08348309525336));
#47077=CARTESIAN_POINT('Ctrl Pts',(-0.0238806920770757,0.160008628857346,
-1.0755358039454));
#47078=CARTESIAN_POINT('Ctrl Pts',(-0.147458094869793,0.0665519272467647,
-1.06758851263745));
#47079=CARTESIAN_POINT('Ctrl Pts',(-0.135789134624223,-0.0879452084021196,
-1.0596412213295));
#47080=CARTESIAN_POINT('Ctrl Pts',(0.000423592542104506,-0.161780311942603,
-1.05169393002155));
#47081=CARTESIAN_POINT('Ctrl Pts',(0.136247806953129,-0.0872329287789347,
-1.0437466387136));
#47082=CARTESIAN_POINT('Ctrl Pts',(0.147107567031384,0.0673231942572166,
-1.03579934740565));
#47083=CARTESIAN_POINT('Ctrl Pts',(0.023042462971293,0.160131488668233,
-1.0278520560977));
#47084=CARTESIAN_POINT('Ctrl Pts',(-0.122156844097886,0.106069572465116,
-1.01990476478974));
#47085=CARTESIAN_POINT('Ctrl Pts',(-0.155315717584476,-0.0452777719649154,
-1.01195747348179));
#47086=CARTESIAN_POINT('Ctrl Pts',(-0.0460213337946129,-0.155097019954134,
-1.00401018217384));
#47087=CARTESIAN_POINT('Ctrl Pts',(0.105483130244754,-0.122663596868249,
-0.996062890865889));
#47088=CARTESIAN_POINT('Ctrl Pts',(0.160240042106027,0.022275045875293,
-0.988115599557937));
#47089=CARTESIAN_POINT('Ctrl Pts',(0.0680271797607449,0.146783349112517,
-0.980168308249986));
#47090=CARTESIAN_POINT('Ctrl Pts',(-0.0865791962028742,0.13666415604595,
-0.972221016942034));
#47091=CARTESIAN_POINT('Ctrl Pts',(-0.161776426052429,0.00119863947484806,
-0.964273725634083));
#47092=CARTESIAN_POINT('Ctrl Pts',(-0.0885947332782831,-0.135366251326679,
-0.956326434326131));
#47093=CARTESIAN_POINT('Ctrl Pts',(0.0658447261231557,-0.147775237454231,
-0.948379143018179));
#47094=CARTESIAN_POINT('Ctrl Pts',(0.159892385798223,-0.0246469821000468,
-0.940431851710227));
#47095=CARTESIAN_POINT('Ctrl Pts',(0.107289136441681,0.121087117252359,
-0.932484560402278));
#47096=CARTESIAN_POINT('Ctrl Pts',(-0.0437181070127741,0.155761920513673,
-0.924537269094323));
#47097=CARTESIAN_POINT('Ctrl Pts',(-0.154627755434431,0.0475742158337616,
-0.916589977786374));
#47098=CARTESIAN_POINT('Ctrl Pts',(-0.123715135192255,-0.104247849317143,
-0.908642686478421));
#47099=CARTESIAN_POINT('Ctrl Pts',(0.020667159958694,-0.160455343513793,
-0.90069539517047));
#47100=CARTESIAN_POINT('Ctrl Pts',(0.146093844560002,-0.0694955922671763,
-0.892748103862517));
#47101=CARTESIAN_POINT('Ctrl Pts',(0.137525436138657,0.0852044786250095,
-0.884800812554568));
#47102=CARTESIAN_POINT('Ctrl Pts',(0.00282075097081221,0.161756273840766,
-0.876853521246614));
#47103=CARTESIAN_POINT('Ctrl Pts',(-0.134471084873137,0.0899476297404762,
-0.868906229938664));
#47104=CARTESIAN_POINT('Ctrl Pts',(-0.148428049349295,-0.0643596374232403,
-0.86095893863071));
#47105=CARTESIAN_POINT('Ctrl Pts',(-0.0262490230201646,-0.159637206043499,
-0.85301164732276));
#47106=CARTESIAN_POINT('Ctrl Pts',(0.120005215320353,-0.108497912693302,
-0.845064356014807));
#47107=CARTESIAN_POINT('Ctrl Pts',(0.156192461868825,0.0421540462855391,
-0.837117064706857));
#47108=CARTESIAN_POINT('Ctrl Pts',(0.0491223143731926,0.154142943378894,
-0.829169773398904));
#47109=CARTESIAN_POINT('Ctrl Pts',(-0.103002086460407,0.124754234187424,
-0.821222482090954));
#47110=CARTESIAN_POINT('Ctrl Pts',(-0.160654511432484,-0.0190571959972504,
-0.813275190783002));
#47111=CARTESIAN_POINT('Ctrl Pts',(-0.0709570171198838,-0.145389650540663,
-0.805327899475051));
#47112=CARTESIAN_POINT('Ctrl Pts',(0.0838211938938518,-0.138372888302216,
-0.797380608167099));
#47113=CARTESIAN_POINT('Ctrl Pts',(0.161719857333879,-0.0044425788454637,
-0.789433316859147));
#47114=CARTESIAN_POINT('Ctrl Pts',(0.0912914821342712,0.133562397599832,
-0.781486025551195));
#47115=CARTESIAN_POINT('Ctrl Pts',(-0.0628680774803865,0.149065937077549,
-0.773538734243243));
#47116=CARTESIAN_POINT('Ctrl Pts',(-0.159365975061913,0.027848424649403,
-0.765591442935292));
#47117=CARTESIAN_POINT('Ctrl Pts',(-0.109695779679766,-0.118911247085109,
-0.757644151627341));
#47118=CARTESIAN_POINT('Ctrl Pts',(0.0405857470466367,-0.156607298359796,
-0.74969686031939));
#47119=CARTESIAN_POINT('Ctrl Pts',(0.15364263253448,-0.0506654737544443,
-0.741749569011437));
#47120=CARTESIAN_POINT('Ctrl Pts',(0.125780789374263,0.101745966933707,
-0.733802277703486));
#47121=CARTESIAN_POINT('Ctrl Pts',(-0.0174453158698736,0.160837525836132,
-0.725854986395534));
#47122=CARTESIAN_POINT('Ctrl Pts',(-0.144670837859916,0.0724113073752861,
-0.717907695087582));
#47123=CARTESIAN_POINT('Ctrl Pts',(-0.139206427326868,-0.0824294810961295,
-0.709960403779631));
#47124=CARTESIAN_POINT('Ctrl Pts',(-0.00606396002700117,-0.161667180193379,
-0.702013112471679));
#47125=CARTESIAN_POINT('Ctrl Pts',(0.1326402808736,-0.0926261553377884,
-0.694065821163729));
#47126=CARTESIAN_POINT('Ctrl Pts',(0.149688836500554,0.0613701962682061,
-0.686118529855775));
#47127=CARTESIAN_POINT('Ctrl Pts',(0.0294450261708669,0.159078720125241,
-0.678171238547825));
#47128=CARTESIAN_POINT('Ctrl Pts',(-0.117805322543121,0.110882616957749,
-0.670223947239873));
#47129=CARTESIAN_POINT('Ctrl Pts',(-0.157006388275539,-0.0390133669856671,
-0.662276655931922));
#47130=CARTESIAN_POINT('Ctrl Pts',(-0.0522035388156852,-0.153126873206524,
-0.65432936462397));
#47131=CARTESIAN_POINT('Ctrl Pts',(0.10047961703755,-0.12679469753454,-0.646382073316018));
#47132=CARTESIAN_POINT('Ctrl Pts',(0.161004368322975,0.0158316816481386,
-0.638434782008066));
#47133=CARTESIAN_POINT('Ctrl Pts',(0.0738583168071857,0.143937478793041,
-0.630487490700115));
#47134=CARTESIAN_POINT('Ctrl Pts',(-0.081029480165993,0.14002596940181,
-0.622540199392163));
#47135=CARTESIAN_POINT('Ctrl Pts',(-0.161598247715861,0.00768473148853606,
-0.614592908084211));
#47136=CARTESIAN_POINT('Ctrl Pts',(-0.0939515151520932,-0.131704827411578,
-0.60664561677626));
#47137=CARTESIAN_POINT('Ctrl Pts',(0.0598661443958943,-0.15029668498692,
-0.598698325468309));
#47138=CARTESIAN_POINT('Ctrl Pts',(0.158775470116437,-0.0310386670492156,
-0.590751034160357));
#47139=CARTESIAN_POINT('Ctrl Pts',(0.112058305192951,0.116687552893062,
-0.582803742852405));
#47140=CARTESIAN_POINT('Ctrl Pts',(-0.0374370642025506,0.1573896914883,
-0.574856451544454));
#47141=CARTESIAN_POINT('Ctrl Pts',(-0.152595717253679,0.0537363549073017,
-0.566909160236501));
#47142=CARTESIAN_POINT('Ctrl Pts',(-0.127795856721654,-0.0992031641010812,
-0.558961868928551));
#47143=CARTESIAN_POINT('Ctrl Pts',(0.0142164555799897,-0.161155022117307,
-0.551014577620598));
#47144=CARTESIAN_POINT('Ctrl Pts',(0.143189647077946,-0.0752978999214523,
-0.543067286312648));
#47145=CARTESIAN_POINT('Ctrl Pts',(0.140831432123592,0.0796213318709609,
-0.535119995004695));
#47146=CARTESIAN_POINT('Ctrl Pts',(0.00930473026448263,0.161513066832355,
-0.527172703696745));
#47147=CARTESIAN_POINT('Ctrl Pts',(-0.130756131271888,0.0952674283146994,
-0.519225412388792));
#47148=CARTESIAN_POINT('Ctrl Pts',(-0.150889421418604,-0.0583560730930949,
-0.51127812108084));
#47149=CARTESIAN_POINT('Ctrl Pts',(-0.0326291870467958,-0.158456255526732,
-0.50333082977289));
#47150=CARTESIAN_POINT('Ctrl Pts',(0.115558050524615,-0.113222726172084,
-0.495383538464937));
#47151=CARTESIAN_POINT('Ctrl Pts',(0.157757169457645,0.0358569971916244,
-0.487436247156986));
#47152=CARTESIAN_POINT('Ctrl Pts',(0.0552637679074694,0.152049218082689,
-0.479488955849034));
#47153=CARTESIAN_POINT('Ctrl Pts',(-0.0979167364692866,0.128784166270905,
-0.471541664541083));
#47154=CARTESIAN_POINT('Ctrl Pts',(-0.161289472071172,-0.0125998000734305,
-0.463594373233132));
#47155=CARTESIAN_POINT('Ctrl Pts',(-0.0767299119706533,-0.142427417907731,
-0.455647081925179));
#47156=CARTESIAN_POINT('Ctrl Pts',(0.0782051777977488,-0.141622734504423,
-0.447699790617228));
#47157=CARTESIAN_POINT('Ctrl Pts',(0.161411646107643,-0.0109237934669493,
-0.439752499309276));
#47158=CARTESIAN_POINT('Ctrl Pts',(0.0965737625129634,0.129794287844178,
-0.431805208001325));
#47159=CARTESIAN_POINT('Ctrl Pts',(-0.0568401341946973,0.151466986197049,
-0.423857916693373));
#47160=CARTESIAN_POINT('Ctrl Pts',(-0.158121108452566,0.0342164262397469,
-0.415910625385421));
#47161=CARTESIAN_POINT('Ctrl Pts',(-0.114375762814762,-0.114416929007158,
-0.40796333407747));
#47162=CARTESIAN_POINT('Ctrl Pts',(0.0342733248257124,-0.158108785234341,
-0.400016042769518));
#47163=CARTESIAN_POINT('Ctrl Pts',(0.151487430643043,-0.0567856242376266,
-0.392068751461566));
#47164=CARTESIAN_POINT('Ctrl Pts',(0.129759526809581,0.0966204634900976,
-0.384121460153615));
#47165=CARTESIAN_POINT('Ctrl Pts',(-0.0109818776801944,0.161407704665871,
-0.376174168845663));
#47166=CARTESIAN_POINT('Ctrl Pts',(-0.141650867923135,0.0781542089686166,
-0.368226877537712));
#47167=CARTESIAN_POINT('Ctrl Pts',(-0.142399796980305,-0.0767811603380389,
-0.36027958622976));
#47168=CARTESIAN_POINT('Ctrl Pts',(-0.0125417583021156,-0.161293995739392,
-0.352332294921809));
#47169=CARTESIAN_POINT('Ctrl Pts',(0.128819393840036,-0.0978703863973884,
-0.344385003613857));
#47170=CARTESIAN_POINT('Ctrl Pts',(0.152029321249178,0.0553184801255625,
-0.336437712305906));
#47171=CARTESIAN_POINT('Ctrl Pts',(0.0358002250341034,0.157770062592353,
-0.328490420997953));
#47172=CARTESIAN_POINT('Ctrl Pts',(-0.113264303078354,0.115517299185288,
-0.320543129690002));
#47173=CARTESIAN_POINT('Ctrl Pts',(-0.15844450346407,-0.0326862063401563,
-0.312595838382051));
#47174=CARTESIAN_POINT('Ctrl Pts',(-0.0583017708779276,-0.150910411421424,
-0.304648547074099));
#47175=CARTESIAN_POINT('Ctrl Pts',(0.0953144755013862,-0.130721840266996,
-0.296701255766148));
#47176=CARTESIAN_POINT('Ctrl Pts',(0.161509708013311,0.00936285107942815,
-0.288753964458196));
#47177=CARTESIAN_POINT('Ctrl Pts',(0.0795706477049501,0.140860075204769,
-0.280806673150245));
#47178=CARTESIAN_POINT('Ctrl Pts',(-0.0753494226742529,0.143162541419151,
-0.272859381842292));
#47179=CARTESIAN_POINT('Ctrl Pts',(-0.161160127556965,0.0141584620863805,
-0.264912090534341));
#47180=CARTESIAN_POINT('Ctrl Pts',(-0.0991571695951433,-0.127831547282851,
-0.256964799226389));
#47181=CARTESIAN_POINT('Ctrl Pts',(0.0537912638857975,-0.152576370034002,
-0.249017507918438));
#47182=CARTESIAN_POINT('Ctrl Pts',(0.157403153241977,-0.0373804241803696,
-0.241070216610486));
#47183=CARTESIAN_POINT('Ctrl Pts',(0.11664722050643,0.112100288629876,-0.233122925302535));
#47184=CARTESIAN_POINT('Ctrl Pts',(-0.03109580132088,0.15876429039619,-0.225175633994583));
#47185=CARTESIAN_POINT('Ctrl Pts',(-0.150318218428302,0.059812055372734,
-0.217228342686632));
#47186=CARTESIAN_POINT('Ctrl Pts',(-0.131671009899015,-0.0939989037990694,
-0.20928105137868));
#47187=CARTESIAN_POINT('Ctrl Pts',(0.00774288308919283,-0.161595471892866,
-0.201333760070728));
#47188=CARTESIAN_POINT('Ctrl Pts',(0.140055119212391,-0.0809790856917334,
-0.193386468762777));
#47189=CARTESIAN_POINT('Ctrl Pts',(0.143910891228999,0.0739101086366355,
-0.185439177454825));
#47190=CARTESIAN_POINT('Ctrl Pts',(0.0157737420722441,0.161010055264145,
-0.177491886146873));
#47191=CARTESIAN_POINT('Ctrl Pts',(-0.126830847136387,0.100433982260212,
-0.169544594838921));
#47192=CARTESIAN_POINT('Ctrl Pts',(-0.153108078234609,-0.0522586381566147,
-0.16159730353097));
#47193=CARTESIAN_POINT('Ctrl Pts',(-0.0389568634868797,-0.157020418959173,
-0.153650012223018));
#47194=CARTESIAN_POINT('Ctrl Pts',(0.110925000223214,-0.117765410005127,
-0.145702720915067));
#47195=CARTESIAN_POINT('Ctrl Pts',(0.159068118580144,0.0295022636793513,
-0.137755429607115));
#47196=CARTESIAN_POINT('Ctrl Pts',(0.0613163169383187,0.149710922597531,
-0.129808138299164));
#47197=CARTESIAN_POINT('Ctrl Pts',(-0.0926738637166896,0.132606918649559,
-0.121860846991212));
#47198=CARTESIAN_POINT('Ctrl Pts',(-0.161665019843371,-0.00612209556041882,
-0.11391355568326));
#47199=CARTESIAN_POINT('Ctrl Pts',(-0.0823793202671913,-0.13923615876769,
-0.105966264375309));
#47200=CARTESIAN_POINT('Ctrl Pts',(0.072463247076575,-0.144644623334344,
-0.098018973067357));
#47201=CARTESIAN_POINT('Ctrl Pts',(0.160844013877,-0.0173877164374548,-0.0900716817594055));
#47202=CARTESIAN_POINT('Ctrl Pts',(0.10170027857703,0.125817926598835,-0.0821243904514541));
#47203=CARTESIAN_POINT('Ctrl Pts',(-0.0507199647238506,0.153623381518765,
-0.0741770991435023));
#47204=CARTESIAN_POINT('Ctrl Pts',(-0.156623402096616,0.0405313031445145,
-0.0662298078355511));
#47205=CARTESIAN_POINT('Ctrl Pts',(-0.118868900789494,-0.109742197881292,
-0.0582825165275991));
#47206=CARTESIAN_POINT('Ctrl Pts',(0.027900335514407,-0.15934904467435,
-0.0503352252196477));
#47207=CARTESIAN_POINT('Ctrl Pts',(0.14909887050496,-0.0628275280611914,
-0.042387933911696));
#47208=CARTESIAN_POINT('Ctrl Pts',(0.133509936600416,0.0913644220801899,
-0.0344406426037444));
#47209=CARTESIAN_POINT('Ctrl Pts',(-0.0044634589477341,0.161670816842846,
-0.0264933512957926));
#47210=CARTESIAN_POINT('Ctrl Pts',(-0.138474820834309,0.0838631351225796,
-0.0185460599878411));
#47211=CARTESIAN_POINT('Ctrl Pts',(-0.145219806667121,-0.0711978527135158,
-0.0105987686798896));
#47212=CARTESIAN_POINT('Ctrl Pts',(-0.0613018075622001,-0.130529025318469,
-0.00530057447458853));
#47213=CARTESIAN_POINT('Ctrl Pts',(-0.0160685904325773,-0.135878184512857,
-0.00265147737193801));
#47214=CARTESIAN_POINT('Ctrl Pts',(0.128823493644022,-0.069446598083337,
-2.93765));
#47215=CARTESIAN_POINT('Ctrl Pts',(0.151941943903563,-0.0265618548091487,
-2.93500090289735));
#47216=CARTESIAN_POINT('Ctrl Pts',(0.151580971107978,0.0833657122950276,
-2.92970270869205));
#47217=CARTESIAN_POINT('Ctrl Pts',(0.0116953364202053,0.172764245811242,
-2.9217554173841));
#47218=CARTESIAN_POINT('Ctrl Pts',(-0.138782966866511,0.103272893425666,
-2.91380812607614));
#47219=CARTESIAN_POINT('Ctrl Pts',(-0.162037660106299,-0.0607202061494744,
-2.9058608347682));
#47220=CARTESIAN_POINT('Ctrl Pts',(-0.0366395801762509,-0.169135679591106,
-2.89791354346024));
#47221=CARTESIAN_POINT('Ctrl Pts',(0.12234579575611,-0.122362484441713,
-2.88996625215229));
#47222=CARTESIAN_POINT('Ctrl Pts',(0.169126899538293,0.0366081863273628,
-2.88201896084434));
#47223=CARTESIAN_POINT('Ctrl Pts',(0.0607823503659455,0.162019005104728,
-2.87407166953639));
#47224=CARTESIAN_POINT('Ctrl Pts',(-0.103308236397252,0.138819650059126,
-2.86612437822844));
#47225=CARTESIAN_POINT('Ctrl Pts',(-0.172647435005854,-0.0116983995188776,
-2.85817708692048));
#47226=CARTESIAN_POINT('Ctrl Pts',(-0.0836362547964333,-0.151489283614881,
-2.85022979561253));
#47227=CARTESIAN_POINT('Ctrl Pts',(0.0820844654854486,-0.15233517728973,
-2.84228250430458));
#47228=CARTESIAN_POINT('Ctrl Pts',(0.172518741936108,-0.0134621957780814,
-2.83433521299663));
#47229=CARTESIAN_POINT('Ctrl Pts',(0.104721297396897,0.137758466350652,
-2.82638792168868));
#47230=CARTESIAN_POINT('Ctrl Pts',(-0.0591249014323184,0.162628932530307,
-2.81844063038073));
#47231=CARTESIAN_POINT('Ctrl Pts',(-0.168742653009007,0.0383386685899805,
-2.81049333907278));
#47232=CARTESIAN_POINT('Ctrl Pts',(-0.123592147011918,-0.121115301787186,
-2.80254604776482));
#47233=CARTESIAN_POINT('Ctrl Pts',(0.0349152227561978,-0.169484098237391,
-2.79459875645688));
#47234=CARTESIAN_POINT('Ctrl Pts',(0.161398875831068,-0.0624046246492733,
-2.78665146514892));
#47235=CARTESIAN_POINT('Ctrl Pts',(0.139849887428109,0.101911446560615,
-2.77870417384097));
#47236=CARTESIAN_POINT('Ctrl Pts',(-0.00996732853818697,0.172755856534424,
-2.77075688253302));
#47237=CARTESIAN_POINT('Ctrl Pts',(-0.150642660216236,0.0851511762825492,
-2.76280959122507));
#47238=CARTESIAN_POINT('Ctrl Pts',(-0.153150792732914,-0.0805528926453607,
-2.75486229991711));
#47239=CARTESIAN_POINT('Ctrl Pts',(-0.0151913048999562,-0.172375050522329,
-2.74691500860916));
#47240=CARTESIAN_POINT('Ctrl Pts',(0.136701421070846,-0.106097385959945,
-2.73896771730121));
#47241=CARTESIAN_POINT('Ctrl Pts',(0.163213644563884,0.0574912171142146,
-2.73102042599326));
#47242=CARTESIAN_POINT('Ctrl Pts',(0.0400287500981403,0.168349734119888,
-2.72307313468531));
#47243=CARTESIAN_POINT('Ctrl Pts',(-0.119869916334605,0.124800388528227,
-2.71512584337735));
#47244=CARTESIAN_POINT('Ctrl Pts',(-0.169825685177861,-0.0332140101527191,
-2.70717855206941));
#47245=CARTESIAN_POINT('Ctrl Pts',(-0.064019871108235,-0.160765014600296,
-2.69923126076145));
#47246=CARTESIAN_POINT('Ctrl Pts',(0.100504012915477,-0.140864747914112,
-2.6912839694535));
#47247=CARTESIAN_POINT('Ctrl Pts',(0.172847116835337,0.00823456242596275,
-2.68333667814555));
#47248=CARTESIAN_POINT('Ctrl Pts',(0.0866574258333968,0.149781255050633,
-2.6753893868376));
#47249=CARTESIAN_POINT('Ctrl Pts',(-0.0790131623320317,0.153950816805319,
-2.66744209552965));
#47250=CARTESIAN_POINT('Ctrl Pts',(-0.172214057687311,0.0169189878994688,
-2.6594948042217));
#47251=CARTESIAN_POINT('Ctrl Pts',(-0.107462790519202,-0.135630684103927,
-2.65154751291375));
#47252=CARTESIAN_POINT('Ctrl Pts',(0.0558517436740735,-0.163781917638226,
-2.64360022160579));
#47253=CARTESIAN_POINT('Ctrl Pts',(0.1679398924462,-0.0417148216086108,
-2.63565293029784));
#47254=CARTESIAN_POINT('Ctrl Pts',(0.125996079239947,0.118612485990478,
-2.62770563898989));
#47255=CARTESIAN_POINT('Ctrl Pts',(-0.0315094567007179,0.170150192345199,
-2.61975834768194));
#47256=CARTESIAN_POINT('Ctrl Pts',(-0.160114989397424,0.0656286826543376,
-2.61181105637399));
#47257=CARTESIAN_POINT('Ctrl Pts',(-0.141865444364848,-0.0990864749188582,
-2.60386376506603));
#47258=CARTESIAN_POINT('Ctrl Pts',(0.00650096816217477,-0.172920997075647,
-2.59591647375808));
#47259=CARTESIAN_POINT('Ctrl Pts',(0.148904789751492,-0.088154962456717,
-2.58796918245013));
#47260=CARTESIAN_POINT('Ctrl Pts',(0.154735361356446,0.0774654875578245,
-2.58002189114218));
#47261=CARTESIAN_POINT('Ctrl Pts',(0.0186449697524707,0.172035748958206,
-2.57207459983422));
#47262=CARTESIAN_POINT('Ctrl Pts',(-0.134546309735667,0.108817389939271,
-2.56412730852628));
#47263=CARTESIAN_POINT('Ctrl Pts',(-0.164333722735227,-0.0542066544684583,
-2.55618001721832));
#47264=CARTESIAN_POINT('Ctrl Pts',(-0.0433966987745295,-0.167513164712969,
-2.54823272591038));
#47265=CARTESIAN_POINT('Ctrl Pts',(0.117343129381529,-0.127179101284886,
-2.54028543460242));
#47266=CARTESIAN_POINT('Ctrl Pts',(0.1704575912232,0.0298017350344859,-2.53233814329447));
#47267=CARTESIAN_POINT('Ctrl Pts',(0.0672308953579195,0.159448864925574,
-2.52439085198652));
#47268=CARTESIAN_POINT('Ctrl Pts',(-0.0976589739600992,0.142851876507598,
-2.51644356067857));
#47269=CARTESIAN_POINT('Ctrl Pts',(-0.172977490428231,-0.00476672023854133,
-2.50849626937062));
#47270=CARTESIAN_POINT('Ctrl Pts',(-0.0896436352611125,-0.148013352349895,
-2.50054897806266));
#47271=CARTESIAN_POINT('Ctrl Pts',(0.075910023771653,-0.155504347552306,
-2.49260168675471));
#47272=CARTESIAN_POINT('Ctrl Pts',(0.171840142351577,-0.0203690768880506,
-2.48465439544676));
#47273=CARTESIAN_POINT('Ctrl Pts',(0.110161047971342,0.133448406983887,
-2.47670710413881));
#47274=CARTESIAN_POINT('Ctrl Pts',(-0.0525561148836437,0.164869004379291,
-2.46875981283085));
#47275=CARTESIAN_POINT('Ctrl Pts',(-0.167069593839744,0.0450742124823536,
-2.46081252152291));
#47276=CARTESIAN_POINT('Ctrl Pts',(-0.128349335705578,-0.116061974137174,
-2.45286523021495));
#47277=CARTESIAN_POINT('Ctrl Pts',(0.028091016858721,-0.170747850904556,
-2.444917938907));
#47278=CARTESIAN_POINT('Ctrl Pts',(0.158766708164214,-0.0688263481188763,
-2.43697064759905));
#47279=CARTESIAN_POINT('Ctrl Pts',(0.143823945157437,0.0962216535714894,
-2.4290233562911));
#47280=CARTESIAN_POINT('Ctrl Pts',(-0.00303199302997265,0.173016591212946,
-2.42107606498315));
#47281=CARTESIAN_POINT('Ctrl Pts',(-0.147107032478502,0.0911232945631927,
-2.4131287736752));
#47282=CARTESIAN_POINT('Ctrl Pts',(-0.15625769807261,-0.0743469273724919,
-2.40518148236724));
#47283=CARTESIAN_POINT('Ctrl Pts',(-0.0220911359504884,-0.17162725753533,
-2.39723419105929));
#47284=CARTESIAN_POINT('Ctrl Pts',(0.132337086240727,-0.111493629513062,
-2.38928689975134));
#47285=CARTESIAN_POINT('Ctrl Pts',(0.165387708748813,0.0509002908783366,
-2.38133960844339));
#47286=CARTESIAN_POINT('Ctrl Pts',(0.0467471940611836,0.166609224426762,
-2.37339231713544));
#47287=CARTESIAN_POINT('Ctrl Pts',(-0.114769149075218,0.129506664837111,
-2.36544502582749));
#47288=CARTESIAN_POINT('Ctrl Pts',(-0.171020942204186,-0.0263774741829819,
-2.35749773451953));
#47289=CARTESIAN_POINT('Ctrl Pts',(-0.0704148805173739,-0.158068587702951,
-2.34955044321158));
#47290=CARTESIAN_POINT('Ctrl Pts',(0.0947746582729476,-0.144781552574654,
-2.34160315190363));
#47291=CARTESIAN_POINT('Ctrl Pts',(0.173038295498278,0.00129696096009361,
-2.33365586059568));
#47292=CARTESIAN_POINT('Ctrl Pts',(0.0925937915859414,0.146185921266108,
-2.32570856928773));
#47293=CARTESIAN_POINT('Ctrl Pts',(-0.0727763555268022,0.15699533716935,
-2.31776127797977));
#47294=CARTESIAN_POINT('Ctrl Pts',(-0.171397115914642,0.0238109737899195,
-2.30981398667183));
#47295=CARTESIAN_POINT('Ctrl Pts',(-0.112815000575814,-0.131212459247438,
-2.30186669536387));
#47296=CARTESIAN_POINT('Ctrl Pts',(0.0492393489425894,-0.165889783689024,
-2.29391940405592));
#47297=CARTESIAN_POINT('Ctrl Pts',(0.166132102763322,-0.048415475295804,
-2.28597211274797));
#47298=CARTESIAN_POINT('Ctrl Pts',(0.130650972312169,0.113464784186839,
-2.27802482144002));
#47299=CARTESIAN_POINT('Ctrl Pts',(-0.0246612793008269,0.171276837663264,
-2.27007753013207));
#47300=CARTESIAN_POINT('Ctrl Pts',(-0.157354573736509,0.0719963328294086,
-2.26213023882412));
#47301=CARTESIAN_POINT('Ctrl Pts',(-0.145724602473588,-0.0933181335571831,
-2.25418294751616));
#47302=CARTESIAN_POINT('Ctrl Pts',(-0.000438201516819747,-0.173042601101902,
-2.24623565620821));
#47303=CARTESIAN_POINT('Ctrl Pts',(0.145250111328747,-0.0940549784735931,
-2.23828836490026));
#47304=CARTESIAN_POINT('Ctrl Pts',(0.157717190674275,0.0711984661526903,
-2.23034107359231));
#47305=CARTESIAN_POINT('Ctrl Pts',(0.0255284174798185,0.171149740629828,
-2.22239378228436));
#47306=CARTESIAN_POINT('Ctrl Pts',(-0.130074639083192,0.114125028298172,
-2.2144464909764));
#47307=CARTESIAN_POINT('Ctrl Pts',(-0.166375178717216,-0.0475734560810524,
-2.20649919966846));
#47308=CARTESIAN_POINT('Ctrl Pts',(-0.0500788884436116,-0.165638276823124,
-2.1985519083605));
#47309=CARTESIAN_POINT('Ctrl Pts',(0.112149010623523,-0.131782143072748,
-2.19060461705255));
#47310=CARTESIAN_POINT('Ctrl Pts',(0.171515511551972,0.0229426047724884,
-2.1826573257446));
#47311=CARTESIAN_POINT('Ctrl Pts',(0.0735705460428639,0.156624738057678,
-2.17471003443665));
#47312=CARTESIAN_POINT('Ctrl Pts',(-0.0918522258750713,0.146653000032309,
-2.1667627431287));
#47313=CARTESIAN_POINT('Ctrl Pts',(-0.173029507590898,0.00217331993337852,
-2.15881545182074));
#47314=CARTESIAN_POINT('Ctrl Pts',(-0.0955067083065008,-0.144299696760383,
-2.15086816051279));
#47315=CARTESIAN_POINT('Ctrl Pts',(0.0696134179040222,-0.158423186006346,
-2.14292086920484));
#47316=CARTESIAN_POINT('Ctrl Pts',(0.170885156554018,-0.0272432943343881,
-2.13497357789689));
#47317=CARTESIAN_POINT('Ctrl Pts',(0.115423580959264,0.12892374015371,-2.12702628658893));
#47318=CARTESIAN_POINT('Ctrl Pts',(-0.0459027797961832,0.166843845027812,
-2.11907899528099));
#47319=CARTESIAN_POINT('Ctrl Pts',(-0.165127796259457,0.0517372662514804,
-2.11113170397303));
#47320=CARTESIAN_POINT('Ctrl Pts',(-0.132900063381712,-0.110821960683875,
-2.10318441266508));
#47321=CARTESIAN_POINT('Ctrl Pts',(0.0212216234075226,-0.171736939872093,
-2.09523712135713));
#47322=CARTESIAN_POINT('Ctrl Pts',(0.155879154050091,-0.0751373618735018,
-2.08728983004918));
#47323=CARTESIAN_POINT('Ctrl Pts',(0.147566651902153,0.0903770826209298,
-2.07934253874123));
#47324=CARTESIAN_POINT('Ctrl Pts',(0.00390821982662287,0.172999016281793,
-2.07139524743328));
#47325=CARTESIAN_POINT('Ctrl Pts',(-0.143334773123449,0.0969488351159036,
-2.06344795612533));
#47326=CARTESIAN_POINT('Ctrl Pts',(-0.159113252179034,-0.0680213701544789,
-2.05550066481737));
#47327=CARTESIAN_POINT('Ctrl Pts',(-0.0289554319259212,-0.170603390290653,
-2.04755337350942));
#47328=CARTESIAN_POINT('Ctrl Pts',(0.127759878179759,-0.116710527992013,
-2.03960608220147));
#47329=CARTESIAN_POINT('Ctrl Pts',(0.167295735497278,0.044227488071404,
-2.03165879089352));
#47330=CARTESIAN_POINT('Ctrl Pts',(0.0533904419725765,0.164600712400203,
-2.02371149958557));
#47331=CARTESIAN_POINT('Ctrl Pts',(-0.109483767800323,0.134004620834232,
-2.01576420827762));
#47332=CARTESIAN_POINT('Ctrl Pts',(-0.171941100359414,-0.0194985082474348,
-2.00781691696966));
#47333=CARTESIAN_POINT('Ctrl Pts',(-0.0766966227808798,-0.155117896680843,
-1.99986962566171));
#47334=CARTESIAN_POINT('Ctrl Pts',(0.0888928521176931,-0.148465466217109,
-1.99192233435376));
#47335=CARTESIAN_POINT('Ctrl Pts',(0.172951130240434,-0.00564272675556493,
-1.98397504304581));
#47336=CARTESIAN_POINT('Ctrl Pts',(0.0983812138986072,0.142355437439242,
-1.97602775173786));
#47337=CARTESIAN_POINT('Ctrl Pts',(-0.06642248298153,0.159787319807454,
-1.96808046042991));
#47338=CARTESIAN_POINT('Ctrl Pts',(-0.17030447017081,0.0306646581021379,
-1.96013316912195));
#47339=CARTESIAN_POINT('Ctrl Pts',(-0.117985739996266,-0.126583170185515,
-1.952185877814));
#47340=CARTESIAN_POINT('Ctrl Pts',(0.0425477493542096,-0.167730804688861,
-1.94423858650605));
#47341=CARTESIAN_POINT('Ctrl Pts',(0.164057078242671,-0.0550382493831285,
-1.9362912951981));
#47342=CARTESIAN_POINT('Ctrl Pts',(0.135095704369094,0.108134566525693,
-1.92834400389014));
#47343=CARTESIAN_POINT('Ctrl Pts',(-0.0177734325482762,0.172127972485977,
-1.9203967125822));
#47344=CARTESIAN_POINT('Ctrl Pts',(-0.154341042492961,0.0782481719841884,
-1.91244942127424));
#47345=CARTESIAN_POINT('Ctrl Pts',(-0.149349352603055,-0.0873996836020006,
-1.90450212996629));
#47346=CARTESIAN_POINT('Ctrl Pts',(-0.00737666631873438,-0.172885854281672,
-1.89655483865834));
#47347=CARTESIAN_POINT('Ctrl Pts',(0.141361788178154,-0.0998037006315704,
-1.88860754735039));
#47348=CARTESIAN_POINT('Ctrl Pts',(0.160445321115353,0.0648169171503288,
-1.88066025604244));
#47349=CARTESIAN_POINT('Ctrl Pts',(0.032370801003498,0.169988426250357,
-1.87271296473448));
#47350=CARTESIAN_POINT('Ctrl Pts',(-0.125393734486796,0.119249088751808,
-1.86476567342654));
#47351=CARTESIAN_POINT('Ctrl Pts',(-0.168149008857156,-0.0408637325392291,
-1.85681838211858));
#47352=CARTESIAN_POINT('Ctrl Pts',(-0.0566805227991419,-0.163496948448273,
-1.84887109081063));
#47353=CARTESIAN_POINT('Ctrl Pts',(0.106774492519686,-0.136173204279861,
-1.84092379950268));
#47354=CARTESIAN_POINT('Ctrl Pts',(0.172297537462134,0.0160465697632314,
-1.83297650819473));
#47355=CARTESIAN_POINT('Ctrl Pts',(0.0797918534780101,0.153548669597705,
-1.82502921688678));
#47356=CARTESIAN_POINT('Ctrl Pts',(-0.0858977272091994,0.150218222186841,
-1.81708192557883));
#47357=CARTESIAN_POINT('Ctrl Pts',(-0.172803194968885,0.0091098641716988,
-1.80913463427087));
#47358=CARTESIAN_POINT('Ctrl Pts',(-0.10121615228637,-0.14035392524979,
-1.80118734296292));
#47359=CARTESIAN_POINT('Ctrl Pts',(0.0632048340975654,-0.16108718994191,
-1.79324005165497));
#47360=CARTESIAN_POINT('Ctrl Pts',(0.169655290306931,-0.0340736890804721,
-1.78529276034702));
#47361=CARTESIAN_POINT('Ctrl Pts',(0.120500447231245,0.124191690679173,
-1.77734546903907));
#47362=CARTESIAN_POINT('Ctrl Pts',(-0.0391756069512533,0.168550305952503,
-1.76939817773112));
#47363=CARTESIAN_POINT('Ctrl Pts',(-0.162920379337028,0.0583170970930484,
-1.76145088642316));
#47364=CARTESIAN_POINT('Ctrl Pts',(-0.1372370122259,-0.105403682535241,
-1.75350359511521));
#47365=CARTESIAN_POINT('Ctrl Pts',(0.0143180935251707,-0.172449778238437,
-1.74555630380726));
#47366=CARTESIAN_POINT('Ctrl Pts',(0.152740857666704,-0.0813275120480199,
-1.73760901249931));
#47367=CARTESIAN_POINT('Ctrl Pts',(0.151071987605236,0.0843871339582318,
-1.72966172119136));
#47368=CARTESIAN_POINT('Ctrl Pts',(0.0108421460446119,0.172703160613315,
-1.72171442988341));
#47369=CARTESIAN_POINT('Ctrl Pts',(-0.139331949992912,0.102618426843595,
-1.71376713857545));
#47370=CARTESIAN_POINT('Ctrl Pts',(-0.161712861748395,-0.0615863959152187,
-1.7058198472675));
#47371=CARTESIAN_POINT('Ctrl Pts',(-0.035773151110808,-0.169305095836731,
-1.69787255595955));
#47372=CARTESIAN_POINT('Ctrl Pts',(0.122977159625931,-0.121739689612795,
-1.6899252646516));
#47373=CARTESIAN_POINT('Ctrl Pts',(0.16893465562522,0.0374835423281985,
-1.68197797334365));
#47374=CARTESIAN_POINT('Ctrl Pts',(0.0599478077103157,0.162327428881901,
-1.67403068203569));
#47375=CARTESIAN_POINT('Ctrl Pts',(-0.104022274404773,0.13828702124328,
-1.66608339072775));
#47376=CARTESIAN_POINT('Ctrl Pts',(-0.172584679507357,-0.0125881776291934,
-1.65813609941979));
#47377=CARTESIAN_POINT('Ctrl Pts',(-0.0828549932865788,-0.151917687923962,
-1.65018880811184));
#47378=CARTESIAN_POINT('Ctrl Pts',(0.082868055736469,-0.151910563013699,
-1.64224151680389));
#47379=CARTESIAN_POINT('Ctrl Pts',(0.172585761273234,-0.0125733377597181,
-1.63429422549594));
#47380=CARTESIAN_POINT('Ctrl Pts',(0.104010383307121,0.138295965165246,
-1.62634693418799));
#47381=CARTESIAN_POINT('Ctrl Pts',(-0.0599617653342634,0.162322273624663,
-1.61839964288004));
#47382=CARTESIAN_POINT('Ctrl Pts',(-0.168937878051169,0.0374690162167301,
-1.61045235157208));
#47383=CARTESIAN_POINT('Ctrl Pts',(-0.122966691292916,-0.121750263445934,
-1.60250506026413));
#47384=CARTESIAN_POINT('Ctrl Pts',(0.035787708804044,-0.169302019229655,
-1.59455776895618));
#47385=CARTESIAN_POINT('Ctrl Pts',(0.161718156702961,-0.0615724906860013,
-1.58661047764823));
#47386=CARTESIAN_POINT('Ctrl Pts',(0.139323125755536,0.102630407026321,
-1.57866318634028));
#47387=CARTESIAN_POINT('Ctrl Pts',(-0.0108569960151533,0.172702227704822,
-1.57071589503232));
#47388=CARTESIAN_POINT('Ctrl Pts',(-0.15107924313768,0.0843741436082613,
-1.56276860372438));
#47389=CARTESIAN_POINT('Ctrl Pts',(-0.152733864095016,-0.0813406452844256,
-1.55482131241642));
#47390=CARTESIAN_POINT('Ctrl Pts',(-0.0143032652488869,-0.172451008752924,
-1.54687402110847));
#47391=CARTESIAN_POINT('Ctrl Pts',(0.137246074933157,-0.105391881718297,
-1.53892672980052));
#47392=CARTESIAN_POINT('Ctrl Pts',(0.162915364295475,0.0583311057083122,
-1.53097943849257));
#47393=CARTESIAN_POINT('Ctrl Pts',(0.0391611138821227,0.168553673873318,
-1.52303214718461));
#47394=CARTESIAN_POINT('Ctrl Pts',(-0.12051112550133,0.124181328898849,
-1.51508485587667));
#47395=CARTESIAN_POINT('Ctrl Pts',(-0.169652359828074,-0.0340882768917243,
-1.50713756456871));
#47396=CARTESIAN_POINT('Ctrl Pts',(-0.0631909826612261,-0.161092624061407,
-1.49919027326076));
#47397=CARTESIAN_POINT('Ctrl Pts',(0.101228220349588,-0.140345221584266,
-1.49124298195281));
#47398=CARTESIAN_POINT('Ctrl Pts',(0.172802411011577,0.00912472275017703,
-1.48329569064486));
#47399=CARTESIAN_POINT('Ctrl Pts',(0.0858848102653002,0.150225607611934,
-1.4753483993369));
#47400=CARTESIAN_POINT('Ctrl Pts',(-0.0798050561804062,0.153541808067782,
-1.46740110802895));
#47401=CARTESIAN_POINT('Ctrl Pts',(-0.172298916601508,0.0160317545710972,
-1.459453816721));
#47402=CARTESIAN_POINT('Ctrl Pts',(-0.106762783169999,-0.136182384861176,
-1.45150652541305));
#47403=CARTESIAN_POINT('Ctrl Pts',(0.0566945809971845,-0.163492074126654,
-1.4435592341051));
#47404=CARTESIAN_POINT('Ctrl Pts',(0.168152521934197,-0.0408492739696887,
-1.43561194279715));
#47405=CARTESIAN_POINT('Ctrl Pts',(0.125383480301026,0.119259870385153,
-1.42766465148919));
#47406=CARTESIAN_POINT('Ctrl Pts',(-0.0323854174659853,0.169985642194378,
-1.41971736018125));
#47407=CARTESIAN_POINT('Ctrl Pts',(-0.160450893853394,0.0648031208996024,
-1.41177006887329));
#47408=CARTESIAN_POINT('Ctrl Pts',(-0.141353205959616,-0.0998158553618607,
-1.40382277756534));
#47409=CARTESIAN_POINT('Ctrl Pts',(0.00739153201114258,-0.172885219354373,
-1.39587548625739));
#47410=CARTESIAN_POINT('Ctrl Pts',(0.149356867178203,-0.0873868413629536,
-1.38792819494944));
#47411=CARTESIAN_POINT('Ctrl Pts',(0.154334313694721,0.0782614428250668,
-1.37998090364149));
#47412=CARTESIAN_POINT('Ctrl Pts',(0.0177586319299275,0.17212950011157,
-1.37203361233353));
#47413=CARTESIAN_POINT('Ctrl Pts',(-0.135105001901376,0.108122949820611,
-1.36408632102558));
#47414=CARTESIAN_POINT('Ctrl Pts',(-0.164052345131089,-0.0550523557504232,
-1.35613902971763));
#47415=CARTESIAN_POINT('Ctrl Pts',(-0.0425333267380425,-0.167734462568895,
-1.34819173840968));
#47416=CARTESIAN_POINT('Ctrl Pts',(0.117996623908803,-0.126573024625337,
-1.34024444710173));
#47417=CARTESIAN_POINT('Ctrl Pts',(0.170301832817638,0.0306793017462093,
-1.33229715579378));
#47418=CARTESIAN_POINT('Ctrl Pts',(0.0664087433035997,0.159793030603709,
-1.32434986448582));
#47419=CARTESIAN_POINT('Ctrl Pts',(-0.0983934540738328,0.142346977530617,
-1.31640257317788));
#47420=CARTESIAN_POINT('Ctrl Pts',(-0.172950644406985,-0.00565759806718521,
-1.30845528186992));
#47421=CARTESIAN_POINT('Ctrl Pts',(-0.0888800858747583,-0.148473109186738,
-1.30050799056197));
#47422=CARTESIAN_POINT('Ctrl Pts',(0.076709960425885,-0.15511130129085,
-1.29256069925402));
#47423=CARTESIAN_POINT('Ctrl Pts',(0.171942776317623,-0.019483723691048,
-1.28461340794607));
#47424=CARTESIAN_POINT('Ctrl Pts',(0.10947224490789,0.134014034382628,-1.27666611663812));
#47425=CARTESIAN_POINT('Ctrl Pts',(-0.0534045950907516,0.164596120974568,
-1.26871882533016));
#47426=CARTESIAN_POINT('Ctrl Pts',(-0.167299537812514,0.0442131028587772,
-1.26077153402221));
#47427=CARTESIAN_POINT('Ctrl Pts',(-0.12774984226529,-0.116721513089383,
-1.25282424271426));
#47428=CARTESIAN_POINT('Ctrl Pts',(0.0289701012791813,-0.170600899905467,
-1.24487695140631));
#47429=CARTESIAN_POINT('Ctrl Pts',(0.15911910045929,-0.0680076884308508,
-1.23692966009836));
#47430=CARTESIAN_POINT('Ctrl Pts',(0.143326436375369,0.0969611595053348,
-1.22898236879041));
#47431=CARTESIAN_POINT('Ctrl Pts',(-0.00392309526217261,0.172998679591046,
-1.22103507748245));
#47432=CARTESIAN_POINT('Ctrl Pts',(-0.147574422497777,0.0903643936577289,
-1.2130877861745));
#47433=CARTESIAN_POINT('Ctrl Pts',(-0.155872692731499,-0.0751507649815555,
-1.20514049486655));
#47434=CARTESIAN_POINT('Ctrl Pts',(-0.021206856399661,-0.171738763994403,
-1.1971932035586));
#47435=CARTESIAN_POINT('Ctrl Pts',(0.132909591999709,-0.110810532762696,
-1.18924591225065));
#47436=CARTESIAN_POINT('Ctrl Pts',(0.165123346981426,0.0517514646974669,
-1.1812986209427));
#47437=CARTESIAN_POINT('Ctrl Pts',(0.0458884334335047,0.166847791395931,
-1.17335132963475));
#47438=CARTESIAN_POINT('Ctrl Pts',(-0.115434666136934,0.128913814894044,
-1.16540403832679));
#47439=CARTESIAN_POINT('Ctrl Pts',(-0.170882813387225,-0.0272579879218593,
-1.15745674701884));
#47440=CARTESIAN_POINT('Ctrl Pts',(-0.0695997955103653,-0.158429171182573,
-1.14950945571089));
#47441=CARTESIAN_POINT('Ctrl Pts',(0.0955191156709451,-0.144291484011088,
-1.14156216440294));
#47442=CARTESIAN_POINT('Ctrl Pts',(0.173029320076704,0.00218819799715939,
-1.13361487309499));
#47443=CARTESIAN_POINT('Ctrl Pts',(0.0918396154674594,0.146660897472607,
-1.12566758178703));
#47444=CARTESIAN_POINT('Ctrl Pts',(-0.0735840132663084,0.156618411460164,
-1.11772029047909));
#47445=CARTESIAN_POINT('Ctrl Pts',(-0.171517483654975,0.0229278567979429,
-1.10977299917113));
#47446=CARTESIAN_POINT('Ctrl Pts',(-0.112137678822651,-0.131791785802262,
-1.10182570786318));
#47447=CARTESIAN_POINT('Ctrl Pts',(0.0500931307897824,-0.165633970140062,
-1.09387841655523));
#47448=CARTESIAN_POINT('Ctrl Pts',(0.166379268741419,-0.0475591500108228,
-1.08593112524728));
#47449=CARTESIAN_POINT('Ctrl Pts',(0.130064825476295,0.114136212441549,
-1.07798383393933));
#47450=CARTESIAN_POINT('Ctrl Pts',(-0.0255431338240911,0.171147544917028,
-1.07003654263137));
#47451=CARTESIAN_POINT('Ctrl Pts',(-0.157723312144672,0.0711849044587089,
-1.06208925132342));
#47452=CARTESIAN_POINT('Ctrl Pts',(-0.145242023404015,-0.0940674675655127,
-1.05414196001547));
#47453=CARTESIAN_POINT('Ctrl Pts',(0.000453080712868733,-0.173042562783117,
-1.04619466870752));
#47454=CARTESIAN_POINT('Ctrl Pts',(0.145732625964489,-0.0933056029731116,
-1.03824737739957));
#47455=CARTESIAN_POINT('Ctrl Pts',(0.157348382496199,0.0720098628141407,
-1.03030008609162));
#47456=CARTESIAN_POINT('Ctrl Pts',(0.024646551842481,0.171278957548664,
-1.02235279478366));
#47457=CARTESIAN_POINT('Ctrl Pts',(-0.130660728183639,0.11345354964567,
-1.01440550347571));
#47458=CARTESIAN_POINT('Ctrl Pts',(-0.166127939108261,-0.0484297601101159,
-1.00645821216776));
#47459=CARTESIAN_POINT('Ctrl Pts',(-0.0492250846032552,-0.165894016958069,
-0.998510920859811));
#47460=CARTESIAN_POINT('Ctrl Pts',(0.112826282560356,-0.131202758280047,
-0.990563629551857));
#47461=CARTESIAN_POINT('Ctrl Pts',(0.171395067876608,0.0238257114112947,
-0.982616338243905));
#47462=CARTESIAN_POINT('Ctrl Pts',(0.0727628558960999,0.157001594318417,
-0.974669046935956));
#47463=CARTESIAN_POINT('Ctrl Pts',(-0.0926063611495833,0.146177958979164,
-0.966721755628002));
#47464=CARTESIAN_POINT('Ctrl Pts',(-0.173038406378754,0.00128208212784741,
-0.958774464320052));
#47465=CARTESIAN_POINT('Ctrl Pts',(-0.0947622087723417,-0.144789701309411,
-0.9508271730121));
#47466=CARTESIAN_POINT('Ctrl Pts',(0.0704284719029783,-0.158062532442362,
-0.942879881704148));
#47467=CARTESIAN_POINT('Ctrl Pts',(0.171023209658835,-0.0263627687216561,
-0.934932590396196));
#47468=CARTESIAN_POINT('Ctrl Pts',(0.114758012923362,0.129516532869604,
-0.926985299088245));
#47469=CARTESIAN_POINT('Ctrl Pts',(-0.0467615199073322,0.16660520421835,
-0.919038007780294));
#47470=CARTESIAN_POINT('Ctrl Pts',(-0.16539208483705,0.050886069704146,
-0.911090716472341));
#47471=CARTESIAN_POINT('Ctrl Pts',(-0.132327498888257,-0.111505008204384,
-0.90314342516439));
#47472=CARTESIAN_POINT('Ctrl Pts',(0.0221058933671197,-0.17162535737799,
-0.895196133856439));
#47473=CARTESIAN_POINT('Ctrl Pts',(0.156264090271199,-0.0743334911624345,
-0.887248842548486));
#47474=CARTESIAN_POINT('Ctrl Pts',(0.147099196629942,0.0911359433347066,
-0.879301551240536));
#47475=CARTESIAN_POINT('Ctrl Pts',(0.00301711605757047,0.173016851281536,
-0.871354259932582));
#47476=CARTESIAN_POINT('Ctrl Pts',(-0.143832218316713,0.096209286406122,
-0.863406968624633));
#47477=CARTESIAN_POINT('Ctrl Pts',(-0.158760789492189,-0.0688399995387715,
-0.85545967731668));
#47478=CARTESIAN_POINT('Ctrl Pts',(-0.0280763348730118,-0.170750265700466,
-0.84751238600873));
#47479=CARTESIAN_POINT('Ctrl Pts',(0.128359314906885,-0.116050937494345,
-0.839565094700776));
#47480=CARTESIAN_POINT('Ctrl Pts',(0.167065717482201,0.0450885779198969,
-0.831617803392827));
#47481=CARTESIAN_POINT('Ctrl Pts',(0.0525419383045171,0.164873522846713,
-0.823670512084872));
#47482=CARTESIAN_POINT('Ctrl Pts',(-0.110172522225335,0.133438934210332,
-0.815723220776924));
#47483=CARTESIAN_POINT('Ctrl Pts',(-0.171838390265988,-0.0203838526161073,
-0.80777592946897));
#47484=CARTESIAN_POINT('Ctrl Pts',(-0.0758966523332277,-0.155510874157695,
-0.79982863816102));
#47485=CARTESIAN_POINT('Ctrl Pts',(0.0896563619686924,-0.148005643727598,
-0.791881346853067));
#47486=CARTESIAN_POINT('Ctrl Pts',(0.172977899658784,-0.00475184662183322,
-0.783934055545116));
#47487=CARTESIAN_POINT('Ctrl Pts',(0.0976466903734667,0.142860273259537,
-0.775986764237163));
#47488=CARTESIAN_POINT('Ctrl Pts',(-0.0672446054394721,0.159443083437229,
-0.768039472929214));
#47489=CARTESIAN_POINT('Ctrl Pts',(-0.170460153117567,0.0297870780006496,
-0.76009218162126));
#47490=CARTESIAN_POINT('Ctrl Pts',(-0.117332193357448,-0.12718919065161,
-0.75214489031331));
#47491=CARTESIAN_POINT('Ctrl Pts',(0.0434111023590466,-0.167509432596059,
-0.744197599005357));
#47492=CARTESIAN_POINT('Ctrl Pts',(0.16433838312751,-0.0541925239098243,
-0.736250307697407));
#47493=CARTESIAN_POINT('Ctrl Pts',(0.134536952493496,0.108828958602222,
-0.728303016389454));
#47494=CARTESIAN_POINT('Ctrl Pts',(-0.0186597623062839,0.172034145120539,
-0.720355725081503));
#47495=CARTESIAN_POINT('Ctrl Pts',(-0.154742021712401,0.0774521822354978,
-0.712408433773552));
#47496=CARTESIAN_POINT('Ctrl Pts',(-0.148897209130542,-0.0881677658207174,
-0.704461142465599));
#47497=CARTESIAN_POINT('Ctrl Pts',(-0.00648609939667713,-0.172921555427013,
-0.696513851157649));
#47498=CARTESIAN_POINT('Ctrl Pts',(0.141873963865172,-0.0990742761460573,
-0.688566559849696));
#47499=CARTESIAN_POINT('Ctrl Pts',(0.160109345674077,0.0656424500190254,
-0.680619268541746));
#47500=CARTESIAN_POINT('Ctrl Pts',(0.0314948260924915,0.170152901080425,
-0.672671977233793));
#47501=CARTESIAN_POINT('Ctrl Pts',(-0.126006277757622,0.118601651684748,
-0.664724685925842));
#47502=CARTESIAN_POINT('Ctrl Pts',(-0.167936304945184,-0.0417292618918592,
-0.65677739461789));
#47503=CARTESIAN_POINT('Ctrl Pts',(-0.0558376605567283,-0.163786719486755,
-0.648830103309939));
#47504=CARTESIAN_POINT('Ctrl Pts',(0.107474452427893,-0.135621443334034,
-0.640882812001987));
#47505=CARTESIAN_POINT('Ctrl Pts',(0.172212602258851,0.0169337957917512,
-0.632935520694036));
#47506=CARTESIAN_POINT('Ctrl Pts',(0.0789999244635886,0.153957610242003,
-0.624988229386083));
#47507=CARTESIAN_POINT('Ctrl Pts',(-0.0866703045663745,0.149773803193526,
-0.617040938078132));
#47508=CARTESIAN_POINT('Ctrl Pts',(-0.172847824251535,0.00821970000618283,
-0.609093646770181));
#47509=CARTESIAN_POINT('Ctrl Pts',(-0.100491900182772,-0.140873389305209,
-0.601146355462228));
#47510=CARTESIAN_POINT('Ctrl Pts',(0.0640336943712063,-0.160759509211294,
-0.593199064154279));
#47511=CARTESIAN_POINT('Ctrl Pts',(0.169828540482666,-0.0331994074376132,
-0.585251772846325));
#47512=CARTESIAN_POINT('Ctrl Pts',(0.119859184834551,0.12481069516463,-0.577304481538374));
#47513=CARTESIAN_POINT('Ctrl Pts',(-0.0400432256242976,0.16834629160835,
-0.569357190230424));
#47514=CARTESIAN_POINT('Ctrl Pts',(-0.163218587393212,0.0574771828297637,
-0.56140989892247));
#47515=CARTESIAN_POINT('Ctrl Pts',(-0.136692297688386,-0.106109139895445,
-0.55346260761452));
#47516=CARTESIAN_POINT('Ctrl Pts',(0.0152061266152587,-0.172373743737386,
-0.545515316306566));
#47517=CARTESIAN_POINT('Ctrl Pts',(0.153157718617635,-0.0805397233948725,
-0.537568024998617));
#47518=CARTESIAN_POINT('Ctrl Pts',(0.150635337776628,0.0851641287726385,
-0.529620733690664));
#47519=CARTESIAN_POINT('Ctrl Pts',(0.00995247414000182,0.172756713545882,
-0.521673442382713));
#47520=CARTESIAN_POINT('Ctrl Pts',(-0.139858650185577,0.101899419944128,
-0.513726151074762));
#47521=CARTESIAN_POINT('Ctrl Pts',(-0.161393508676135,-0.0624185002534306,
-0.505778859766809));
#47522=CARTESIAN_POINT('Ctrl Pts',(-0.034900650643503,-0.16948710393815,
-0.497831568458858));
#47523=CARTESIAN_POINT('Ctrl Pts',(0.123602563086265,-0.121104666364214,
-0.489884277150907));
#47524=CARTESIAN_POINT('Ctrl Pts',(0.168739351362149,0.0383531630841987,
-0.481936985842954));
#47525=CARTESIAN_POINT('Ctrl Pts',(0.0591109258779971,0.16263404397151,
-0.473989694535003));
#47526=CARTESIAN_POINT('Ctrl Pts',(-0.104733158284532,0.13774940788413,
-0.466042403227052));
#47527=CARTESIAN_POINT('Ctrl Pts',(-0.17251755335367,-0.0134769284907569,
-0.4580951119191));
#47528=CARTESIAN_POINT('Ctrl Pts',(-0.0820714242054011,-0.152342427266925,
-0.450147820611148));
#47529=CARTESIAN_POINT('Ctrl Pts',(0.083649389882709,-0.151481726254132,
-0.442200529303197));
#47530=CARTESIAN_POINT('Ctrl Pts',(0.172648232471067,-0.0116842475708879,
-0.434253237995245));
#47531=CARTESIAN_POINT('Ctrl Pts',(0.103296693906605,0.138829848536424,
-0.426305946687294));
#47532=CARTESIAN_POINT('Ctrl Pts',(-0.0607970300704926,0.162011280321123,
-0.418358655379342));
#47533=CARTESIAN_POINT('Ctrl Pts',(-0.169128625777697,0.0365983846532847,
-0.410411364071391));
#47534=CARTESIAN_POINT('Ctrl Pts',(-0.122337971042862,-0.122382002997978,
-0.402464072763438));
#47535=CARTESIAN_POINT('Ctrl Pts',(0.0366592442042335,-0.169115444685149,
-0.394516781455488));
#47536=CARTESIAN_POINT('Ctrl Pts',(0.162033147996417,-0.0607387254315766,
-0.386569490147535));
#47537=CARTESIAN_POINT('Ctrl Pts',(0.138792667630779,0.103346645947574,
-0.378622198839585));
#47538=CARTESIAN_POINT('Ctrl Pts',(-0.0117463752859325,0.172644016647908,
-0.370674907531632));
#47539=CARTESIAN_POINT('Ctrl Pts',(-0.151511818165916,0.0835948728854811,
-0.362727616223682));
#47540=CARTESIAN_POINT('Ctrl Pts',(-0.152312883523237,-0.0821262402007903,
-0.354780324915729));
#47541=CARTESIAN_POINT('Ctrl Pts',(-0.0134148461722152,-0.172522391934662,
-0.346833033607778));
#47542=CARTESIAN_POINT('Ctrl Pts',(0.137787087801864,-0.104683581576881,
-0.338885742299826));
#47543=CARTESIAN_POINT('Ctrl Pts',(0.162612762030453,0.0591694468582298,
-0.330938450991874));
#47544=CARTESIAN_POINT('Ctrl Pts',(0.0382924387629439,0.168753142045614,
-0.322991159683923));
#47545=CARTESIAN_POINT('Ctrl Pts',(-0.121149137624835,0.123558974863995,
-0.315043868375971));
#47546=CARTESIAN_POINT('Ctrl Pts',(-0.169474533761859,-0.0349616393048283,
-0.30709657706802));
#47547=CARTESIAN_POINT('Ctrl Pts',(-0.0623604178182606,-0.161415959886906,
-0.299149285760068));
#47548=CARTESIAN_POINT('Ctrl Pts',(0.101949742295844,-0.139821972030507,
-0.291201994452117));
#47549=CARTESIAN_POINT('Ctrl Pts',(0.172753120904425,0.0100146410047549,
-0.283254703144165));
#47550=CARTESIAN_POINT('Ctrl Pts',(0.0851099162552044,0.150665974830759,
-0.275307411836213));
#47551=CARTESIAN_POINT('Ctrl Pts',(-0.0805948328768723,0.153128726012732,
-0.267360120528262));
#47552=CARTESIAN_POINT('Ctrl Pts',(-0.172379204589526,0.0151440959352495,
-0.25941282922031));
#47553=CARTESIAN_POINT('Ctrl Pts',(-0.106059943506291,-0.136730472829133,
-0.251465537912358));
#47554=CARTESIAN_POINT('Ctrl Pts',(0.0575359142677703,-0.163197893327065,
-0.243518246604407));
#47555=CARTESIAN_POINT('Ctrl Pts',(0.168360690494893,-0.0399826426369145,
-0.235570955296455));
#47556=CARTESIAN_POINT('Ctrl Pts',(0.124767555060224,0.119904090926243,
-0.227623663988504));
#47557=CARTESIAN_POINT('Ctrl Pts',(-0.0332605190813962,0.169816582492104,
-0.219676372680552));
#47558=CARTESIAN_POINT('Ctrl Pts',(-0.160782541691814,0.0639758399692923,
-0.2117290813726));
#47559=CARTESIAN_POINT('Ctrl Pts',(-0.140837217604386,-0.100542587765356,
-0.203781790064649));
#47560=CARTESIAN_POINT('Ctrl Pts',(0.00828189979977818,-0.172844855191089,
-0.195834498756697));
#47561=CARTESIAN_POINT('Ctrl Pts',(0.149804982252761,-0.0866164019074298,
-0.187887207448745));
#47562=CARTESIAN_POINT('Ctrl Pts',(0.153929171798746,0.0790553217538663,
-0.179939916140794));
#47563=CARTESIAN_POINT('Ctrl Pts',(0.0168718227829098,0.172218685093424,
-0.171992624832842));
#47564=CARTESIAN_POINT('Ctrl Pts',(-0.135660109471302,0.107425640809655,
-0.164045333524891));
#47565=CARTESIAN_POINT('Ctrl Pts',(-0.163766616112805,-0.0558965956091489,
-0.156098042216939));
#47566=CARTESIAN_POINT('Ctrl Pts',(-0.0416688249318735,-0.167951312367441,
-0.148150750908988));
#47567=CARTESIAN_POINT('Ctrl Pts',(0.118646985438833,-0.125963586729395,
-0.140203459601036));
#47568=CARTESIAN_POINT('Ctrl Pts',(0.170141561514371,0.031556048159871,
-0.132256168293084));
#47569=CARTESIAN_POINT('Ctrl Pts',(0.0655848199080706,0.160132969283019,
-0.124308876985133));
#47570=CARTESIAN_POINT('Ctrl Pts',(-0.099125305718535,0.141838279147541,
-0.116361585677181));
#47571=CARTESIAN_POINT('Ctrl Pts',(-0.172919244685382,-0.0065482820045211,
-0.108414294369229));
#47572=CARTESIAN_POINT('Ctrl Pts',(-0.0881141130721895,-0.1489290103099,
-0.100467003061277));
#47573=CARTESIAN_POINT('Ctrl Pts',(0.0775077376916343,-0.15471398227649,
-0.0925197117533261));
#47574=CARTESIAN_POINT('Ctrl Pts',(0.172041084822943,-0.0185981531198262,
-0.0845724204453744));
#47575=CARTESIAN_POINT('Ctrl Pts',(0.108780089674747,0.134576675006324,
-0.076625129137423));
#47576=CARTESIAN_POINT('Ctrl Pts',(-0.0542508082392599,0.164317791962513,
-0.0686778378294712));
#47577=CARTESIAN_POINT('Ctrl Pts',(-0.167526657386005,0.0433528683734585,
-0.06073054652152));
#47578=CARTESIAN_POINT('Ctrl Pts',(-0.127143896441013,-0.117381842937533,
-0.0527832552135681));
#47579=CARTESIAN_POINT('Ctrl Pts',(0.0298426026130803,-0.170442044130026,
-0.0448359639056166));
#47580=CARTESIAN_POINT('Ctrl Pts',(0.159478309507775,-0.0672012331938912,
-0.0368886725976649));
#47581=CARTESIAN_POINT('Ctrl Pts',(0.142804160215386,0.0977247079951531,
-0.0289413812897132));
#47582=CARTESIAN_POINT('Ctrl Pts',(-0.00477418028139723,0.172925445239909,
-0.0209940899817616));
#47583=CARTESIAN_POINT('Ctrl Pts',(-0.148114672239004,0.0897012229138564,
-0.01304679867381));
#47584=CARTESIAN_POINT('Ctrl Pts',(-0.155329206692728,-0.0761542535693343,
-0.00509950736585855));
#47585=CARTESIAN_POINT('Ctrl Pts',(-0.0655693004694094,-0.139615734371339,
0.000198686839442543));
#47586=CARTESIAN_POINT('Ctrl Pts',(-0.0171871968558861,-0.145337272453549,
0.00284778394209306));
#47587=CARTESIAN_POINT('Ctrl Pts',(-0.146319403921505,0.000134192518820611,
-0.0587155045842896));
#47588=CARTESIAN_POINT('Ctrl Pts',(-0.145990313106502,-0.0362412802340569,
-0.0567380881273823));
#47589=CARTESIAN_POINT('Ctrl Pts',(-0.132264295006575,-0.0728382504267649,
-0.0547606716704749));
#47590=CARTESIAN_POINT('Ctrl Pts',(-0.107709940089491,-0.0994360912511227,
-0.0527832552135677));
#47591=CARTESIAN_POINT('Ctrl Pts',(-0.0748150634229754,-0.135068576668367,
-0.0501341581109172));
#47592=CARTESIAN_POINT('Ctrl Pts',(-0.0224862304049495,-0.152755310399195,
-0.047485061008267));
#47593=CARTESIAN_POINT('Ctrl Pts',(0.0252841372531801,-0.144391875441922,
-0.0448359639056166));
#47594=CARTESIAN_POINT('Ctrl Pts',(0.0730545049113125,-0.136028440484648,
-0.042186866802966));
#47595=CARTESIAN_POINT('Ctrl Pts',(0.116266407209548,-0.101614836839265,
-0.0395377697003152));
#47596=CARTESIAN_POINT('Ctrl Pts',(0.135093333476596,-0.0569203781517345,
-0.0368886725976646));
#47597=CARTESIAN_POINT('Ctrl Pts',(0.153920259743645,-0.0122259194642038,
-0.0342395754950141));
#47598=CARTESIAN_POINT('Ctrl Pts',(0.148362209979515,0.0427493942654739,
-0.0315904783923637));
#47599=CARTESIAN_POINT('Ctrl Pts',(0.120986795014652,0.0827705073377738,
-0.0289413812897131));
#47600=CARTESIAN_POINT('Ctrl Pts',(0.093611380049789,0.122791620410074,
-0.0262922841870625));
#47601=CARTESIAN_POINT('Ctrl Pts',(0.0444185998841973,0.147858532824991,
-0.0236431870844121));
#47602=CARTESIAN_POINT('Ctrl Pts',(-0.00406787219153488,0.146521285311441,
-0.0209940899817616));
#47603=CARTESIAN_POINT('Ctrl Pts',(-0.0488742093476865,0.145285535206551,
-0.0185460599878418));
#47604=CARTESIAN_POINT('Ctrl Pts',(-0.0930773873900169,0.12150167906643,
-0.0160980299939217));
#47605=CARTESIAN_POINT('Ctrl Pts',(-0.119330942213657,0.085138415363241,
-0.013650000000002));
#47606=CARTESIAN_POINT('',(-0.000893209148009567,0.117964196654764,-2.93765));
#47607=CARTESIAN_POINT('Ctrl Pts',(-0.0008932091480129,0.117964196654764,
-2.93765));
#47608=CARTESIAN_POINT('Ctrl Pts',(0.00208421411728759,0.118354195981894,
-2.93765));
#47609=CARTESIAN_POINT('Ctrl Pts',(0.00507143193442542,0.118622138849448,
-2.93765));
#47610=CARTESIAN_POINT('Ctrl Pts',(0.00806195760498323,0.118765052615256,
-2.93765));
#47611=CARTESIAN_POINT('Ctrl Pts',(0.0152384124430961,0.119108007098531,
-2.93765));
#47612=CARTESIAN_POINT('Ctrl Pts',(0.0224335537438771,0.118732751163502,
-2.93765));
#47613=CARTESIAN_POINT('Ctrl Pts',(0.0295711880776548,0.117700942165764,
-2.93765));
#47614=CARTESIAN_POINT('Ctrl Pts',(0.0334765121796589,0.117136392574247,
-2.93765));
#47615=CARTESIAN_POINT('Ctrl Pts',(0.0373569563325073,0.116375728419311,
-2.93765));
#47616=CARTESIAN_POINT('Ctrl Pts',(0.0411928145026145,0.115431075471498,
-2.93765));
#47617=CARTESIAN_POINT('Ctrl Pts',(0.0481018456958536,0.113729595282767,
-2.93765));
#47618=CARTESIAN_POINT('Ctrl Pts',(0.0548737925559738,0.111431279199373,
-2.93765));
#47619=CARTESIAN_POINT('Ctrl Pts',(0.0614384215502389,0.10858518186639,
-2.93765));
#47620=CARTESIAN_POINT('Ctrl Pts',(0.0646734046575246,0.107182653741505,
-2.93765));
#47621=CARTESIAN_POINT('Ctrl Pts',(0.0678508377690415,0.105649735926586,
-2.93765));
#47622=CARTESIAN_POINT('Ctrl Pts',(0.0709571867534955,0.103995938706946,
-2.93765));
#47623=CARTESIAN_POINT('Ctrl Pts',(0.0793412397536873,0.099532330911938,
-2.93765));
#47624=CARTESIAN_POINT('Ctrl Pts',(0.0872211356366982,0.0941863465303336,
-2.93765));
#47625=CARTESIAN_POINT('Ctrl Pts',(0.0944378463806949,0.0880609267163502,
-2.93765));
#47626=CARTESIAN_POINT('Ctrl Pts',(0.0970752818418381,0.0858223169112907,
-2.93765));
#47627=CARTESIAN_POINT('Ctrl Pts',(0.0996240141760927,0.0834791156530963,
-2.93765));
#47628=CARTESIAN_POINT('Ctrl Pts',(0.102075530811344,0.0810347775427261,
-2.93765));
#47629=CARTESIAN_POINT('Ctrl Pts',(0.104250398830597,0.0788662779665695,
-2.93765));
#47630=CARTESIAN_POINT('Ctrl Pts',(0.106344685942108,0.0766219445137936,
-2.93765));
#47631=CARTESIAN_POINT('Ctrl Pts',(0.108348175066807,0.0743108418799378,
-2.93765));
#47632=CARTESIAN_POINT('Ctrl Pts',(0.111175899843332,0.0710489513618998,
-2.93765));
#47633=CARTESIAN_POINT('Ctrl Pts',(0.113826045040914,0.0676509280277566,
-2.93765));
#47634=CARTESIAN_POINT('Ctrl Pts',(0.116284186664136,0.0641259479802579,
-2.93765));
#47635=CARTESIAN_POINT('Ctrl Pts',(0.120002164263989,0.0587943606002954,
-2.93765));
#47636=CARTESIAN_POINT('Ctrl Pts',(0.123281449454453,0.0531727090630523,
-2.93765));
#47637=CARTESIAN_POINT('Ctrl Pts',(0.126128015808201,0.047316382515659,
-2.93765));
#47638=CARTESIAN_POINT('Ctrl Pts',(0.127562547730943,0.0443650768588713,
-2.93765));
#47639=CARTESIAN_POINT('Ctrl Pts',(0.128887043644863,0.0413540347815275,
-2.93765));
#47640=CARTESIAN_POINT('Ctrl Pts',(0.130101371942864,0.0382896759029232,
-2.93765));
#47641=CARTESIAN_POINT('Ctrl Pts',(0.131334954033748,0.0351767300554848,
-2.93765));
#47642=CARTESIAN_POINT('Ctrl Pts',(0.132451910687336,0.0320157007800445,
-2.93765));
#47643=CARTESIAN_POINT('Ctrl Pts',(0.133451273547085,0.0288208664690228,
-2.93765));
#47644=CARTESIAN_POINT('Ctrl Pts',(0.13594044569831,0.0208633037907661,
-2.93765));
#47645=CARTESIAN_POINT('Ctrl Pts',(0.137706627804123,0.0126846288520797,
-2.93765));
#47646=CARTESIAN_POINT('Ctrl Pts',(0.138759382734113,0.00439393427432196,
-2.93765));
#47647=CARTESIAN_POINT('Ctrl Pts',(0.139457649115666,-0.00110507897032189,
-2.93765));
#47648=CARTESIAN_POINT('Ctrl Pts',(0.139841620680567,-0.00665378048569686,
-2.93765));
#47649=CARTESIAN_POINT('Ctrl Pts',(0.13990842161102,-0.0122228021535617,
-2.93765));
#47650=CARTESIAN_POINT('Ctrl Pts',(0.139946458473856,-0.0153938375250784,
-2.93765));
#47651=CARTESIAN_POINT('Ctrl Pts',(0.139881269861857,-0.0185709804508514,
-2.93765));
#47652=CARTESIAN_POINT('Ctrl Pts',(0.139713346423489,-0.0217351033015259,
-2.93765));
#47653=CARTESIAN_POINT('Ctrl Pts',(0.139165794893991,-0.0320524260245424,
-2.93765));
#47654=CARTESIAN_POINT('Ctrl Pts',(0.137530845631308,-0.0422672851557336,
-2.93765));
#47655=CARTESIAN_POINT('Ctrl Pts',(0.134806053950555,-0.0521934162937557,
-2.93765));
#47656=CARTESIAN_POINT('Ctrl Pts',(0.133196241206826,-0.0580577957671597,
-2.93765));
#47657=CARTESIAN_POINT('Ctrl Pts',(0.131205098375125,-0.0638217359559869,
-2.93765));
#47658=CARTESIAN_POINT('Ctrl Pts',(0.128823493644037,-0.0694465980833095,
-2.93765));
#47659=CARTESIAN_POINT('Ctrl Pts',(-0.000893209148009566,0.117964196654764,
-2.93765));
#47660=CARTESIAN_POINT('Ctrl Pts',(-0.0369831781664475,0.117488069255602,
-2.93520197000608));
#47661=CARTESIAN_POINT('Ctrl Pts',(-0.0981247360162019,0.0868112407524339,
-2.93105639951488));
#47662=CARTESIAN_POINT('Ctrl Pts',(-0.117478474975439,0.0250944040704393,
-2.92691082902367));
#47663=CARTESIAN_POINT('Ctrl Pts',(-0.117640397146581,-8.56657636452585E-5,
-2.92521328852638));
#47664=CARTESIAN_POINT('Origin',(-3.28582941601228E-18,0.,-2.93765));
#47665=CARTESIAN_POINT('',(-0.111717694016329,0.0372841450039274,-2.93765));
#47666=CARTESIAN_POINT('Ctrl Pts',(0.0262268935511073,-0.144224038131951,
-2.93765));
#47667=CARTESIAN_POINT('Ctrl Pts',(0.0225529367225777,-0.144559449307367,
-2.93765));
#47668=CARTESIAN_POINT('Ctrl Pts',(0.018871621332308,-0.144745852633568,
-2.93765));
#47669=CARTESIAN_POINT('Ctrl Pts',(0.0151894836933861,-0.144777913300572,
-2.93765));
#47670=CARTESIAN_POINT('Ctrl Pts',(0.00801195125766715,-0.144840408649714,
-2.93765));
#47671=CARTESIAN_POINT('Ctrl Pts',(0.000830984588550291,-0.144317119643943,
-2.93765));
#47672=CARTESIAN_POINT('Ctrl Pts',(-0.0062939751165674,-0.143238551230609,
-2.93765));
#47673=CARTESIAN_POINT('Ctrl Pts',(-0.0109733672327204,-0.142530190097499,
-2.93765));
#47674=CARTESIAN_POINT('Ctrl Pts',(-0.0156307259998283,-0.141580965612318,
-2.93765));
#47675=CARTESIAN_POINT('Ctrl Pts',(-0.0202259413021322,-0.140404321648008,
-2.93765));
#47676=CARTESIAN_POINT('Ctrl Pts',(-0.0264890284927663,-0.138800604900045,
-2.93765));
#47677=CARTESIAN_POINT('Ctrl Pts',(-0.0326462411610736,-0.136773775845124,
-2.93765));
#47678=CARTESIAN_POINT('Ctrl Pts',(-0.0386527104818304,-0.13434452281258,
-2.93765));
#47679=CARTESIAN_POINT('Ctrl Pts',(-0.0417103306569216,-0.1331079006497,
-2.93765));
#47680=CARTESIAN_POINT('Ctrl Pts',(-0.0447288163869714,-0.131766884032008,
-2.93765));
#47681=CARTESIAN_POINT('Ctrl Pts',(-0.0477016792219733,-0.130323591521167,
-2.93765));
#47682=CARTESIAN_POINT('Ctrl Pts',(-0.0508144489056172,-0.128812375759888,
-2.93765));
#47683=CARTESIAN_POINT('Ctrl Pts',(-0.0538686917803179,-0.127193116028306,
-2.93765));
#47684=CARTESIAN_POINT('Ctrl Pts',(-0.0568558823257219,-0.125470616735044,
-2.93765));
#47685=CARTESIAN_POINT('Ctrl Pts',(-0.0653824269832697,-0.120553967822511,
-2.93765));
#47686=CARTESIAN_POINT('Ctrl Pts',(-0.0733713052120728,-0.114795730576438,
-2.93765));
#47687=CARTESIAN_POINT('Ctrl Pts',(-0.080650133064915,-0.108259608267344,
-2.93765));
#47688=CARTESIAN_POINT('Ctrl Pts',(-0.0835973555190745,-0.105613109844528,
-2.93765));
#47689=CARTESIAN_POINT('Ctrl Pts',(-0.0864276939354442,-0.102838727361706,
-2.93765));
#47690=CARTESIAN_POINT('Ctrl Pts',(-0.0891274150692409,-0.0999395069146105,
-2.93765));
#47691=CARTESIAN_POINT('Ctrl Pts',(-0.0911100509910371,-0.097810361599689,
-2.93765));
#47692=CARTESIAN_POINT('Ctrl Pts',(-0.0930196844243488,-0.0956163133794605,
-2.93765));
#47693=CARTESIAN_POINT('Ctrl Pts',(-0.0948462221025146,-0.0933654881788209,
-2.93765));
#47694=CARTESIAN_POINT('Ctrl Pts',(-0.0976832640047863,-0.0898694281274804,
-2.93765));
#47695=CARTESIAN_POINT('Ctrl Pts',(-0.100324145957716,-0.086232035159791,
-2.93765));
#47696=CARTESIAN_POINT('Ctrl Pts',(-0.102751026356172,-0.0824594073302338,
-2.93765));
#47697=CARTESIAN_POINT('Ctrl Pts',(-0.106748435662813,-0.0762453649711815,
-2.93765));
#47698=CARTESIAN_POINT('Ctrl Pts',(-0.110166211331277,-0.0696643617856752,
-2.93765));
#47699=CARTESIAN_POINT('Ctrl Pts',(-0.112992526824757,-0.0628009944060238,
-2.93765));
#47700=CARTESIAN_POINT('Ctrl Pts',(-0.114133115052098,-0.0600312130241466,
-2.93765));
#47701=CARTESIAN_POINT('Ctrl Pts',(-0.115177892243825,-0.0572131827636228,
-2.93765));
#47702=CARTESIAN_POINT('Ctrl Pts',(-0.116122837122688,-0.0543598758198917,
-2.93765));
#47703=CARTESIAN_POINT('Ctrl Pts',(-0.119054866830036,-0.0455064697532169,
-2.93765));
#47704=CARTESIAN_POINT('Ctrl Pts',(-0.121016207235663,-0.0363600245602272,
-2.93765));
#47705=CARTESIAN_POINT('Ctrl Pts',(-0.121991070818189,-0.027094190560155,
-2.93765));
#47706=CARTESIAN_POINT('Ctrl Pts',(-0.122559674353073,-0.0216897564828892,
-2.93765));
#47707=CARTESIAN_POINT('Ctrl Pts',(-0.122791706067432,-0.0162445702826281,
-2.93765));
#47708=CARTESIAN_POINT('Ctrl Pts',(-0.122676027364733,-0.0107949329128276,
-2.93765));
#47709=CARTESIAN_POINT('Ctrl Pts',(-0.122612206719513,-0.00778833476608035,
-2.93765));
#47710=CARTESIAN_POINT('Ctrl Pts',(-0.122442102964897,-0.00478029932637062,
-2.93765));
#47711=CARTESIAN_POINT('Ctrl Pts',(-0.12216540228983,-0.00179153671437861,
-2.93765));
#47712=CARTESIAN_POINT('Ctrl Pts',(-0.121359044251975,0.00691828213531097,
-2.93765));
#47713=CARTESIAN_POINT('Ctrl Pts',(-0.119650749016099,0.0154971799534183,
-2.93765));
#47714=CARTESIAN_POINT('Ctrl Pts',(-0.117001838809494,0.0237911387571977,
-2.93765));
#47715=CARTESIAN_POINT('Ctrl Pts',(-0.115534100011671,0.0283867513579932,
-2.93765));
#47716=CARTESIAN_POINT('Ctrl Pts',(-0.113776792745658,0.0328945535045048,
-2.93765));
#47717=CARTESIAN_POINT('Ctrl Pts',(-0.111717694016322,0.037284145003949,
-2.93765));
#47718=CARTESIAN_POINT('Origin',(0.,0.,-2.93765));
#47719=CARTESIAN_POINT('Origin',(0.,0.,-3.06008671147362));
#47720=CARTESIAN_POINT('Ctrl Pts',(-0.111717694016322,0.037284145003949,
-2.93765));
#47721=CARTESIAN_POINT('Ctrl Pts',(-0.115720921699064,0.0252889292013365,
-2.93679557049121));
#47722=CARTESIAN_POINT('Ctrl Pts',(-0.11762911624172,0.0126318964897331,
-2.93594114098241));
#47723=CARTESIAN_POINT('Ctrl Pts',(-0.117558445841294,-3.12605290917947E-5,
-2.93508671147362));
#47724=CARTESIAN_POINT('Ctrl Pts',(-0.138823048348883,0.046330160232009,
-2.95414778394209));
#47725=CARTESIAN_POINT('Ctrl Pts',(-0.15424614371138,0.000116611595973093,
-2.95149868683944));
#47726=CARTESIAN_POINT('Ctrl Pts',(-0.13504236871914,-0.108121172854393,
-2.94620049263414));
#47727=CARTESIAN_POINT('Ctrl Pts',(0.0180999205918092,-0.172211081102293,
-2.93825320132619));
#47728=CARTESIAN_POINT('Ctrl Pts',(0.15443488214358,-0.0779478857227474,
-2.93030591001824));
#47729=CARTESIAN_POINT('Ctrl Pts',(0.149227010588132,0.0876039139611851,
-2.92235861871029));
#47730=CARTESIAN_POINT('Ctrl Pts',(0.00709707033375117,0.17291318152139,
-2.91441132740233));
#47731=CARTESIAN_POINT('Ctrl Pts',(-0.141514212609231,0.0995730889212593,
-2.90646403609439));
#47732=CARTESIAN_POINT('Ctrl Pts',(-0.160345505504641,-0.0650644803652693,
-2.89851674478643));
#47733=CARTESIAN_POINT('Ctrl Pts',(-0.0321025340682361,-0.170041405975025,
-2.89056945347848));
#47734=CARTESIAN_POINT('Ctrl Pts',(0.125580313835011,-0.119050713111042,
-2.88262216217053));
#47735=CARTESIAN_POINT('Ctrl Pts',(0.168084926783387,0.0411272070241147,
-2.87467487086258));
#47736=CARTESIAN_POINT('Ctrl Pts',(0.0564234196368953,0.163586137243789,
-2.86672757955463));
#47737=CARTESIAN_POINT('Ctrl Pts',(-0.106988207737868,0.13600510865514,
-2.85878028824668));
#47738=CARTESIAN_POINT('Ctrl Pts',(-0.172272163300253,-0.0163171448586885,
-2.85083299693872));
#47739=CARTESIAN_POINT('Ctrl Pts',(-0.0795504967991995,-0.153673888715109,
-2.84288570563077));
#47740=CARTESIAN_POINT('Ctrl Pts',(0.0861336102392644,-0.150083061316343,
-2.83493841432282));
#47741=CARTESIAN_POINT('Ctrl Pts',(0.172817302014886,-0.00883838299254691,
-2.82699112301487));
#47742=CARTESIAN_POINT('Ctrl Pts',(0.100995520311121,0.140512776799912,
-2.81904383170691));
#47743=CARTESIAN_POINT('Ctrl Pts',(-0.0634578319565696,0.160987690016662,
-2.81109654039897));
#47744=CARTESIAN_POINT('Ctrl Pts',(-0.169708614925762,0.0338071110003193,
-2.80314924909101));
#47745=CARTESIAN_POINT('Ctrl Pts',(-0.120305186517372,-0.124380852578114,
-2.79520195778306));
#47746=CARTESIAN_POINT('Ctrl Pts',(0.0394403609169686,-0.168488551460744,
-2.78725466647511));
#47747=CARTESIAN_POINT('Ctrl Pts',(0.163011799154919,-0.0580610684788042,
-2.77930737516716));
#47748=CARTESIAN_POINT('Ctrl Pts',(0.137071248485045,0.105619160687613,
-2.77136008385921));
#47749=CARTESIAN_POINT('Ctrl Pts',(-0.0145890045231812,0.172427072037811,
-2.76341279255126));
#47750=CARTESIAN_POINT('Ctrl Pts',(-0.152868440543263,0.0810874475707317,
-2.7554655012433));
#47751=CARTESIAN_POINT('Ctrl Pts',(-0.150939225174926,-0.084624373309619,
-2.74751820993535));
#47752=CARTESIAN_POINT('Ctrl Pts',(-0.0105708060663173,-0.172719982367763,
-2.7395709186274));
#47753=CARTESIAN_POINT('Ctrl Pts',(0.139492998563312,-0.102399402381208,
-2.73162362731945));
#47754=CARTESIAN_POINT('Ctrl Pts',(0.16161590755552,0.0618403806498103,
-2.7236763360115));
#47755=CARTESIAN_POINT('Ctrl Pts',(0.0355071190986658,0.169361089825304,
-2.71572904470354));
#47756=CARTESIAN_POINT('Ctrl Pts',(-0.123168268870792,0.121546336011192,
-2.7077817533956));
#47757=CARTESIAN_POINT('Ctrl Pts',(-0.168875559555085,-0.0377489024866377,
-2.69983446208764));
#47758=CARTESIAN_POINT('Ctrl Pts',(-0.0596927083592543,-0.162421411220021,
-2.69188717077969));
#47759=CARTESIAN_POINT('Ctrl Pts',(0.104239403721097,-0.138123426564634,
-2.68393987947174));
#47760=CARTESIAN_POINT('Ctrl Pts',(0.172564691021556,0.0128593027283262,
-2.67599258816379));
#47761=CARTESIAN_POINT('Ctrl Pts',(0.0826162201395204,0.152047671550354,
-2.66804529685583));
#47762=CARTESIAN_POINT('Ctrl Pts',(-0.0831066143792944,0.151780186126033,
-2.66009800554788));
#47763=CARTESIAN_POINT('Ctrl Pts',(-0.172605302986316,0.0123021800927432,
-2.65215071423994));
#47764=CARTESIAN_POINT('Ctrl Pts',(-0.103792984723003,-0.138459201847778,
-2.64420342293198));
#47765=CARTESIAN_POINT('Ctrl Pts',(0.0602167094800405,-0.162227871074707,
-2.63625613162403));
#47766=CARTESIAN_POINT('Ctrl Pts',(0.168996536794456,-0.0372035590436465,
-2.62830884031608));
#47767=CARTESIAN_POINT('Ctrl Pts',(0.122775263710156,0.12194330188631,-2.62036154900813));
#47768=CARTESIAN_POINT('Ctrl Pts',(-0.0360536481919909,0.169245586961913,
-2.61241425770017));
#47769=CARTESIAN_POINT('Ctrl Pts',(-0.161814692259995,0.0613183465435701,
-2.60446696639222));
#47770=CARTESIAN_POINT('Ctrl Pts',(-0.139161716510039,-0.102849165830422,
-2.59651967508427));
#47771=CARTESIAN_POINT('Ctrl Pts',(0.0111283079130825,-0.172684958861581,
-2.58857238377632));
#47772=CARTESIAN_POINT('Ctrl Pts',(0.151211614465995,-0.0841366858428694,
-2.58062509246837));
#47773=CARTESIAN_POINT('Ctrl Pts',(0.152605885847715,0.0815804992548367,
-2.57267780116042));
#47774=CARTESIAN_POINT('Ctrl Pts',(0.014032317163657,0.172473268447759,
-2.56473050985246));
#47775=CARTESIAN_POINT('Ctrl Pts',(-0.137411483317849,0.105176130877793,
-2.55678321854451));
#47776=CARTESIAN_POINT('Ctrl Pts',(-0.162823522878765,-0.058586983634443,
-2.54883592723656));
#47777=CARTESIAN_POINT('Ctrl Pts',(-0.0388962582402102,-0.168614991471532,
-2.54088863592861));
#47778=CARTESIAN_POINT('Ctrl Pts',(0.120706073728026,-0.12399184658355,
-2.53294134462066));
#47779=CARTESIAN_POINT('Ctrl Pts',(0.169598597036642,0.0343547687699517,
-2.52499405331271));
#47780=CARTESIAN_POINT('Ctrl Pts',(0.0629378192812766,0.161191703130625,
-2.51704676200475));
#47781=CARTESIAN_POINT('Ctrl Pts',(-0.10144858664574,0.140186014001455,
-2.5090994706968));
#47782=CARTESIAN_POINT('Ctrl Pts',(-0.172787863547209,-0.0093961941670593,
-2.50115217938885));
#47783=CARTESIAN_POINT('Ctrl Pts',(-0.0856486917575374,-0.150360353332441,
-2.4932048880809));
#47784=CARTESIAN_POINT('Ctrl Pts',(0.0800461813615386,-0.153416241328843,
-2.48525759677295));
#47785=CARTESIAN_POINT('Ctrl Pts',(0.172323892039918,-0.0157610433109308,
-2.477310305465));
#47786=CARTESIAN_POINT('Ctrl Pts',(0.106548701766463,0.136349948316512,
-2.46936301415705));
#47787=CARTESIAN_POINT('Ctrl Pts',(-0.0569513669756151,0.163402803077679,
-2.46141572284909));
#47788=CARTESIAN_POINT('Ctrl Pts',(-0.168216492221969,0.0405850464896916,
-2.45346843154115));
#47789=CARTESIAN_POINT('Ctrl Pts',(-0.125195962305283,-0.119456708796486,
-2.44552114023319));
#47790=CARTESIAN_POINT('Ctrl Pts',(0.0326524350392282,-0.169934554285005,
-2.43757384892524));
#47791=CARTESIAN_POINT('Ctrl Pts',(0.160552506472577,-0.064550963737247,
-2.42962655761728));
#47792=CARTESIAN_POINT('Ctrl Pts',(0.141196216047521,0.100037806992637,
-2.42167926630934));
#47793=CARTESIAN_POINT('Ctrl Pts',(-0.00766313565102988,0.172873394731602,
-2.41373197500138));
#47794=CARTESIAN_POINT('Ctrl Pts',(-0.14949397374247,0.0871520858540961,
-2.40578468369343));
#47795=CARTESIAN_POINT('Ctrl Pts',(-0.154211171089647,-0.078503814972228,
-2.39783739238548));
#47796=CARTESIAN_POINT('Ctrl Pts',(-0.017488184714347,-0.172157188782319,
-2.38989010107753));
#47797=CARTESIAN_POINT('Ctrl Pts',(0.135274703579161,-0.107910559379536,
-2.38194280976958));
#47798=CARTESIAN_POINT('Ctrl Pts',(0.163965653425891,0.0553100239617989,
-2.37399551846162));
#47799=CARTESIAN_POINT('Ctrl Pts',(0.0422697539875444,0.16780107911413,
-2.36604822715368));
#47800=CARTESIAN_POINT('Ctrl Pts',(-0.118195332713031,0.126387489803738,
-2.35810093584572));
#47801=CARTESIAN_POINT('Ctrl Pts',(-0.170253424927118,-0.0309468181663384,
-2.35015364453777));
#47802=CARTESIAN_POINT('Ctrl Pts',(-0.0661576177127792,-0.159897166555896,
-2.34220635322982));
#47803=CARTESIAN_POINT('Ctrl Pts',(0.0986169687224061,-0.142192221074285,
-2.33425906192187));
#47804=CARTESIAN_POINT('Ctrl Pts',(0.172941543814754,0.0059293066208318,
-2.32631177061392));
#47805=CARTESIAN_POINT('Ctrl Pts',(0.088646716969042,0.148612562808953,
-2.31836447930597));
#47806=CARTESIAN_POINT('Ctrl Pts',(-0.0769535551690017,0.154990595201404,
-2.31041718799801));
#47807=CARTESIAN_POINT('Ctrl Pts',(-0.171973175436669,0.0192135677130206,
-2.30246989669006));
#47808=CARTESIAN_POINT('Ctrl Pts',(-0.10926156678474,-0.134185857219671,
-2.29452260538211));
#47809=CARTESIAN_POINT('Ctrl Pts',(0.0536631196270061,-0.164512017329835,
-2.28657531407415));
#47810=CARTESIAN_POINT('Ctrl Pts',(0.167368793917039,-0.0439502113395367,
-2.27862802276621));
#47811=CARTESIAN_POINT('Ctrl Pts',(0.127566309273023,0.116922072306703,
-2.27068073145825));
#47812=CARTESIAN_POINT('Ctrl Pts',(-0.0292380896479154,0.170555176901126,
-2.26273344015031));
#47813=CARTESIAN_POINT('Ctrl Pts',(-0.159225749273804,0.0677576196617771,
-2.25478614884235));
#47814=CARTESIAN_POINT('Ctrl Pts',(-0.143173928935275,-0.0971862146977188,
-2.2468388575344));
#47815=CARTESIAN_POINT('Ctrl Pts',(0.00419488140978216,-0.172992303944401,
-2.23889156622645));
#47816=CARTESIAN_POINT('Ctrl Pts',(0.147716209156132,-0.0901324348199692,
-2.2309442749185));
#47817=CARTESIAN_POINT('Ctrl Pts',(0.155754435294457,0.0753955578276256,
-2.22299698361055));
#47818=CARTESIAN_POINT('Ctrl Pts',(0.0209370188228705,0.17177187050517,
-2.2150496923026));
#47819=CARTESIAN_POINT('Ctrl Pts',(-0.133083518719539,0.11060158814077,
-2.20710240099464));
#47820=CARTESIAN_POINT('Ctrl Pts',(-0.165041839853626,-0.0520108195644357,
-2.19915510968669));
#47821=CARTESIAN_POINT('Ctrl Pts',(-0.0456262495787772,-0.166919680096175,
-2.19120781837874));
#47822=CARTESIAN_POINT('Ctrl Pts',(0.115637055601487,-0.12873230218501,
-2.18326052707079));
#47823=CARTESIAN_POINT('Ctrl Pts',(0.170839779866426,0.0275264212934636,
-2.17531323576284));
#47824=CARTESIAN_POINT('Ctrl Pts',(0.0693508087069927,0.15853832213607,
-2.16736594445488));
#47825=CARTESIAN_POINT('Ctrl Pts',(-0.0957456887782547,0.144141240921575,
-2.15941865314693));
#47826=CARTESIAN_POINT('Ctrl Pts',(-0.173025670016707,-0.00246003441113623,
-2.15147136183898));
#47827=CARTESIAN_POINT('Ctrl Pts',(-0.0916090900206878,-0.146805002910718,
-2.14352407053103));
#47828=CARTESIAN_POINT('Ctrl Pts',(0.0738299796018623,-0.156502614566092,
-2.13557677922308));
#47829=CARTESIAN_POINT('Ctrl Pts',(0.171553294228662,-0.022658364754064,
-2.12762948791513));
#47830=CARTESIAN_POINT('Ctrl Pts',(0.111930488710947,0.131967798916868,
-2.11968219660717));
#47831=CARTESIAN_POINT('Ctrl Pts',(-0.0503532899098111,0.165555067724588,
-2.11173490529923));
#47832=CARTESIAN_POINT('Ctrl Pts',(-0.166453782809105,0.0472977001827116,
-2.10378761399127));
#47833=CARTESIAN_POINT('Ctrl Pts',(-0.129885351301263,-0.114340411803446,
-2.09584032268332));
#47834=CARTESIAN_POINT('Ctrl Pts',(0.0258119852080813,-0.171107205206712,
-2.08789303137537));
#47835=CARTESIAN_POINT('Ctrl Pts',(0.157834954262227,-0.0709370246562046,
-2.07994574006742));
#47836=CARTESIAN_POINT('Ctrl Pts',(0.14509405977175,0.0942955358062407,
-2.07199844875947));
#47837=CARTESIAN_POINT('Ctrl Pts',(-0.000724940060565141,0.173041638676773,
-2.06405115745151));
#47838=CARTESIAN_POINT('Ctrl Pts',(-0.145879035692817,0.0930765340962364,
-2.05610386614356));
#47839=CARTESIAN_POINT('Ctrl Pts',(-0.157235057788262,-0.0722569779077145,
-2.04815657483561));
#47840=CARTESIAN_POINT('Ctrl Pts',(-0.0243774324284428,-0.171317468584586,
-2.04020928352766));
#47841=CARTESIAN_POINT('Ctrl Pts',(0.130838809995228,-0.11324813487677,
-2.03226199221971));
#47842=CARTESIAN_POINT('Ctrl Pts',(0.166051649338603,0.0486906973246862,
-2.02431470091175));
#47843=CARTESIAN_POINT('Ctrl Pts',(0.0489643950900598,0.165971148900942,
-2.01636740960381));
#47844=CARTESIAN_POINT('Ctrl Pts',(-0.113032271287723,0.131025340684818,
-2.00842011829585));
#47845=CARTESIAN_POINT('Ctrl Pts',(-0.17135742603286,-0.0240949537751543,
-2.0004728269879));
#47846=CARTESIAN_POINT('Ctrl Pts',(-0.0725161080183242,-0.157115716374617,
-1.99252553567995));
#47847=CARTESIAN_POINT('Ctrl Pts',(0.0928359015918849,-0.146032289681619,
-1.984578244372));
#47848=CARTESIAN_POINT('Ctrl Pts',(0.17304020831898,-0.00101022718139327,
-1.97663095306405));
#47849=CARTESIAN_POINT('Ctrl Pts',(0.0945346194978198,0.144938400606728,
-1.96868366175609));
#47850=CARTESIAN_POINT('Ctrl Pts',(-0.0706767109076062,0.157951691315151,
-1.96073637044814));
#47851=CARTESIAN_POINT('Ctrl Pts',(-0.171064417284779,0.0260940489969148,
-1.95278907914019));
#47852=CARTESIAN_POINT('Ctrl Pts',(-0.114554394151342,-0.129696665472376,
-1.94484178783224));
#47853=CARTESIAN_POINT('Ctrl Pts',(0.0470232089796812,-0.166531534765303,
-1.93689449652429));
#47854=CARTESIAN_POINT('Ctrl Pts',(0.165471826899637,-0.0506261667177226,
-1.92894720521634));
#47855=CARTESIAN_POINT('Ctrl Pts',(0.132152155711843,0.111712765585439,
-1.92099991390838));
#47856=CARTESIAN_POINT('Ctrl Pts',(-0.0223754996390369,0.171590417185628,
-1.91305262260043));
#47857=CARTESIAN_POINT('Ctrl Pts',(-0.156380680791286,0.0740879000194224,
-1.90510533129248));
#47858=CARTESIAN_POINT('Ctrl Pts',(-0.146955836313892,-0.0913669328987178,
-1.89715803998453));
#47859=CARTESIAN_POINT('Ctrl Pts',(-0.00274529284687124,-0.173021379087149,
-1.88921074867658));
#47860=CARTESIAN_POINT('Ctrl Pts',(0.143983192231577,-0.0959831996176365,
-1.88126345736863));
#47861=CARTESIAN_POINT('Ctrl Pts',(0.158652443090577,0.0690893374944751,
-1.87331616606068));
#47862=CARTESIAN_POINT('Ctrl Pts',(0.0278080418568483,0.170794165773079,
-1.86536887475272));
#47863=CARTESIAN_POINT('Ctrl Pts',(-0.128541480188837,0.115849135192702,
-1.85742158344477));
#47864=CARTESIAN_POINT('Ctrl Pts',(-0.166994675753097,-0.0453509925376745,
-1.84947429213682));
#47865=CARTESIAN_POINT('Ctrl Pts',(-0.0522828479776232,-0.164955867011098,
-1.84152700082887));
#47866=CARTESIAN_POINT('Ctrl Pts',(0.110382027370459,-0.133265683083161,
-1.83357970952092));
#47867=CARTESIAN_POINT('Ctrl Pts',(0.171806155238182,0.0206537956876658,
-1.82563241821296));
#47868=CARTESIAN_POINT('Ctrl Pts',(0.0756522426187192,0.155629921418706,
-1.81768512690501));
#47869=CARTESIAN_POINT('Ctrl Pts',(-0.0898887774288336,0.147864606807659,
-1.80973783559706));
#47870=CARTESIAN_POINT('Ctrl Pts',(-0.172985152874525,0.00448008247821151,
-1.80179054428911));
#47871=CARTESIAN_POINT('Ctrl Pts',(-0.0974221288036245,-0.143013506611804,
-1.79384325298116));
#47872=CARTESIAN_POINT('Ctrl Pts',(0.0674950172757856,-0.159337242655242,
-1.7858959616732));
#47873=CARTESIAN_POINT('Ctrl Pts',(0.170506741222779,-0.0295192386694261,
-1.77794867036526));
#47874=CARTESIAN_POINT('Ctrl Pts',(0.117132227817026,0.127373370296363,
-1.7700013790573));
#47875=CARTESIAN_POINT('Ctrl Pts',(-0.0436742161369485,0.167441025734009,
-1.76205408774936));
#47876=CARTESIAN_POINT('Ctrl Pts',(-0.164423321114139,0.0539342722935164,
-1.7541067964414));
#47877=CARTESIAN_POINT('Ctrl Pts',(-0.134365810835652,-0.109040190446056,
-1.74615950513345));
#47878=CARTESIAN_POINT('Ctrl Pts',(0.0189300150352012,-0.172004618498461,
-1.7382122138255));
#47879=CARTESIAN_POINT('Ctrl Pts',(0.154863513744348,-0.0772089785244452,
-1.73026492251755));
#47880=CARTESIAN_POINT('Ctrl Pts',(0.148758509787723,0.088401583808041,
-1.72231763120959));
#47881=CARTESIAN_POINT('Ctrl Pts',(0.00621442164551661,0.172931533323585,
-1.71437033990164));
#47882=CARTESIAN_POINT('Ctrl Pts',(-0.142029441247508,0.0988512623741091,
-1.70642304859369));
#47883=CARTESIAN_POINT('Ctrl Pts',(-0.160006021153813,-0.0658939105574994,
-1.69847575728574));
#47884=CARTESIAN_POINT('Ctrl Pts',(-0.0312274673769587,-0.170202172533887,
-1.69052846597779));
#47885=CARTESIAN_POINT('Ctrl Pts',(0.126192453246251,-0.118403543011715,
-1.68258117466984));
#47886=CARTESIAN_POINT('Ctrl Pts',(0.167870539828374,0.0419930483742822,
-1.67463388336188));
#47887=CARTESIAN_POINT('Ctrl Pts',(0.0555802736177277,0.163874242755269,
-1.66668659205393));
#47888=CARTESIAN_POINT('Ctrl Pts',(-0.107687389731462,0.135452428353494,
-1.65873930074598));
#47889=CARTESIAN_POINT('Ctrl Pts',(-0.172185787011349,-0.0172043310046124,
-1.65079200943803));
#47890=CARTESIAN_POINT('Ctrl Pts',(-0.0787579512096747,-0.154081534829091,
-1.64284471813008));
#47891=CARTESIAN_POINT('Ctrl Pts',(0.0869055015709199,-0.149637455373784,
-1.63489742682213));
#47892=CARTESIAN_POINT('Ctrl Pts',(0.172860525825677,-0.00794813596417602,
-1.62695013551418));
#47893=CARTESIAN_POINT('Ctrl Pts',(0.10027045663234,0.141031095084652,-1.61900284420622));
#47894=CARTESIAN_POINT('Ctrl Pts',(-0.064286178327947,0.160658711341843,
-1.61105555289827));
#47895=CARTESIAN_POINT('Ctrl Pts',(-0.169880490330225,0.0329325562201978,
-1.60310826159032));
#47896=CARTESIAN_POINT('Ctrl Pts',(-0.119662952948367,-0.124998847777535,
-1.59516097028237));
#47897=CARTESIAN_POINT('Ctrl Pts',(0.0403076582879941,-0.168283174849338,
-1.58721367897441));
#47898=CARTESIAN_POINT('Ctrl Pts',(0.163308687143305,-0.0572206864478598,
-1.57926638766647));
#47899=CARTESIAN_POINT('Ctrl Pts',(0.1365254263793,0.106323761248294,-1.57131909635851));
#47900=CARTESIAN_POINT('Ctrl Pts',(-0.015476917110248,0.172349642560687,
-1.56337180505056));
#47901=CARTESIAN_POINT('Ctrl Pts',(-0.153284063299477,0.0802990049280576,
-1.55542451374261));
#47902=CARTESIAN_POINT('Ctrl Pts',(-0.150501355189484,-0.0854006811457802,
-1.54747722243466));
#47903=CARTESIAN_POINT('Ctrl Pts',(-0.00968105111241323,-0.172772137520472,
-1.53952993112671));
#47904=CARTESIAN_POINT('Ctrl Pts',(0.1400185685051,-0.101679568880954,-1.53158263981875));
#47905=CARTESIAN_POINT('Ctrl Pts',(0.161295247592536,0.0626719822416413,
-1.52363534851081));
#47906=CARTESIAN_POINT('Ctrl Pts',(0.0346343337556016,0.169541726956345,
-1.51568805720285));
#47907=CARTESIAN_POINT('Ctrl Pts',(-0.123792673905044,0.120910330995634,
-1.5077407658949));
#47908=CARTESIAN_POINT('Ctrl Pts',(-0.16867888930721,-0.0386182153409498,
-1.49979347458695));
#47909=CARTESIAN_POINT('Ctrl Pts',(-0.0588553458434272,-0.162726711143821,
-1.491846183279));
#47910=CARTESIAN_POINT('Ctrl Pts',(0.104949442106884,-0.137584697025097,
-1.48389889197105));
#47911=CARTESIAN_POINT('Ctrl Pts',(0.172496168671101,0.0137479470403931,
-1.47595160066309));
#47912=CARTESIAN_POINT('Ctrl Pts',(0.0818319847294822,0.152471179339796,
-1.46800430935515));
#47913=CARTESIAN_POINT('Ctrl Pts',(-0.0838872738395407,0.151350122371288,
-1.46005701804719));
#47914=CARTESIAN_POINT('Ctrl Pts',(-0.172666377295255,0.0114129928488046,
-1.45210972673924));
#47915=CARTESIAN_POINT('Ctrl Pts',(-0.103078457436309,-0.138991963316535,
-1.44416243543129));
#47916=CARTESIAN_POINT('Ctrl Pts',(0.0610514846030254,-0.161915565903346,
-1.43621514412334));
#47917=CARTESIAN_POINT('Ctrl Pts',(0.16918591647428,-0.0363326288725753,
-1.42826785281538));
#47918=CARTESIAN_POINT('Ctrl Pts',(0.122145551731954,0.122574052907337,
-1.42032056150743));
#47919=CARTESIAN_POINT('Ctrl Pts',(-0.0369248894035242,0.169057643413635,
-1.41237327019948));
#47920=CARTESIAN_POINT('Ctrl Pts',(-0.162128373273433,0.0604840874424386,
-1.40442597889153));
#47921=CARTESIAN_POINT('Ctrl Pts',(-0.138630133783172,-0.10356457049249,
-1.39647868758358));
#47922=CARTESIAN_POINT('Ctrl Pts',(0.0120175946397989,-0.17262535060966,
-1.38853139627563));
#47923=CARTESIAN_POINT('Ctrl Pts',(0.15164296468403,-0.0833567364756583,
-1.38058410496768));
#47924=CARTESIAN_POINT('Ctrl Pts',(0.152183671577224,0.0823654318225178,
-1.37263681365972));
#47925=CARTESIAN_POINT('Ctrl Pts',(0.0131437870297985,0.172543255784019,
-1.36468952235177));
#47926=CARTESIAN_POINT('Ctrl Pts',(-0.137951382742217,0.104466981642739,
-1.35674223104382));
#47927=CARTESIAN_POINT('Ctrl Pts',(-0.162519603902411,-0.0594248483501469,
-1.34879493973587));
#47928=CARTESIAN_POINT('Ctrl Pts',(-0.0380272708106778,-0.168813094660117,
-1.34084764842792));
#47929=CARTESIAN_POINT('Ctrl Pts',(0.12134310731451,-0.123368490958159,
-1.33290035711997));
#47930=CARTESIAN_POINT('Ctrl Pts',(0.169419399085581,0.0352278507365205,
-1.32495306581201));
#47931=CARTESIAN_POINT('Ctrl Pts',(0.0621067474779282,0.161513733693909,
-1.31700577450406));
#47932=CARTESIAN_POINT('Ctrl Pts',(-0.1021692856514,0.139661631536786,-1.30905848319611));
#47933=CARTESIAN_POINT('Ctrl Pts',(-0.172737175387357,-0.010286033892214,
-1.30111119188816));
#47934=CARTESIAN_POINT('Ctrl Pts',(-0.0848731068556039,-0.150799502607639,
-1.29316390058021));
#47935=CARTESIAN_POINT('Ctrl Pts',(0.080835308113122,-0.153001918995452,
-1.28521660927226));
#47936=CARTESIAN_POINT('Ctrl Pts',(0.172402785366406,-0.0148732596272302,
-1.2772693179643));
#47937=CARTESIAN_POINT('Ctrl Pts',(0.105845001886694,0.136896931410605,
-1.26932202665635));
#47938=CARTESIAN_POINT('Ctrl Pts',(-0.0577922370382871,0.16310730085482,
-1.2613747353484));
#47939=CARTESIAN_POINT('Ctrl Pts',(-0.168423299000403,0.0397180891767819,
-1.25342744404045));
#47940=CARTESIAN_POINT('Ctrl Pts',(-0.124579025709963,-0.120099960895874,
-1.2454801527325));
#47941=CARTESIAN_POINT('Ctrl Pts',(0.0335272699740489,-0.169764119949185,
-1.23753286142455));
#47942=CARTESIAN_POINT('Ctrl Pts',(0.160882854206129,-0.0637231627944186,
-1.22958557011659));
#47943=CARTESIAN_POINT('Ctrl Pts',(0.140679086570741,0.100763727876932,
-1.22163827880865));
#47944=CARTESIAN_POINT('Ctrl Pts',(-0.00855343890287729,0.172831631760418,
-1.21369098750069));
#47945=CARTESIAN_POINT('Ctrl Pts',(-0.149940877919179,0.0863809434010756,
-1.20574369619274));
#47946=CARTESIAN_POINT('Ctrl Pts',(-0.153804782352703,-0.0792970565624726,
-1.19779640488479));
#47947=CARTESIAN_POINT('Ctrl Pts',(-0.016601236745816,-0.172244980166459,
-1.18984911357684));
#47948=CARTESIAN_POINT('Ctrl Pts',(0.135828715344837,-0.107212379610778,
-1.18190182226888));
#47949=CARTESIAN_POINT('Ctrl Pts',(0.16367859766873,0.0561538148235014,
-1.17395453096093));
#47950=CARTESIAN_POINT('Ctrl Pts',(0.04140491396222,0.168016568688374,-1.16600723965298));
#47951=CARTESIAN_POINT('Ctrl Pts',(-0.11884473864751,0.125777034270327,
-1.15805994834503));
#47952=CARTESIAN_POINT('Ctrl Pts',(-0.170091771343399,-0.0318233181063728,
-1.15011265703708));
#47953=CARTESIAN_POINT('Ctrl Pts',(-0.0653331708643289,-0.160235798243859,
-1.14216536572913));
#47954=CARTESIAN_POINT('Ctrl Pts',(0.0993480384953303,-0.141682396581807,
-1.13421807442118));
#47955=CARTESIAN_POINT('Ctrl Pts',(0.17290871023143,0.00681998388102105,
-1.12627078311322));
#47956=CARTESIAN_POINT('Ctrl Pts',(0.0878800945018856,0.149067176951782,
-1.11832349180527));
#47957=CARTESIAN_POINT('Ctrl Pts',(-0.0777508318389294,0.154592180922545,
-1.11037620049732));
#47958=CARTESIAN_POINT('Ctrl Pts',(-0.172069856051197,0.018327544640642,
-1.10242890918937));
#47959=CARTESIAN_POINT('Ctrl Pts',(-0.10856897732768,-0.134746841952068,
-1.09448161788142));
#47960=CARTESIAN_POINT('Ctrl Pts',(0.0545097464461239,-0.1642334369013,
-1.08653432657347));
#47961=CARTESIAN_POINT('Ctrl Pts',(0.167592944620013,-0.0430875755598672,
-1.07858703526552));
#47962=CARTESIAN_POINT('Ctrl Pts',(0.126962396181698,0.117577566779703,
-1.07063974395756));
#47963=CARTESIAN_POINT('Ctrl Pts',(-0.0301161664627092,0.170402320323477,
-1.06269245264961));
#47964=CARTESIAN_POINT('Ctrl Pts',(-0.159572630867386,0.0669366098043176,
-1.05474516134166));
#47965=CARTESIAN_POINT('Ctrl Pts',(-0.142671460689015,-0.0979223598515507,
-1.04679787003371));
#47966=CARTESIAN_POINT('Ctrl Pts',(0.0050858431223512,-0.172968403050293,
-1.03885057872576));
#47967=CARTESIAN_POINT('Ctrl Pts',(0.148178487554465,-0.0893704094211579,
-1.03090328741781));
#47968=CARTESIAN_POINT('Ctrl Pts',(0.155364035533507,0.0761967894125327,
-1.02295599610985));
#47969=CARTESIAN_POINT('Ctrl Pts',(0.0200520097346351,0.171877430629029,
-1.0150087048019));
#47970=CARTESIAN_POINT('Ctrl Pts',(-0.133651420012675,0.109914658634004,
-1.00706141349395));
#47971=CARTESIAN_POINT('Ctrl Pts',(-0.164771762764467,-0.0528601972142011,
-0.999114122185998));
#47972=CARTESIAN_POINT('Ctrl Pts',(-0.0447659047812013,-0.167152469389939,
-0.991166830878048));
#47973=CARTESIAN_POINT('Ctrl Pts',(0.116298572704249,-0.128134992258121,
-0.983219539570095));
#47974=CARTESIAN_POINT('Ctrl Pts',(0.170695735664292,0.028405986694009,
-0.975272248262145));
#47975=CARTESIAN_POINT('Ctrl Pts',(0.0685333183915558,0.158893418756964,
-0.967324956954192));
#47976=CARTESIAN_POINT('Ctrl Pts',(-0.0964868352949552,0.143646179443793,
-0.959377665646241));
#47977=CARTESIAN_POINT('Ctrl Pts',(-0.173010704215006,-0.00335119099153059,
-0.95143037433829));
#47978=CARTESIAN_POINT('Ctrl Pts',(-0.0908517383104639,-0.147274899083318,
-0.943483083030339));
#47979=CARTESIAN_POINT('Ctrl Pts',(0.0746350855393954,-0.156120268577023,
-0.935535791722385));
#47980=CARTESIAN_POINT('Ctrl Pts',(0.171667723247975,-0.0217744586359998,
-0.927588500414436));
#47981=CARTESIAN_POINT('Ctrl Pts',(0.111249288223971,0.132542559669315,
-0.919641209106481));
#47982=CARTESIAN_POINT('Ctrl Pts',(-0.0512053329868681,0.165293521130557,
-0.911693917798533));
#47983=CARTESIAN_POINT('Ctrl Pts',(-0.166695187287125,0.0464397328733114,
-0.903746626490578));
#47984=CARTESIAN_POINT('Ctrl Pts',(-0.129294704597221,-0.115007885021643,
-0.89579933518263));
#47985=CARTESIAN_POINT('Ctrl Pts',(0.0266929507556997,-0.170971987863474,
-0.887852043874675));
#47986=CARTESIAN_POINT('Ctrl Pts',(0.158198230206126,-0.0701231360799296,
-0.879904752566726));
#47987=CARTESIAN_POINT('Ctrl Pts',(0.144606454839957,0.0950416091649022,
-0.871957461258772));
#47988=CARTESIAN_POINT('Ctrl Pts',(-0.00161620190464337,0.173035609472263,
-0.864010169950822));
#47989=CARTESIAN_POINT('Ctrl Pts',(-0.146356502392492,0.0923239322249147,
-0.85606287864287));
#47990=CARTESIAN_POINT('Ctrl Pts',(-0.156860804015258,-0.0730658772459555,
-0.848115587334918));
#47991=CARTESIAN_POINT('Ctrl Pts',(-0.0234947181556815,-0.171440754993727,
-0.840168296026968));
#47992=CARTESIAN_POINT('Ctrl Pts',(0.131420372415852,-0.112572731903036,
-0.832221004719014));
#47993=CARTESIAN_POINT('Ctrl Pts',(0.165798659537729,0.0495453201576731,
-0.824273713411065));
#47994=CARTESIAN_POINT('Ctrl Pts',(0.048108891535868,0.166221144290443,
-0.816326422103112));
#47995=CARTESIAN_POINT('Ctrl Pts',(-0.113705633508154,0.130441416592061,
-0.808379130795161));
#47996=CARTESIAN_POINT('Ctrl Pts',(-0.171231049144374,-0.0249772308903897,
-0.800431839487209));
#47997=CARTESIAN_POINT('Ctrl Pts',(-0.0717059030162035,-0.157487135114794,
-0.792484548179257));
#47998=CARTESIAN_POINT('Ctrl Pts',(0.0935868267762013,-0.145552190323593,
-0.784537256871307));
#47999=CARTESIAN_POINT('Ctrl Pts',(0.173043116317887,-0.000118949688376935,
-0.776589965563353));
#48000=CARTESIAN_POINT('Ctrl Pts',(0.0937868431381373,0.145423389825078,
-0.768642674255404));
#48001=CARTESIAN_POINT('Ctrl Pts',(-0.0714893223132149,0.157585567388741,
-0.76069538294745));
#48002=CARTESIAN_POINT('Ctrl Pts',(-0.171196548687525,0.0252126153247527,
-0.7527480916395));
#48003=CARTESIAN_POINT('Ctrl Pts',(-0.113884856601376,-0.130284971086147,
-0.744800800331547));
#48004=CARTESIAN_POINT('Ctrl Pts',(0.0478803256378469,-0.166287127195246,
-0.736853509023597));
#48005=CARTESIAN_POINT('Ctrl Pts',(0.165730388064043,-0.0497732129380442,
-0.728906217715644));
#48006=CARTESIAN_POINT('Ctrl Pts',(0.13157501294286,0.112391949102775,-0.720958926407693));
#48007=CARTESIAN_POINT('Ctrl Pts',(-0.0232589996105465,0.171472893458854,
-0.713011635099741));
#48008=CARTESIAN_POINT('Ctrl Pts',(-0.156760204982269,0.0732814600560811,
-0.70506434379179));
#48009=CARTESIAN_POINT('Ctrl Pts',(-0.146483290802742,-0.0921226344045439,
-0.697117052483838));
#48010=CARTESIAN_POINT('Ctrl Pts',(-0.0018540893212253,-0.173033223997078,
-0.689169761175886));
#48011=CARTESIAN_POINT('Ctrl Pts',(0.144475655203828,-0.0952403239571285,
-0.681222469867936));
#48012=CARTESIAN_POINT('Ctrl Pts',(0.158294485823848,0.0699055792608682,
-0.673275178559983));
#48013=CARTESIAN_POINT('Ctrl Pts',(0.0269279774118191,0.170935128883862,
-0.665327887252032));
#48014=CARTESIAN_POINT('Ctrl Pts',(-0.12913646984271,0.115185530387271,
-0.65738059594408));
#48015=CARTESIAN_POINT('Ctrl Pts',(-0.166758874988585,-0.0462105168395193,
-0.649433304636128));
#48016=CARTESIAN_POINT('Ctrl Pts',(-0.0514325297353875,-0.165222967952561,
-0.641486013328178));
#48017=CARTESIAN_POINT('Ctrl Pts',(0.111066963894049,-0.132695379668595,
-0.633538722020224));
#48018=CARTESIAN_POINT('Ctrl Pts',(0.171697496489914,0.0215384296811568,
-0.625591430712274));
#48019=CARTESIAN_POINT('Ctrl Pts',(0.0748496487802092,0.156017512900038,
-0.617644139404321));
#48020=CARTESIAN_POINT('Ctrl Pts',(-0.0906491792717766,0.147399662656966,
-0.609696848096371));
#48021=CARTESIAN_POINT('Ctrl Pts',(-0.173005933504491,0.0035890425288093,
-0.601749556788418));
#48022=CARTESIAN_POINT('Ctrl Pts',(-0.096684228537071,-0.143513393821711,
-0.593802265480468));
#48023=CARTESIAN_POINT('Ctrl Pts',(0.0683148073313607,-0.158987488040138,
-0.585854974172515));
#48024=CARTESIAN_POINT('Ctrl Pts',(0.170656521868019,-0.0286406319403842,
-0.577907682864565));
#48025=CARTESIAN_POINT('Ctrl Pts',(0.116474622480369,0.127974984165225,
-0.569960391556612));
#48026=CARTESIAN_POINT('Ctrl Pts',(-0.0445360616588884,0.167213855484376,
-0.562013100248662));
#48027=CARTESIAN_POINT('Ctrl Pts',(-0.164698934976151,0.053086675086657,
-0.554065808940708));
#48028=CARTESIAN_POINT('Ctrl Pts',(-0.133802404118461,-0.109730811106793,
-0.546118517632758));
#48029=CARTESIAN_POINT('Ctrl Pts',(0.0198156941023548,-0.171904835654138,
-0.538171226324805));
#48030=CARTESIAN_POINT('Ctrl Pts',(0.155259133544419,-0.076410311510098,
-0.530223935016855));
#48031=CARTESIAN_POINT('Ctrl Pts',(0.148301213746763,0.0891666095310972,
-0.522276643708902));
#48032=CARTESIAN_POINT('Ctrl Pts',(0.00532363486478151,0.172961247584135,
-0.514329352400952));
#48033=CARTESIAN_POINT('Ctrl Pts',(-0.142536702432337,0.0981184116960201,
-0.506382061093));
#48034=CARTESIAN_POINT('Ctrl Pts',(-0.159664504357515,-0.0667171664738782,
-0.498434769785048));
#48035=CARTESIAN_POINT('Ctrl Pts',(-0.0303504067061914,-0.170360755653416,
-0.490487478477097));
#48036=CARTESIAN_POINT('Ctrl Pts',(0.126800630838936,-0.117752003264836,
-0.482540187169144));
#48037=CARTESIAN_POINT('Ctrl Pts',(0.167652022935169,0.0428571284593396,
-0.474592895861193));
#48038=CARTESIAN_POINT('Ctrl Pts',(0.0547354826705796,0.164158341825365,
-0.466645604553241));
#48039=CARTESIAN_POINT('Ctrl Pts',(-0.108383625088712,0.134895974983183,
-0.45869831324529));
#48040=CARTESIAN_POINT('Ctrl Pts',(-0.172094890103951,-0.0180909660920301,
-0.450751021937338));
#48041=CARTESIAN_POINT('Ctrl Pts',(-0.0779632913239864,-0.154485143169061,
-0.442803730629387));
#48042=CARTESIAN_POINT('Ctrl Pts',(0.0876750742521607,-0.149187853422831,
-0.434856439321435));
#48043=CARTESIAN_POINT('Ctrl Pts',(0.172899170729097,-0.00705769191907936,
-0.426909148013484));
#48044=CARTESIAN_POINT('Ctrl Pts',(0.0995427292295024,0.141545679240223,
-0.418961856705532));
#48045=CARTESIAN_POINT('Ctrl Pts',(-0.0651128173282645,0.160325466703235,
-0.41101456539758));
#48046=CARTESIAN_POINT('Ctrl Pts',(-0.170047859978802,0.0320571297945394,
-0.403067274089629));
#48047=CARTESIAN_POINT('Ctrl Pts',(-0.119017544302387,-0.125613527942909,
-0.395119982781677));
#48048=CARTESIAN_POINT('Ctrl Pts',(0.0411738860545093,-0.168073333284031,
-0.387172691473725));
#48049=CARTESIAN_POINT('Ctrl Pts',(0.163601242855845,-0.0563787867025962,
-0.379225400165774));
#48050=CARTESIAN_POINT('Ctrl Pts',(0.135975982306233,0.107025541296875,
-0.371278108857821));
#48051=CARTESIAN_POINT('Ctrl Pts',(-0.0163644190684062,0.172267640729731,
-0.363330817549871));
#48052=CARTESIAN_POINT('Ctrl Pts',(-0.153695619597269,0.0795084320726162,
-0.355383526241918));
#48053=CARTESIAN_POINT('Ctrl Pts',(-0.150059492535187,-0.0861747234060912,
-0.347436234933969));
#48054=CARTESIAN_POINT('Ctrl Pts',(-0.0087910393354631,-0.172819709181089,
-0.339488943626015));
#48055=CARTESIAN_POINT('Ctrl Pts',(0.140540423890929,-0.100957037925017,
-0.331541652318065));
#48056=CARTESIAN_POINT('Ctrl Pts',(0.160970308618749,0.0635019212088733,
-0.323594361010112));
#48057=CARTESIAN_POINT('Ctrl Pts',(0.0337606295975726,0.169717866305254,
-0.315647069702161));
#48058=CARTESIAN_POINT('Ctrl Pts',(-0.124413794838165,0.120271118345218,
-0.307699778394209));
#48059=CARTESIAN_POINT('Ctrl Pts',(-0.168477744168953,-0.039486503691345,
-0.299752487086258));
#48060=CARTESIAN_POINT('Ctrl Pts',(-0.0580164219515768,-0.163027694082816,
-0.291805195778306));
#48061=CARTESIAN_POINT('Ctrl Pts',(0.105656696284218,-0.137042317494962,
-0.283857904470355));
#48062=CARTESIAN_POINT('Ctrl Pts',(0.172423070161505,0.0146362266327961,
-0.275910613162403));
#48063=CARTESIAN_POINT('Ctrl Pts',(0.0810455783953381,0.152890642213818,
-0.267963321854451));
#48064=CARTESIAN_POINT('Ctrl Pts',(-0.0846657078511696,0.150916043442814,
-0.2600160305465));
#48065=CARTESIAN_POINT('Ctrl Pts',(-0.172722870928364,0.0105235028277298,
-0.252068739238548));
#48066=CARTESIAN_POINT('Ctrl Pts',(-0.102361195579199,-0.139521037458531,
-0.244121447930597));
#48067=CARTESIAN_POINT('Ctrl Pts',(0.0618846400935952,-0.161598965271126,
-0.236174156622645));
#48068=CARTESIAN_POINT('Ctrl Pts',(0.169370807803051,-0.0354607348225401,
-0.228226865314694));
#48069=CARTESIAN_POINT('Ctrl Pts',(0.121512599367703,0.123201552138589,
-0.220279574006742));
#48070=CARTESIAN_POINT('Ctrl Pts',(-0.0377951510689661,0.168865214959562,
-0.21233228269879));
#48071=CARTESIAN_POINT('Ctrl Pts',(-0.162437753107342,0.0596482236948258,
-0.204384991390838));
#48072=CARTESIAN_POINT('Ctrl Pts',(-0.138094873460796,-0.104277227568877,
-0.196437700082887));
#48073=CARTESIAN_POINT('Ctrl Pts',(0.0129065627974987,-0.172561162992656,
-0.188490408774936));
#48074=CARTESIAN_POINT('Ctrl Pts',(0.152070291491269,-0.0825745753144448,
-0.180543117466984));
#48075=CARTESIAN_POINT('Ctrl Pts',(0.151757420906439,0.0831481785180167,
-0.172595826159032));
#48076=CARTESIAN_POINT('Ctrl Pts',(0.012254906519396,0.172608667222736,
-0.164648534851081));
#48077=CARTESIAN_POINT('Ctrl Pts',(-0.138487619250733,0.103755058131125,
-0.156701243543129));
#48078=CARTESIAN_POINT('Ctrl Pts',(-0.162211379504551,-0.0602611311391257,
-0.148753952235178));
#48079=CARTESIAN_POINT('Ctrl Pts',(-0.0371572630349655,-0.169006729728073,
-0.140806660927225));
#48080=CARTESIAN_POINT('Ctrl Pts',(0.121976899919814,-0.12274184287718,
-0.132859369619274));
#48081=CARTESIAN_POINT('Ctrl Pts',(0.169235748100154,0.0360999609252447,
-0.124912078311322));
#48082=CARTESIAN_POINT('Ctrl Pts',(0.0612739492687115,0.161831550093002,
-0.116964787003371));
#48083=CARTESIAN_POINT('Ctrl Pts',(-0.102887124683252,0.139133409897374,
-0.109017495695419));
#48084=CARTESIAN_POINT('Ctrl Pts',(-0.17268218848071,-0.0111753462307528,
-0.101070204387468));
#48085=CARTESIAN_POINT('Ctrl Pts',(-0.0840947316560137,-0.151235134400324,
-0.093122913079516));
#48086=CARTESIAN_POINT('Ctrl Pts',(0.0816212678773405,-0.152582620718228,
-0.0851756217715646));
#48087=CARTESIAN_POINT('Ctrl Pts',(0.172479045841006,-0.013986821845635,
-0.0772283304636131));
#48088=CARTESIAN_POINT('Ctrl Pts',(0.105134810098645,0.137443586413713,
-0.0692810391556613));
#48089=CARTESIAN_POINT('Ctrl Pts',(-0.0586245811406043,0.162801200529421,
-0.0613337478477097));
#48090=CARTESIAN_POINT('Ctrl Pts',(-0.168638912927327,0.0388619839671219,
-0.0533864565397582));
#48091=CARTESIAN_POINT('Ctrl Pts',(-0.12393356787755,-0.120762648130661,
-0.0454391652318062));
#48092=CARTESIAN_POINT('Ctrl Pts',(0.0343531967590567,-0.16954605151339,
-0.0374918739238549));
#48093=CARTESIAN_POINT('Ctrl Pts',(0.161301394425332,-0.0629771683730991,
-0.0295445826159031));
#48094=CARTESIAN_POINT('Ctrl Pts',(0.139971593454551,0.10165914811014,-0.0215972913079518));
#48095=CARTESIAN_POINT('Ctrl Pts',(0.0406598484393165,0.148790668971504,
-0.0162990971026507));
#48096=CARTESIAN_POINT('Ctrl Pts',(-0.00798678478681935,0.146131905375825,
-0.0136500000000002));
#48097=CARTESIAN_POINT('Ctrl Pts',(-0.129787930238029,0.0433148218226557,
-2.94864852262806));
#48098=CARTESIAN_POINT('Ctrl Pts',(-0.144207233435665,0.000109022081449632,
-2.94599942552541));
#48099=CARTESIAN_POINT('Ctrl Pts',(-0.126253311240158,-0.101084246503596,
-2.94070123132011));
#48100=CARTESIAN_POINT('Ctrl Pts',(0.0169219107275231,-0.161002946168919,
-2.93275394001216));
#48101=CARTESIAN_POINT('Ctrl Pts',(0.14438368807171,-0.0728747486437721,
-2.92480664870421));
#48102=CARTESIAN_POINT('Ctrl Pts',(0.139514764084194,0.0819023268038132,
-2.91685935739625));
#48103=CARTESIAN_POINT('Ctrl Pts',(0.0066351667127898,0.161659351292547,
-2.90891206608831));
#48104=CARTESIAN_POINT('Ctrl Pts',(-0.132303943561717,0.0930925035302517,
-2.90096477478035));
#48105=CARTESIAN_POINT('Ctrl Pts',(-0.149909626174738,-0.0608298430199986,
-2.8930174834724));
#48106=CARTESIAN_POINT('Ctrl Pts',(-0.0300131822609338,-0.158974481534216,
-2.88507019216445));
#48107=CARTESIAN_POINT('Ctrl Pts',(0.11740708193013,-0.111302451803343,
-2.8771229008565));
#48108=CARTESIAN_POINT('Ctrl Pts',(0.157145337254098,0.0384504960783959,
-2.86917560954854));
#48109=CARTESIAN_POINT('Ctrl Pts',(0.0527511745255854,0.152939345598777,
-2.8612283182406));
#48110=CARTESIAN_POINT('Ctrl Pts',(-0.100025018952735,0.127153392495664,
-2.85328102693264));
#48111=CARTESIAN_POINT('Ctrl Pts',(-0.161060052911221,-0.0152551646415358,
-2.8453337356247));
#48112=CARTESIAN_POINT('Ctrl Pts',(-0.0743730558561778,-0.143672222913865,
-2.83738644431673));
#48113=CARTESIAN_POINT('Ctrl Pts',(0.0805277158933123,-0.140315099860671,
-2.8294391530088));
#48114=CARTESIAN_POINT('Ctrl Pts',(0.16156971197941,-0.00826314829488561,
-2.82149186170083));
#48115=CARTESIAN_POINT('Ctrl Pts',(0.0944223578173568,0.131367684903636,
-2.81354457039289));
#48116=CARTESIAN_POINT('Ctrl Pts',(-0.0593277612398802,0.150510014940419,
-2.80559727908493));
#48117=CARTESIAN_POINT('Ctrl Pts',(-0.158663349758915,0.0316068190134606,
-2.79764998777698));
#48118=CARTESIAN_POINT('Ctrl Pts',(-0.112475279434508,-0.116285686053977,
-2.78970269646903));
#48119=CARTESIAN_POINT('Ctrl Pts',(0.0368734361630542,-0.157522692542648,
-2.78175540516108));
#48120=CARTESIAN_POINT('Ctrl Pts',(0.152402387559763,-0.0542822391159111,
-2.77380811385312));
#48121=CARTESIAN_POINT('Ctrl Pts',(0.128150143997042,0.0987450745547089,
-2.76586082254518));
#48122=CARTESIAN_POINT('Ctrl Pts',(-0.0136394980791459,0.161204879614442,
-2.75791353123722));
#48123=CARTESIAN_POINT('Ctrl Pts',(-0.142919196291981,0.0758099761794772,
-2.74996623992927));
#48124=CARTESIAN_POINT('Ctrl Pts',(-0.141115541404577,-0.0791167056924326,
-2.74201894862132));
#48125=CARTESIAN_POINT('Ctrl Pts',(-0.00988281885907166,-0.16147872625534,
-2.73407165731337));
#48126=CARTESIAN_POINT('Ctrl Pts',(0.130414277611373,-0.0957348700431142,
-2.72612436600542));
#48127=CARTESIAN_POINT('Ctrl Pts',(0.151097345755275,0.0578155796543157,
-2.71817707469747));
#48128=CARTESIAN_POINT('Ctrl Pts',(0.0331961842888706,0.158338442879036,
-2.71022978338952));
#48129=CARTESIAN_POINT('Ctrl Pts',(-0.115152021785071,0.113635650322734,
-2.70228249208156));
#48130=CARTESIAN_POINT('Ctrl Pts',(-0.157884512716944,-0.035292064111602,
-2.69433520077361));
#48131=CARTESIAN_POINT('Ctrl Pts',(-0.0558076858302437,-0.151850424258141,
-2.68638790946566));
#48132=CARTESIAN_POINT('Ctrl Pts',(0.0974551172814357,-0.129133842430521,
-2.67844061815771));
#48133=CARTESIAN_POINT('Ctrl Pts',(0.161333541845059,0.0120223716829652,
-2.67049332684976));
#48134=CARTESIAN_POINT('Ctrl Pts',(0.0772392505677555,0.142151845984807,
-2.66254603554181));
#48135=CARTESIAN_POINT('Ctrl Pts',(-0.0776977281342388,0.141901769502529,
-2.65459874423385));
#48136=CARTESIAN_POINT('Ctrl Pts',(-0.161371510632747,0.0115015086517994,
-2.6466514529259));
#48137=CARTESIAN_POINT('Ctrl Pts',(-0.0970377528850418,-0.129447764214701,
-2.63870416161795));
#48138=CARTESIAN_POINT('Ctrl Pts',(0.0562975830174607,-0.151669480422257,
-2.63075687031));
#48139=CARTESIAN_POINT('Ctrl Pts',(0.157997616309539,-0.0347822136395501,
-2.62280957900205));
#48140=CARTESIAN_POINT('Ctrl Pts',(0.114784594855777,0.114006780188545,
-2.6148622876941));
#48141=CARTESIAN_POINT('Ctrl Pts',(-0.0337071432447416,0.158230457369758,
-2.60691499638614));
#48142=CARTESIAN_POINT('Ctrl Pts',(-0.151283192814987,0.0573275214610534,
-2.59896770507819));
#48143=CARTESIAN_POINT('Ctrl Pts',(-0.130104556621024,-0.0961553612213634,
-2.59102041377024));
#48144=CARTESIAN_POINT('Ctrl Pts',(0.0104040364209517,-0.16144598220865,
-2.58307312246229));
#48145=CARTESIAN_POINT('Ctrl Pts',(0.141370202591794,-0.0786607587321608,
-2.57512583115434));
#48146=CARTESIAN_POINT('Ctrl Pts',(0.142673729628386,0.0762709382339727,
-2.56717853984639));
#48147=CARTESIAN_POINT('Ctrl Pts',(0.0131190419946609,0.161248069390943,
-2.55923124853843));
#48148=CARTESIAN_POINT('Ctrl Pts',(-0.128468235086874,0.0983308787656647,
-2.55128395723048));
#48149=CARTESIAN_POINT('Ctrl Pts',(-0.152226365000939,-0.0547739257655036,
-2.54333666592253));
#48150=CARTESIAN_POINT('Ctrl Pts',(-0.0363647457035736,-0.157640903369266,
-2.53538937461458));
#48151=CARTESIAN_POINT('Ctrl Pts',(0.112850075420815,-0.115921998010216,
-2.52744208330662));
#48152=CARTESIAN_POINT('Ctrl Pts',(0.158560492241468,0.0321188331872045,
-2.51949479199867));
#48153=CARTESIAN_POINT('Ctrl Pts',(0.0588415929153526,0.150700750125366,
-2.51154750069073));
#48154=CARTESIAN_POINT('Ctrl Pts',(-0.094845936916996,0.131062189038263,
-2.50360020938277));
#48155=CARTESIAN_POINT('Ctrl Pts',(-0.161542189476235,-0.00878465505231707,
-2.49565291807482));
#48156=CARTESIAN_POINT('Ctrl Pts',(-0.0800743577022627,-0.140574344685416,
-2.48770562676687));
#48157=CARTESIAN_POINT('Ctrl Pts',(0.0748364794314408,-0.14343134417369,
-2.47975833545891));
#48158=CARTESIAN_POINT('Ctrl Pts',(0.161108414952932,-0.0147352562420184,
-2.47181104415097));
#48159=CARTESIAN_POINT('Ctrl Pts',(0.0996141176576514,0.127475788714766,
-2.46386375284301));
#48160=CARTESIAN_POINT('Ctrl Pts',(-0.0532447610962578,0.152767943499173,
-2.45591646153507));
#48161=CARTESIAN_POINT('Ctrl Pts',(-0.157268339926687,0.0379436213594348,
-2.44796917022711));
#48162=CARTESIAN_POINT('Ctrl Pts',(-0.117047745421395,-0.111682023785981,
-2.44002187891916));
#48163=CARTESIAN_POINT('Ctrl Pts',(0.0305272936401855,-0.158874584147906,
-2.43207458761121));
#48164=CARTESIAN_POINT('Ctrl Pts',(0.150103154753057,-0.0603497479559275,
-2.42412729630326));
#48165=CARTESIAN_POINT('Ctrl Pts',(0.132006643393938,0.0935269760284694,
-2.4161800049953));
#48166=CARTESIAN_POINT('Ctrl Pts',(-0.00716439040280769,0.161622153974386,
-2.40823271368735));
#48167=CARTESIAN_POINT('Ctrl Pts',(-0.139764352287754,0.0814799053432716,
-2.4002854223794));
#48168=CARTESIAN_POINT('Ctrl Pts',(-0.144174536961678,-0.0733944959588244,
-2.39233813107145));
#48169=CARTESIAN_POINT('Ctrl Pts',(-0.0163499888865172,-0.160952561360715,
-2.3843908397635));
#48170=CARTESIAN_POINT('Ctrl Pts',(0.126470524887037,-0.100887340533693,
-2.37644354845554));
#48171=CARTESIAN_POINT('Ctrl Pts',(0.153294161462234,0.0517102427644136,
-2.3684962571476));
#48172=CARTESIAN_POINT('Ctrl Pts',(0.0395186818540962,0.156879963442368,
-2.36054896583964));
#48173=CARTESIAN_POINT('Ctrl Pts',(-0.110502742729481,0.118161723897488,
-2.35260167453169));
#48174=CARTESIAN_POINT('Ctrl Pts',(-0.159172701507709,-0.0289326846300512,
-2.34465438322374));
#48175=CARTESIAN_POINT('Ctrl Pts',(-0.0618518349405682,-0.149490466785172,
-2.33670709191578));
#48176=CARTESIAN_POINT('Ctrl Pts',(0.0921986111748694,-0.132937824724904,
-2.32875980060784));
#48177=CARTESIAN_POINT('Ctrl Pts',(0.16168586766282,0.00554340538704512,
-2.32081250929988));
#48178=CARTESIAN_POINT('Ctrl Pts',(0.0828772603299642,0.138940306842052,
-2.31286521799194));
#48179=CARTESIAN_POINT('Ctrl Pts',(-0.0719451328049027,0.144903233265683,
-2.30491792668398));
#48180=CARTESIAN_POINT('Ctrl Pts',(-0.160780524285084,0.0179630775697664,
-2.29697063537603));
#48181=CARTESIAN_POINT('Ctrl Pts',(-0.102150419373578,-0.125452544681112,
-2.28902334406807));
#48182=CARTESIAN_POINT('Ctrl Pts',(0.0501705250629579,-0.153804965979877,
-2.28107605276013));
#48183=CARTESIAN_POINT('Ctrl Pts',(0.15647581296685,-0.0410897688181301,
-2.27312876145218));
#48184=CARTESIAN_POINT('Ctrl Pts',(0.119263821430011,0.109312350825853,
-2.26518147014422));
#48185=CARTESIAN_POINT('Ctrl Pts',(-0.027335166491799,0.159454814345725,
-2.25723417883627));
#48186=CARTESIAN_POINT('Ctrl Pts',(-0.148862747826359,0.0633477028371972,
-2.24928688752832));
#48187=CARTESIAN_POINT('Ctrl Pts',(-0.133855639402594,-0.0908609759208357,
-2.24133959622037));
#48188=CARTESIAN_POINT('Ctrl Pts',(0.00392186299208866,-0.161733324135243,
-2.23339230491242));
#48189=CARTESIAN_POINT('Ctrl Pts',(0.138102291204558,-0.0842662821608703,
-2.22544501360447));
#48190=CARTESIAN_POINT('Ctrl Pts',(0.145617359816636,0.0704885357004696,
-2.21749772229651));
#48191=CARTESIAN_POINT('Ctrl Pts',(0.0195743600986712,0.16059232102405,
-2.20955043098856));
#48192=CARTESIAN_POINT('Ctrl Pts',(-0.124421950453024,0.103403227177053,
-2.20160313968061));
#48193=CARTESIAN_POINT('Ctrl Pts',(-0.154300305691649,-0.0486257628076713,
-2.19365584837266));
#48194=CARTESIAN_POINT('Ctrl Pts',(-0.042656724281636,-0.156055929136719,
-2.18570855706471));
#48195=CARTESIAN_POINT('Ctrl Pts',(0.108110967766809,-0.12035392720509,
-2.17776126575676));
#48196=CARTESIAN_POINT('Ctrl Pts',(0.15972089429603,0.0257348998529341,
-2.1698139744488));
#48197=CARTESIAN_POINT('Ctrl Pts',(0.0648372012390534,0.148220060992602,
-2.16186668314085));
#48198=CARTESIAN_POINT('Ctrl Pts',(-0.089514204763127,0.134759995142434,
-2.1539193918329));
#48199=CARTESIAN_POINT('Ctrl Pts',(-0.161764518619993,-0.00229992626103489,
-2.14597210052495));
#48200=CARTESIAN_POINT('Ctrl Pts',(-0.0856468311724065,-0.137250389636203,
-2.138024809217));
#48201=CARTESIAN_POINT('Ctrl Pts',(0.0690248511036805,-0.146316844810428,
-2.13007751790905));
#48202=CARTESIAN_POINT('Ctrl Pts',(0.160387970501104,-0.0211836744617428,
-2.1221302266011));
#48203=CARTESIAN_POINT('Ctrl Pts',(0.104645637976606,0.123378845827124,
-2.11418293529314));
#48204=CARTESIAN_POINT('Ctrl Pts',(-0.0470761113215489,0.154780130792054,
-2.10623564398519));
#48205=CARTESIAN_POINT('Ctrl Pts',(-0.155620354170519,0.0442193906901315,
-2.09828835267724));
#48206=CARTESIAN_POINT('Ctrl Pts',(-0.121431931614596,-0.106898714349201,
-2.09034106136929));
#48207=CARTESIAN_POINT('Ctrl Pts',(0.0241320456173179,-0.159970914604774,
-2.08239377006134));
#48208=CARTESIAN_POINT('Ctrl Pts',(0.147562470904876,-0.066320180379818,
-2.07444647875339));
#48209=CARTESIAN_POINT('Ctrl Pts',(0.135650801013122,0.0881584331171016,
-2.06649918744543));
#48210=CARTESIAN_POINT('Ctrl Pts',(-0.000677758276635096,0.161779447980522,
-2.05855189613748));
#48211=CARTESIAN_POINT('Ctrl Pts',(-0.136384687794117,0.0870187685529117,
-2.05060460482953));
#48212=CARTESIAN_POINT('Ctrl Pts',(-0.147001617915132,-0.067554226185322,
-2.04265731352158));
#48213=CARTESIAN_POINT('Ctrl Pts',(-0.0227908588453908,-0.160167493263313,
-2.03471002221363));
#48214=CARTESIAN_POINT('Ctrl Pts',(0.122323335685659,-0.10587752685012,
-2.02676273090567));
#48215=CARTESIAN_POINT('Ctrl Pts',(0.155244393035563,0.0455217264191934,
-2.01881543959773));
#48216=CARTESIAN_POINT('Ctrl Pts',(0.0457776109203872,0.15516913186451,
-2.01086814828977));
#48217=CARTESIAN_POINT('Ctrl Pts',(-0.105675712462875,0.122497726267175,
-2.00292085698182));
#48218=CARTESIAN_POINT('Ctrl Pts',(-0.160204850132875,-0.0225267649489869,
-1.99497356567387));
#48219=CARTESIAN_POINT('Ctrl Pts',(-0.0677964911486736,-0.146890043682654,
-1.98702627436592));
#48220=CARTESIAN_POINT('Ctrl Pts',(0.0867937973030992,-0.136527967445768,
-1.97907898305797));
#48221=CARTESIAN_POINT('Ctrl Pts',(0.161778110715712,-0.0009444778551103,
-1.97113169175001));
#48222=CARTESIAN_POINT('Ctrl Pts',(0.0883819563566127,0.135505272723026,
-1.96318440044206));
#48223=CARTESIAN_POINT('Ctrl Pts',(-0.0660768088140216,0.147671610278073,
-1.95523710913411));
#48224=CARTESIAN_POINT('Ctrl Pts',(-0.15993091147926,0.024395751650182,
-1.94728981782616));
#48225=CARTESIAN_POINT('Ctrl Pts',(-0.107098769933436,-0.12125552615823,
-1.93934252651821));
#48226=CARTESIAN_POINT('Ctrl Pts',(0.043962764391142,-0.155693045741462,
-1.93139523521026));
#48227=CARTESIAN_POINT('Ctrl Pts',(0.154702307588264,-0.0473312282962324,
-1.92344794390231));
#48228=CARTESIAN_POINT('Ctrl Pts',(0.123551203999137,0.10444208507842,-1.91550065259435));
#48229=CARTESIAN_POINT('Ctrl Pts',(-0.0209192192559613,0.160422677358549,
-1.9075533612864));
#48230=CARTESIAN_POINT('Ctrl Pts',(-0.146202846937255,0.0692659851052862,
-1.89960606997845));
#48231=CARTESIAN_POINT('Ctrl Pts',(-0.137391406242903,-0.0854204345327365,
-1.8916587786705));
#48232=CARTESIAN_POINT('Ctrl Pts',(-0.00256661902134908,-0.161760506960022,
-1.88371148736255));
#48233=CARTESIAN_POINT('Ctrl Pts',(0.134612232846497,-0.0897362575174868,
-1.87576419605459));
#48234=CARTESIAN_POINT('Ctrl Pts',(0.148326754532756,0.0645927475413762,
-1.86781690474665));
#48235=CARTESIAN_POINT('Ctrl Pts',(0.0259981915071029,0.159678248936804,
-1.85986961343869));
#48236=CARTESIAN_POINT('Ctrl Pts',(-0.120175524611116,0.108309244432814,
-1.85192232213074));
#48237=CARTESIAN_POINT('Ctrl Pts',(-0.15612604379855,-0.0423993819881522,
-1.84397503082279));
#48238=CARTESIAN_POINT('Ctrl Pts',(-0.0488800866043013,-0.154219928280103,
-1.83602773951484));
#48239=CARTESIAN_POINT('Ctrl Pts',(0.103197956234794,-0.124592258885236,
-1.82808044820689));
#48240=CARTESIAN_POINT('Ctrl Pts',(0.160624374379668,0.0193095701739912,
-1.82013315689893));
#48241=CARTESIAN_POINT('Ctrl Pts',(0.070728514494755,0.145500949765042,
-1.81218586559098));
#48242=CARTESIAN_POINT('Ctrl Pts',(-0.084038482895108,0.13824103058735,
-1.80423857428303));
#48243=CARTESIAN_POINT('Ctrl Pts',(-0.161726638483477,0.00418850211877394,
-1.79629128297508));
#48244=CARTESIAN_POINT('Ctrl Pts',(-0.0910815358630474,-0.133705657958041,
-1.78834399166713));
#48245=CARTESIAN_POINT('Ctrl Pts',(0.063102191587005,-0.14896698480563,
-1.78039670035917));
#48246=CARTESIAN_POINT('Ctrl Pts',(0.1594095310407,-0.0275980172937854,
-1.77244940905123));
#48247=CARTESIAN_POINT('Ctrl Pts',(0.109508828637277,0.119083439636481,
-1.76450211774327));
#48248=CARTESIAN_POINT('Ctrl Pts',(-0.0408317364054441,0.15654334366967,
-1.75655482643532));
#48249=CARTESIAN_POINT('Ctrl Pts',(-0.153722042442376,0.0504240301097478,
-1.74860753512737));
#48250=CARTESIAN_POINT('Ctrl Pts',(-0.125620786249326,-0.101943451026858,
-1.74066024381942));
#48251=CARTESIAN_POINT('Ctrl Pts',(0.0176979795503254,-0.160809920915969,
-1.73271295251147));
#48252=CARTESIAN_POINT('Ctrl Pts',(0.144784422740484,-0.0721839322624418,
-1.72476566120351));
#48253=CARTESIAN_POINT('Ctrl Pts',(0.139076755050945,0.0826480813429048,
-1.71681836989556));
#48254=CARTESIAN_POINT('Ctrl Pts',(0.00580996407003145,0.161676508691489,
-1.70887107858761));
#48255=CARTESIAN_POINT('Ctrl Pts',(-0.132785639212092,0.0924176561280391,
-1.70092378727966));
#48256=CARTESIAN_POINT('Ctrl Pts',(-0.149592236722726,-0.0616052908235646,
-1.69297649597171));
#48257=CARTESIAN_POINT('Ctrl Pts',(-0.0291950681506911,-0.159124784810037,
-1.68502920466376));
#48258=CARTESIAN_POINT('Ctrl Pts',(0.117979381041458,-0.110697401930842,
-1.67708191335581));
#48259=CARTESIAN_POINT('Ctrl Pts',(0.156944903396088,0.0392599852668939,
-1.66913462204785));
#48260=CARTESIAN_POINT('Ctrl Pts',(0.0519629035718947,0.153208700136586,
-1.6611873307399));
#48261=CARTESIAN_POINT('Ctrl Pts',(-0.1006786955928,0.126636682674872,-1.65324003943195));
#48262=CARTESIAN_POINT('Ctrl Pts',(-0.16097929831109,-0.016084609427433,
-1.645292748124));
#48263=CARTESIAN_POINT('Ctrl Pts',(-0.0736320920687726,-0.144053337909053,
-1.63734545681605));
#48264=CARTESIAN_POINT('Ctrl Pts',(0.0812493696784421,-0.139898495603134,
-1.6293981655081));
#48265=CARTESIAN_POINT('Ctrl Pts',(0.161610122624517,-0.00743084184010702,
-1.62145087420014));
#48266=CARTESIAN_POINT('Ctrl Pts',(0.0937444839680286,0.131852269114839,
-1.61350358289219));
#48267=CARTESIAN_POINT('Ctrl Pts',(-0.0601021957616684,0.150202447416113,
-1.60555629158424));
#48268=CARTESIAN_POINT('Ctrl Pts',(-0.158824038875523,0.0307891834972998,
-1.59760900027629));
#48269=CARTESIAN_POINT('Ctrl Pts',(-0.111874844804655,-0.116863459837105,
-1.58966170896834));
#48270=CARTESIAN_POINT('Ctrl Pts',(0.0376842866091804,-0.157330682601715,
-1.58171441766039));
#48271=CARTESIAN_POINT('Ctrl Pts',(0.152679952978355,-0.0534965522598539,
-1.57376712635243));
#48272=CARTESIAN_POINT('Ctrl Pts',(0.127639846015364,0.0994038171014477,
-1.56581983504448));
#48273=CARTESIAN_POINT('Ctrl Pts',(-0.0144696220267058,0.161132489534446,
-1.55787254373653));
#48274=CARTESIAN_POINT('Ctrl Pts',(-0.143307768779982,0.0750728483039466,
-1.54992525242858));
#48275=CARTESIAN_POINT('Ctrl Pts',(-0.140706169619418,-0.0798424885395985,
-1.54197796112063));
#48276=CARTESIAN_POINT('Ctrl Pts',(-0.00905097245273122,-0.161527486957557,
-1.53403066981268));
#48277=CARTESIAN_POINT('Ctrl Pts',(0.130905641514927,-0.095061885972925,
-1.52608337850473));
#48278=CARTESIAN_POINT('Ctrl Pts',(0.15079755553023,0.0585930575347549,
-1.51813608719677));
#48279=CARTESIAN_POINT('Ctrl Pts',(0.0323802030482504,0.158507323476609,
-1.51018879588882));
#48280=CARTESIAN_POINT('Ctrl Pts',(-0.115735788227241,0.113041038869003,
-1.50224150458087));
#48281=CARTESIAN_POINT('Ctrl Pts',(-0.15770064249716,-0.0361047988658983,
-1.49429421327292));
#48282=CARTESIAN_POINT('Ctrl Pts',(-0.0550248219680774,-0.152135854132237,
-1.48634692196497));
#48283=CARTESIAN_POINT('Ctrl Pts',(0.0981189437394838,-0.128630175404576,
-1.47839963065702));
#48284=CARTESIAN_POINT('Ctrl Pts',(0.161269479182942,0.0128531797321523,
-1.47045233934906));
#48285=CARTESIAN_POINT('Ctrl Pts',(0.0765060561025797,0.142547790318873,
-1.46250504804111));
#48286=CARTESIAN_POINT('Ctrl Pts',(-0.0784275793856785,0.141499695889663,
-1.45455775673316));
#48287=CARTESIAN_POINT('Ctrl Pts',(-0.161428609999475,0.0106701930067575,
-1.44661046542521));
#48288=CARTESIAN_POINT('Ctrl Pts',(-0.0963697296803828,-0.129945851594016,
-1.43866317411726));
#48289=CARTESIAN_POINT('Ctrl Pts',(0.057078027883893,-0.151377501228055,
-1.43071588280931));
#48290=CARTESIAN_POINT('Ctrl Pts',(0.158174670458443,-0.0339679668294594,
-1.42276859150135));
#48291=CARTESIAN_POINT('Ctrl Pts',(0.114195866865224,0.114596479597168,
-1.4148213001934));
#48292=CARTESIAN_POINT('Ctrl Pts',(-0.0345216808516293,0.158054745883641,
-1.40687400888545));
#48293=CARTESIAN_POINT('Ctrl Pts',(-0.151576458306368,0.056547559031861,
-1.3989267175775));
#48294=CARTESIAN_POINT('Ctrl Pts',(-0.129607571266712,-0.0968242046985573,
-1.39097942626955));
#48295=CARTESIAN_POINT('Ctrl Pts',(0.0112354450740637,-0.16139025348252,
-1.3830321349616));
#48296=CARTESIAN_POINT('Ctrl Pts',(0.141773478940156,-0.0779315713582716,
-1.37508484365364));
#48297=CARTESIAN_POINT('Ctrl Pts',(0.142278994626267,0.07700478448319,-1.36713755234569));
#48298=CARTESIAN_POINT('Ctrl Pts',(0.0122883406925415,0.161313501692165,
-1.35919026103774));
#48299=CARTESIAN_POINT('Ctrl Pts',(-0.128972995857213,0.0976678835891277,
-1.35124296972979));
#48300=CARTESIAN_POINT('Ctrl Pts',(-0.151942226197115,-0.0555572591425189,
-1.34329567842184));
#48301=CARTESIAN_POINT('Ctrl Pts',(-0.0355523151942074,-0.157826113268673,
-1.33534838711389));
#48302=CARTESIAN_POINT('Ctrl Pts',(0.113445648502268,-0.115339212677492,
-1.32740109580593));
#48303=CARTESIAN_POINT('Ctrl Pts',(0.158392957156713,0.0329350917459731,
-1.31945380449798));
#48304=CARTESIAN_POINT('Ctrl Pts',(0.0580646103427997,0.151001821746967,
-1.31150651319003));
#48305=CARTESIAN_POINT('Ctrl Pts',(-0.0955197301622941,0.13057193532642,
-1.30355922188208));
#48306=CARTESIAN_POINT('Ctrl Pts',(-0.161494800289547,-0.0096165807126814,
-1.29561193057413));
#48307=CARTESIAN_POINT('Ctrl Pts',(-0.0793492507380876,-0.140984912499416,
-1.28766463926618));
#48308=CARTESIAN_POINT('Ctrl Pts',(0.0755742468915394,-0.143043987472178,
-1.27971734795822));
#48309=CARTESIAN_POINT('Ctrl Pts',(0.161182173609555,-0.0139052528083161,
-1.27177005665028));
#48310=CARTESIAN_POINT('Ctrl Pts',(0.0989562171721762,0.127987172123371,
-1.26382276534232));
#48311=CARTESIAN_POINT('Ctrl Pts',(-0.0540309042211304,0.152491673655355,
-1.25587547403437));
#48312=CARTESIAN_POINT('Ctrl Pts',(-0.157461686954082,0.037133088839183,
-1.24792818272642));
#48313=CARTESIAN_POINT('Ctrl Pts',(-0.116470961344493,-0.112283410656488,
-1.23998089141847));
#48314=CARTESIAN_POINT('Ctrl Pts',(0.0313451910775401,-0.158715242309856,
-1.23203360011052));
#48315=CARTESIAN_POINT('Ctrl Pts',(0.150412002232682,-0.0595758233641786,
-1.22408630880256));
#48316=CARTESIAN_POINT('Ctrl Pts',(0.13152317061867,0.0942056512932029,
-1.21613901749462));
#48317=CARTESIAN_POINT('Ctrl Pts',(-0.00799674942183057,0.161583109092035,
-1.20819172618666));
#48318=CARTESIAN_POINT('Ctrl Pts',(-0.140182170285556,0.0807589516969816,
-1.20024443487871));
#48319=CARTESIAN_POINT('Ctrl Pts',(-0.143794597508774,-0.0741361104486446,
-1.19229714357076));
#48320=CARTESIAN_POINT('Ctrl Pts',(-0.0155207667765463,-0.161034638956444,
-1.18434985226281));
#48321=CARTESIAN_POINT('Ctrl Pts',(0.126988479515248,-0.10023460088996,
-1.17640256095485));
#48322=CARTESIAN_POINT('Ctrl Pts',(0.153025788356846,0.0524991165918986,
-1.1684552696469));
#48323=CARTESIAN_POINT('Ctrl Pts',(0.0387101288205123,0.157081428157065,
-1.16050797833895));
#48324=CARTESIAN_POINT('Ctrl Pts',(-0.111109882920702,0.117590999070983,
-1.152560687031));
#48325=CARTESIAN_POINT('Ctrl Pts',(-0.159021568937894,-0.029752138707914,
-1.14461339572305));
#48326=CARTESIAN_POINT('Ctrl Pts',(-0.0610810461463133,-0.149807059068777,
-1.1366661044151));
#48327=CARTESIAN_POINT('Ctrl Pts',(0.092882100219491,-0.132461181498507,
-1.12871881310715));
#48328=CARTESIAN_POINT('Ctrl Pts',(0.161655171010697,0.0063761140725619,
-1.12077152179919));
#48329=CARTESIAN_POINT('Ctrl Pts',(0.0821605324921188,0.139365333012824,
-1.11282423049124));
#48330=CARTESIAN_POINT('Ctrl Pts',(-0.0726905197564767,0.1445307492636,
-1.10487693918329));
#48331=CARTESIAN_POINT('Ctrl Pts',(-0.160870912567167,0.0171347201602809,
-1.09692964787534));
#48332=CARTESIAN_POINT('Ctrl Pts',(-0.101502906203354,-0.125977018449545,
-1.08898235656739));
#48333=CARTESIAN_POINT('Ctrl Pts',(0.0509620502732468,-0.153544516597341,
-1.08103506525943));
#48334=CARTESIAN_POINT('Ctrl Pts',(0.156685375111944,-0.0402832765697306,
-1.07308777395149));
#48335=CARTESIAN_POINT('Ctrl Pts',(0.118699213239233,0.10992518329096,-1.06514048264353));
#48336=CARTESIAN_POINT('Ctrl Pts',(-0.0281560948155716,0.159311906240246,
-1.05719319133558));
#48337=CARTESIAN_POINT('Ctrl Pts',(-0.149187053081172,0.0625801273418309,
-1.04924590002763));
#48338=CARTESIAN_POINT('Ctrl Pts',(-0.133385873650668,-0.0915492100217792,
-1.04129860871968));
#48339=CARTESIAN_POINT('Ctrl Pts',(0.00475483761677099,-0.161710978799839,
-1.03335131741172));
#48340=CARTESIAN_POINT('Ctrl Pts',(0.138534482812702,-0.0835538521971371,
-1.02540402610378));
#48341=CARTESIAN_POINT('Ctrl Pts',(0.145252368717955,0.0712376201665093,
-1.01745673479582));
#48342=CARTESIAN_POINT('Ctrl Pts',(0.0187469506794855,0.160691010904112,
-1.00950944348787));
#48343=CARTESIAN_POINT('Ctrl Pts',(-0.124952890626809,0.102761005586597,
-1.00156215217992));
#48344=CARTESIAN_POINT('Ctrl Pts',(-0.154047806219669,-0.0494198598143619,
-0.993614860871969));
#48345=CARTESIAN_POINT('Ctrl Pts',(-0.0418523739097306,-0.156273567641121,
-0.985667569564015));
#48346=CARTESIAN_POINT('Ctrl Pts',(0.108729430886627,-0.11979549242035,
-0.977720278256066));
#48347=CARTESIAN_POINT('Ctrl Pts',(0.159586225024031,0.0265572198797849,
-0.969772986948112));
#48348=CARTESIAN_POINT('Ctrl Pts',(0.0640729162208801,0.148552046610325,
-0.961825695640163));
#48349=CARTESIAN_POINT('Ctrl Pts',(-0.0902071147197211,0.134297154099061,
-0.95387840433221));
#48350=CARTESIAN_POINT('Ctrl Pts',(-0.161750526848092,-0.00313308307082268,
-0.945931113024258));
#48351=CARTESIAN_POINT('Ctrl Pts',(-0.0849387707162987,-0.137689703225653,
-0.937983821716307));
#48352=CARTESIAN_POINT('Ctrl Pts',(0.069777557765129,-0.145959383314327,
-0.930036530408354));
#48353=CARTESIAN_POINT('Ctrl Pts',(0.160494952056057,-0.0203572962273449,
-0.922089239100404));
#48354=CARTESIAN_POINT('Ctrl Pts',(0.104008772540114,0.123916199021204,
-0.914141947792451));
#48355=CARTESIAN_POINT('Ctrl Pts',(-0.0478727002796515,0.154535606618988,
-0.906194656484501));
#48356=CARTESIAN_POINT('Ctrl Pts',(-0.15584604715108,0.0434172630706667,
-0.898247365176548));
#48357=CARTESIAN_POINT('Ctrl Pts',(-0.120879726385485,-0.107522745938403,
-0.890300073868598));
#48358=CARTESIAN_POINT('Ctrl Pts',(0.024955674664485,-0.159844497707004,
-0.882352782560644));
#48359=CARTESIAN_POINT('Ctrl Pts',(0.147902103504972,-0.0655592626862832,
-0.874405491252694));
#48360=CARTESIAN_POINT('Ctrl Pts',(0.135194931216111,0.0888559492585357,
-0.866458199944742));
#48361=CARTESIAN_POINT('Ctrl Pts',(-0.00151101349915643,0.161773811178971,
-0.85851090863679));
#48362=CARTESIAN_POINT('Ctrl Pts',(-0.136831079192702,0.0863151487985995,
-0.85056361732884));
#48363=CARTESIAN_POINT('Ctrl Pts',(-0.146651721963705,-0.0683104793589116,
-0.842616326020886));
#48364=CARTESIAN_POINT('Ctrl Pts',(-0.0219655948865895,-0.160282755736362,
-0.834669034712937));
#48365=CARTESIAN_POINT('Ctrl Pts',(0.122867047870162,-0.105246081603238,
-0.826721743404984));
#48366=CARTESIAN_POINT('Ctrl Pts',(0.155007868747866,0.0463207272331561,
-0.818774452097032));
#48367=CARTESIAN_POINT('Ctrl Pts',(0.0449777867058173,0.155402856628216,
-0.810827160789081));
#48368=CARTESIAN_POINT('Ctrl Pts',(-0.106305249776236,0.121951806116908,
-0.802879869481129));
#48369=CARTESIAN_POINT('Ctrl Pts',(-0.160086698320322,-0.0233516202020928,
-0.794932578173178));
#48370=CARTESIAN_POINT('Ctrl Pts',(-0.0670390172886451,-0.14723728911569,
-0.786985286865226));
#48371=CARTESIAN_POINT('Ctrl Pts',(0.0874958494954061,-0.136079114731987,
-0.779037995557275));
#48372=CARTESIAN_POINT('Ctrl Pts',(0.16178082945128,-0.000111208002141897,
-0.771090704249321));
#48373=CARTESIAN_POINT('Ctrl Pts',(0.0876828480517711,0.135958697046912,
-0.763143412941372));
#48374=CARTESIAN_POINT('Ctrl Pts',(-0.066836532459887,0.147329315052716,
-0.755196121633419));
#48375=CARTESIAN_POINT('Ctrl Pts',(-0.160054443280973,0.0235716849457503,
-0.747248830325469));
#48376=CARTESIAN_POINT('Ctrl Pts',(-0.106472808366821,-0.121805542663896,
-0.739301539017515));
#48377=CARTESIAN_POINT('Ctrl Pts',(0.044764096722905,-0.155464545121215,
-0.731354247709567));
#48378=CARTESIAN_POINT('Ctrl Pts',(0.154944040634522,-0.0465337879074077,
-0.723406956401613));
#48379=CARTESIAN_POINT('Ctrl Pts',(0.12301162381898,0.105077064817125,-0.715459665093662));
#48380=CARTESIAN_POINT('Ctrl Pts',(-0.0217452177773267,0.160312802511157,
-0.70751237378571));
#48381=CARTESIAN_POINT('Ctrl Pts',(-0.146557670288339,0.0685120312413697,
-0.699565082477759));
#48382=CARTESIAN_POINT('Ctrl Pts',(-0.136949615743669,-0.0861269521858602,
-0.691617791169806));
#48383=CARTESIAN_POINT('Ctrl Pts',(-0.00173341832168038,-0.161771580959345,
-0.683670499861855));
#48384=CARTESIAN_POINT('Ctrl Pts',(0.135072644504701,-0.0890417309561679,
-0.675723208553904));
#48385=CARTESIAN_POINT('Ctrl Pts',(0.147992094450622,0.0653558652707012,
-0.667775917245952));
#48386=CARTESIAN_POINT('Ctrl Pts',(0.0251754049154316,0.159810037646288,
-0.659828625938));
#48387=CARTESIAN_POINT('Ctrl Pts',(-0.1207317901348,0.107688829485749,-0.65188133463005));
#48388=CARTESIAN_POINT('Ctrl Pts',(-0.155905589821069,-0.0432029652652273,
-0.643934043322096));
#48389=CARTESIAN_POINT('Ctrl Pts',(-0.0480851102223821,-0.154469645303101,
-0.635986752014146));
#48390=CARTESIAN_POINT('Ctrl Pts',(0.1038383145528,-0.124059072928981,-0.628039460706194));
#48391=CARTESIAN_POINT('Ctrl Pts',(0.160522787545149,0.0201366289109875,
-0.620092169398242));
#48392=CARTESIAN_POINT('Ctrl Pts',(0.0699781564356221,0.145863315357343,
-0.612144878090291));
#48393=CARTESIAN_POINT('Ctrl Pts',(-0.0847493949700018,0.137806346723881,
-0.604197586782338));
#48394=CARTESIAN_POINT('Ctrl Pts',(-0.161746066633085,0.00335545434920126,
-0.596250295474388));
#48395=CARTESIAN_POINT('Ctrl Pts',(-0.0903916608786185,-0.13417301065702,
-0.588303004166436));
#48396=CARTESIAN_POINT('Ctrl Pts',(0.0638686266697115,-0.148639993516177,
-0.580355712858485));
#48397=CARTESIAN_POINT('Ctrl Pts',(0.159549563406843,-0.026776593544546,
-0.572408421550533));
#48398=CARTESIAN_POINT('Ctrl Pts',(0.108894022691339,0.11964589824671,-0.564461130242582));
#48399=CARTESIAN_POINT('Ctrl Pts',(-0.0416374898290139,0.156330958501196,
-0.556513838934629));
#48400=CARTESIAN_POINT('Ctrl Pts',(-0.153979718333526,0.0496315976681452,
-0.548566547626678));
#48401=CARTESIAN_POINT('Ctrl Pts',(-0.125094048127839,-0.102589123537314,
-0.540619256318726));
#48402=CARTESIAN_POINT('Ctrl Pts',(0.01852601534372,-0.160716632308695,
-0.532671965010776));
#48403=CARTESIAN_POINT('Ctrl Pts',(0.145154294138808,-0.0714372454552122,
-0.524724673702822));
#48404=CARTESIAN_POINT('Ctrl Pts',(0.138649221529904,0.0833633163586695,
-0.516777382394872));
#48405=CARTESIAN_POINT('Ctrl Pts',(0.00497715299197124,0.161704289037918,
-0.50883009108692));
#48406=CARTESIAN_POINT('Ctrl Pts',(-0.133259885960394,0.0917325020861564,
-0.500882799778969));
#48407=CARTESIAN_POINT('Ctrl Pts',(-0.149272947104322,-0.0623749661960178,
-0.492935508471017));
#48408=CARTESIAN_POINT('Ctrl Pts',(-0.0283750898365281,-0.159273046752842,
-0.484988217163066));
#48409=CARTESIAN_POINT('Ctrl Pts',(0.118547976184055,-0.110088266803636,
-0.477040925855113));
#48410=CARTESIAN_POINT('Ctrl Pts',(0.15674060839156,0.0400678278199378,
-0.469093634547163));
#48411=CARTESIAN_POINT('Ctrl Pts',(0.0511730947482288,0.153474308987053,
-0.46114634323921));
#48412=CARTESIAN_POINT('Ctrl Pts',(-0.101329617374527,0.126116445350699,
-0.453199051931259));
#48413=CARTESIAN_POINT('Ctrl Pts',(-0.160894317311058,-0.0169135390197523,
-0.445251760623307));
#48414=CARTESIAN_POINT('Ctrl Pts',(-0.0728891515914287,-0.144430677923514,
-0.437304469315356));
#48415=CARTESIAN_POINT('Ctrl Pts',(0.0819688557195135,-0.139478155412228,
-0.429357178007404));
#48416=CARTESIAN_POINT('Ctrl Pts',(0.161646252374504,-0.00659835119118075,
-0.421409886699452));
#48417=CARTESIAN_POINT('Ctrl Pts',(0.0930641197596701,0.132333362227829,
-0.413462595391501));
#48418=CARTESIAN_POINT('Ctrl Pts',(-0.0608750340344286,0.149890891572741,
-0.405515304083549));
#48419=CARTESIAN_POINT('Ctrl Pts',(-0.158980515487525,0.0299707330655217,
-0.397568012775598));
#48420=CARTESIAN_POINT('Ctrl Pts',(-0.111271441743595,-0.117438134340879,
-0.389620721467646));
#48421=CARTESIAN_POINT('Ctrl Pts',(0.0384941370646189,-0.157134498302616,
-0.381673430159694));
#48422=CARTESIAN_POINT('Ctrl Pts',(0.152953468081658,-0.0527094464679463,
-0.373726138851743));
#48423=CARTESIAN_POINT('Ctrl Pts',(0.127126161797411,0.100059922705459,
-0.365778847543791));
#48424=CARTESIAN_POINT('Ctrl Pts',(-0.0152993620706074,0.161055824686338,
-0.35783155623584));
#48425=CARTESIAN_POINT('Ctrl Pts',(-0.143692539469735,0.0743337288577851,
-0.349884264927888));
#48426=CARTESIAN_POINT('Ctrl Pts',(-0.140293065023078,-0.0805661532629814,
-0.341936973619937));
#48427=CARTESIAN_POINT('Ctrl Pts',(-0.00821888593833973,-0.161571962478322,
-0.333989682311984));
#48428=CARTESIAN_POINT('Ctrl Pts',(0.13139353261958,-0.0943863800074581,
-0.326042391004034));
#48429=CARTESIAN_POINT('Ctrl Pts',(0.150493764788252,0.0593689810003615,
-0.318095099696081));
#48430=CARTESIAN_POINT('Ctrl Pts',(0.0315633627925462,0.158671999024367,
-0.310147808388131));
#48431=CARTESIAN_POINT('Ctrl Pts',(-0.116316484309744,0.112443428545168,
-0.302200517080177));
#48432=CARTESIAN_POINT('Ctrl Pts',(-0.157512588629431,-0.0369165757947868,
-0.294253225772227));
#48433=CARTESIAN_POINT('Ctrl Pts',(-0.0542404983500219,-0.152417247986887,
-0.286305934464274));
#48434=CARTESIAN_POINT('Ctrl Pts',(0.0987801671956758,-0.128123095942938,
-0.278358643156324));
#48435=CARTESIAN_POINT('Ctrl Pts',(0.161201138195067,0.0136836467989822,
-0.270411351848371));
#48436=CARTESIAN_POINT('Ctrl Pts',(0.0757708320050786,0.142939952995593,
-0.262464060540421));
#48437=CARTESIAN_POINT('Ctrl Pts',(-0.0791553500289386,0.141093868425444,
-0.254516769232468));
#48438=CARTESIAN_POINT('Ctrl Pts',(-0.16148142681772,0.00983859429043673,
-0.246569477924517));
#48439=CARTESIAN_POINT('Ctrl Pts',(-0.0956991498812775,-0.13044049163145,
-0.238622186616566));
#48440=CARTESIAN_POINT('Ctrl Pts',(0.0578569585295865,-0.151081506137494,
-0.230674895308614));
#48441=CARTESIAN_POINT('Ctrl Pts',(0.158347528374801,-0.0331528188732168,
-0.222727604000663));
#48442=CARTESIAN_POINT('Ctrl Pts',(0.113604109384946,0.115183138854537,
-0.21478031269271));
#48443=CARTESIAN_POINT('Ctrl Pts',(-0.0353353026649132,0.157874841386009,
-0.206833021384759));
#48444=CARTESIAN_POINT('Ctrl Pts',(-0.151865702554914,0.0557660963925229,
-0.198885730076807));
#48445=CARTESIAN_POINT('Ctrl Pts',(-0.129107147668427,-0.0974904794131229,
-0.190938438768856));
#48446=CARTESIAN_POINT('Ctrl Pts',(0.0120665558918105,-0.161330243433346,
-0.182991147460904));
#48447=CARTESIAN_POINT('Ctrl Pts',(0.142172993736196,-0.0772003161421253,
-0.175043856152953));
#48448=CARTESIAN_POINT('Ctrl Pts',(0.141880485927735,0.0777365871248822,
-0.167096564845001));
#48449=CARTESIAN_POINT('Ctrl Pts',(0.0114573118176813,0.161374655912202,
-0.15914927353705));
#48450=CARTESIAN_POINT('Ctrl Pts',(-0.129474332107829,0.0970022946962231,
-0.151201982229098));
#48451=CARTESIAN_POINT('Ctrl Pts',(-0.151654062184562,-0.0563391135504591,
-0.143254690921146));
#48452=CARTESIAN_POINT('Ctrl Pts',(-0.0347389307465692,-0.158007145849288,
-0.135307399613195));
#48453=CARTESIAN_POINT('Ctrl Pts',(0.114038191537599,-0.114753349174383,
-0.127360108305243));
#48454=CARTESIAN_POINT('Ctrl Pts',(0.15822125885756,0.0337504417737982,
-0.119412816997291));
#48455=CARTESIAN_POINT('Ctrl Pts',(0.0572860137252658,0.15129895347779,
-0.11146552568934));
#48456=CARTESIAN_POINT('Ctrl Pts',(-0.096190849571472,0.130078092307543,
-0.103518234381388));
#48457=CARTESIAN_POINT('Ctrl Pts',(-0.161443392134426,-0.0104480133107038,
-0.0955709430734366));
#48458=CARTESIAN_POINT('Ctrl Pts',(-0.0786215350791608,-0.141392191761692,
-0.0876236517654851));
#48459=CARTESIAN_POINT('Ctrl Pts',(0.0763090534835393,-0.142651978679687,
-0.0796763604575335));
#48460=CARTESIAN_POINT('Ctrl Pts',(0.161253470770041,-0.0130765076804255,
-0.071729069149582));
#48461=CARTESIAN_POINT('Ctrl Pts',(0.0982922472958529,0.128498248794366,
-0.0637817778416304));
#48462=CARTESIAN_POINT('Ctrl Pts',(-0.0548090762867236,0.152205495472761,
-0.0558344865336785));
#48463=CARTESIAN_POINT('Ctrl Pts',(-0.157663267928126,0.036332702127111,
-0.0478871952257271));
#48464=CARTESIAN_POINT('Ctrl Pts',(-0.115867512298235,-0.112902967751805,
-0.0399399039177751));
#48465=CARTESIAN_POINT('Ctrl Pts',(0.0321173634886005,-0.158511366575469,
-0.0319926126098238));
#48466=CARTESIAN_POINT('Ctrl Pts',(0.150803302304377,-0.0588783810225519,
-0.0240453213018721));
#48467=CARTESIAN_POINT('Ctrl Pts',(0.130861723774648,0.0950427942614887,
-0.0160980299939207));
#48468=CARTESIAN_POINT('Ctrl Pts',(0.0380135549211517,0.13910682119594,
-0.0107998357886196));
#48469=CARTESIAN_POINT('Ctrl Pts',(-0.00746697525422262,0.136621099781669,
-0.00815073868596909));
#48470=CARTESIAN_POINT('Ctrl Pts',(-0.120752812127176,0.0402994834133023,
-2.94314926131403));
#48471=CARTESIAN_POINT('Ctrl Pts',(-0.13416832315995,0.000101432566926213,
-2.94050016421138));
#48472=CARTESIAN_POINT('Ctrl Pts',(-0.117464253761176,-0.0940473201527993,
-2.93520197000608));
#48473=CARTESIAN_POINT('Ctrl Pts',(0.0157439008632371,-0.149794811235546,
-2.92725467869813));
#48474=CARTESIAN_POINT('Ctrl Pts',(0.13433249399984,-0.0678016115647968,
-2.91930738739018));
#48475=CARTESIAN_POINT('Ctrl Pts',(0.129802517580256,0.0762007396464412,
-2.91136009608222));
#48476=CARTESIAN_POINT('Ctrl Pts',(0.00617326309182846,0.150405521063703,
-2.90341280477427));
#48477=CARTESIAN_POINT('Ctrl Pts',(-0.123093674514204,0.0866119181392443,
-2.89546551346632));
#48478=CARTESIAN_POINT('Ctrl Pts',(-0.139473746844836,-0.0565952056747279,
-2.88751822215837));
#48479=CARTESIAN_POINT('Ctrl Pts',(-0.0279238304536315,-0.147907557093408,
-2.87957093085042));
#48480=CARTESIAN_POINT('Ctrl Pts',(0.109233850025249,-0.103554190495644,
-2.87162363954247));
#48481=CARTESIAN_POINT('Ctrl Pts',(0.146205747724809,0.0357737851326773,
-2.86367634823451));
#48482=CARTESIAN_POINT('Ctrl Pts',(0.0490789294142754,0.142292553953765,
-2.85572905692656));
#48483=CARTESIAN_POINT('Ctrl Pts',(-0.0930618301676024,0.118301676336187,
-2.84778176561861));
#48484=CARTESIAN_POINT('Ctrl Pts',(-0.14984794252219,-0.0141931844243834,
-2.83983447431066));
#48485=CARTESIAN_POINT('Ctrl Pts',(-0.069195614913156,-0.133670557112622,
-2.83188718300271));
#48486=CARTESIAN_POINT('Ctrl Pts',(0.0749218215473602,-0.130547138405,-2.82393989169476));
#48487=CARTESIAN_POINT('Ctrl Pts',(0.150322121943934,-0.00768791359722427,
-2.81599260038681));
#48488=CARTESIAN_POINT('Ctrl Pts',(0.0878491953235926,0.122222593007361,
-2.80804530907885));
#48489=CARTESIAN_POINT('Ctrl Pts',(-0.0551976905231906,0.140032339864175,
-2.80009801777091));
#48490=CARTESIAN_POINT('Ctrl Pts',(-0.147618084592067,0.0294065270266016,
-2.79215072646295));
#48491=CARTESIAN_POINT('Ctrl Pts',(-0.104645372351645,-0.10819051952984,
-2.784203435155));
#48492=CARTESIAN_POINT('Ctrl Pts',(0.0343065114091399,-0.146556833624553,
-2.77625614384705));
#48493=CARTESIAN_POINT('Ctrl Pts',(0.141792975964607,-0.0505034097530179,
-2.76830885253909));
#48494=CARTESIAN_POINT('Ctrl Pts',(0.119229039509039,0.0918709884218048,
-2.76036156123115));
#48495=CARTESIAN_POINT('Ctrl Pts',(-0.0126899916351106,0.149982687191073,
-2.75241426992319));
#48496=CARTESIAN_POINT('Ctrl Pts',(-0.132969952040698,0.0705325047882228,
-2.74446697861524));
#48497=CARTESIAN_POINT('Ctrl Pts',(-0.131291857634228,-0.0736090380752462,
-2.73651968730729));
#48498=CARTESIAN_POINT('Ctrl Pts',(-0.00919483165182608,-0.150237470142918,
-2.72857239599934));
#48499=CARTESIAN_POINT('Ctrl Pts',(0.121335556659434,-0.0890703377050207,
-2.72062510469138));
#48500=CARTESIAN_POINT('Ctrl Pts',(0.14057878395503,0.053790778658821,-2.71267781338343));
#48501=CARTESIAN_POINT('Ctrl Pts',(0.0308852494790753,0.147315795932769,
-2.70473052207548));
#48502=CARTESIAN_POINT('Ctrl Pts',(-0.107135774699351,0.105724964634277,
-2.69678323076753));
#48503=CARTESIAN_POINT('Ctrl Pts',(-0.146893465878803,-0.0328352257365663,
-2.68883593945958));
#48504=CARTESIAN_POINT('Ctrl Pts',(-0.0519226633012332,-0.141279437296261,
-2.68088864815163));
#48505=CARTESIAN_POINT('Ctrl Pts',(0.0906708308417741,-0.120144258296409,
-2.67294135684367));
#48506=CARTESIAN_POINT('Ctrl Pts',(0.150102392668563,0.0111854406376042,
-2.66499406553573));
#48507=CARTESIAN_POINT('Ctrl Pts',(0.0718622809959905,0.132256020419261,
-2.65704677422777));
#48508=CARTESIAN_POINT('Ctrl Pts',(-0.0722888418891832,0.132023352879024,
-2.64909948291982));
#48509=CARTESIAN_POINT('Ctrl Pts',(-0.150137718279179,0.0107008372108558,
-2.64115219161187));
#48510=CARTESIAN_POINT('Ctrl Pts',(-0.0902825210470809,-0.120436326581624,
-2.63320490030392));
#48511=CARTESIAN_POINT('Ctrl Pts',(0.0523784565548806,-0.141111089769806,
-2.62525760899597));
#48512=CARTESIAN_POINT('Ctrl Pts',(0.146998695824624,-0.0323608682354538,
-2.61731031768802));
#48513=CARTESIAN_POINT('Ctrl Pts',(0.106793926001398,0.106070258490779,
-2.60936302638006));
#48514=CARTESIAN_POINT('Ctrl Pts',(-0.031360638297492,0.147215327777602,
-2.60141573507211));
#48515=CARTESIAN_POINT('Ctrl Pts',(-0.140751693369979,0.0533366963785367,
-2.59346844376416));
#48516=CARTESIAN_POINT('Ctrl Pts',(-0.121047396732009,-0.0894615566123041,
-2.58552115245621));
#48517=CARTESIAN_POINT('Ctrl Pts',(0.00967976492882044,-0.150207005555719,
-2.57757386114826));
#48518=CARTESIAN_POINT('Ctrl Pts',(0.131528790717594,-0.073184831621452,
-2.56962656984031));
#48519=CARTESIAN_POINT('Ctrl Pts',(0.132741573409056,0.0709613772131088,
-2.56167927853235));
#48520=CARTESIAN_POINT('Ctrl Pts',(0.012205766825665,0.150022870334127,
-2.5537319872244));
#48521=CARTESIAN_POINT('Ctrl Pts',(-0.119524986855898,0.0914856266535366,
-2.54578469591645));
#48522=CARTESIAN_POINT('Ctrl Pts',(-0.141629207123113,-0.0509608678965643,
-2.5378374046085));
#48523=CARTESIAN_POINT('Ctrl Pts',(-0.0338332331669371,-0.146666815267001,
-2.52989011330055));
#48524=CARTESIAN_POINT('Ctrl Pts',(0.104994077113604,-0.107852149436882,
-2.5219428219926));
#48525=CARTESIAN_POINT('Ctrl Pts',(0.147522387446294,0.0298828976044573,
-2.51399553068464));
#48526=CARTESIAN_POINT('Ctrl Pts',(0.0547453665494287,0.140209797120107,
-2.5060482393767));
#48527=CARTESIAN_POINT('Ctrl Pts',(-0.0882432871882518,0.121938364075071,
-2.49810094806874));
#48528=CARTESIAN_POINT('Ctrl Pts',(-0.150296515405261,-0.00817311593757486,
-2.49015365676079));
#48529=CARTESIAN_POINT('Ctrl Pts',(-0.0745000236469882,-0.130788336038391,
-2.48220636545284));
#48530=CARTESIAN_POINT('Ctrl Pts',(0.0696267775013432,-0.133446447018537,
-2.47425907414489));
#48531=CARTESIAN_POINT('Ctrl Pts',(0.149892937865947,-0.0137094691731059,
-2.46631178283693));
#48532=CARTESIAN_POINT('Ctrl Pts',(0.09267953354884,0.11860162911302,-2.45836449152898));
#48533=CARTESIAN_POINT('Ctrl Pts',(-0.0495381552169006,0.142133083920666,
-2.45041720022103));
#48534=CARTESIAN_POINT('Ctrl Pts',(-0.146320187631405,0.0353021962291781,
-2.44246990891308));
#48535=CARTESIAN_POINT('Ctrl Pts',(-0.108899528537508,-0.103907338775475,
-2.43452261760512));
#48536=CARTESIAN_POINT('Ctrl Pts',(0.0284021522411427,-0.147814614010807,
-2.42657532629718));
#48537=CARTESIAN_POINT('Ctrl Pts',(0.139653803033537,-0.0561485321746081,
-2.41862803498922));
#48538=CARTESIAN_POINT('Ctrl Pts',(0.122817070740355,0.087016145064302,
-2.41068074368128));
#48539=CARTESIAN_POINT('Ctrl Pts',(-0.00666564515458532,0.150370913217171,
-2.40273345237332));
#48540=CARTESIAN_POINT('Ctrl Pts',(-0.130034730833038,0.075807724832447,
-2.39478616106537));
#48541=CARTESIAN_POINT('Ctrl Pts',(-0.134137902833708,-0.0682851769454208,
-2.38683886975742));
#48542=CARTESIAN_POINT('Ctrl Pts',(-0.0152117930586876,-0.149747933939112,
-2.37889157844947));
#48543=CARTESIAN_POINT('Ctrl Pts',(0.117666346194914,-0.0938641216878506,
-2.37094428714152));
#48544=CARTESIAN_POINT('Ctrl Pts',(0.142622669498577,0.0481104615670283,
-2.36299699583356));
#48545=CARTESIAN_POINT('Ctrl Pts',(0.0367676097206484,0.145958847770606,
-2.35504970452561));
#48546=CARTESIAN_POINT('Ctrl Pts',(-0.102810152745931,0.109935957991238,
-2.34710241321766));
#48547=CARTESIAN_POINT('Ctrl Pts',(-0.148091978088299,-0.026918551093764,
-2.33915512190971));
#48548=CARTESIAN_POINT('Ctrl Pts',(-0.0575460521683576,-0.139083767014448,
-2.33120783060176));
#48549=CARTESIAN_POINT('Ctrl Pts',(0.0857802536273329,-0.123683428375524,
-2.32326053929381));
#48550=CARTESIAN_POINT('Ctrl Pts',(0.150430191510887,0.0051575041532583,
-2.31531324798585));
#48551=CARTESIAN_POINT('Ctrl Pts',(0.0771078036908864,0.129268050875151,
-2.3073659566779));
#48552=CARTESIAN_POINT('Ctrl Pts',(-0.0669367104408037,0.134815871329962,
-2.29941866536995));
#48553=CARTESIAN_POINT('Ctrl Pts',(-0.1495878731335,0.0167125874265122,
-2.291471374062));
#48554=CARTESIAN_POINT('Ctrl Pts',(-0.0950392719624149,-0.116719232142552,
-2.28352408275405));
#48555=CARTESIAN_POINT('Ctrl Pts',(0.0466779304989097,-0.14309791462992,
-2.27557679144609));
#48556=CARTESIAN_POINT('Ctrl Pts',(0.145582832016662,-0.0382293262967235,
-2.26762950013815));
#48557=CARTESIAN_POINT('Ctrl Pts',(0.110961333587,0.101702629345004,-2.25968220883019));
#48558=CARTESIAN_POINT('Ctrl Pts',(-0.0254322433356824,0.148354451790324,
-2.25173491752225));
#48559=CARTESIAN_POINT('Ctrl Pts',(-0.138499746378915,0.0589377860126174,
-2.24378762621429));
#48560=CARTESIAN_POINT('Ctrl Pts',(-0.124537349869914,-0.0845357371439527,
-2.23584033490634));
#48561=CARTESIAN_POINT('Ctrl Pts',(0.00364884457439508,-0.150474344326084,
-2.22789304359839));
#48562=CARTESIAN_POINT('Ctrl Pts',(0.128488373252985,-0.0784001295017715,
-2.21994575229044));
#48563=CARTESIAN_POINT('Ctrl Pts',(0.135480284338815,0.0655815135733136,
-2.21199846098248));
#48564=CARTESIAN_POINT('Ctrl Pts',(0.0182117013744718,0.14941277154293,
-2.20405116967453));
#48565=CARTESIAN_POINT('Ctrl Pts',(-0.115760382186509,0.0962048662133375,
-2.19610387836658));
#48566=CARTESIAN_POINT('Ctrl Pts',(-0.143558771529671,-0.0452407060509069,
-2.18815658705863));
#48567=CARTESIAN_POINT('Ctrl Pts',(-0.0396871989844945,-0.145192178177263,
-2.18020929575068));
#48568=CARTESIAN_POINT('Ctrl Pts',(0.100584879932131,-0.111975552225169,
-2.17226200444273));
#48569=CARTESIAN_POINT('Ctrl Pts',(0.148602008725634,0.0239433784124045,
-2.16431471313477));
#48570=CARTESIAN_POINT('Ctrl Pts',(0.0603235937711138,0.137901799849134,
-2.15636742182682));
#48571=CARTESIAN_POINT('Ctrl Pts',(-0.0832827207479992,0.125378749363293,
-2.14842013051887));
#48572=CARTESIAN_POINT('Ctrl Pts',(-0.150503367223278,-0.00213981811093342,
-2.14047283921092));
#48573=CARTESIAN_POINT('Ctrl Pts',(-0.0796845723241252,-0.127695776361688,
-2.13252554790297));
#48574=CARTESIAN_POINT('Ctrl Pts',(0.0642197226054989,-0.136131075054764,
-2.12457825659501));
#48575=CARTESIAN_POINT('Ctrl Pts',(0.149222646773545,-0.0197089841694217,
-2.11663096528707));
#48576=CARTESIAN_POINT('Ctrl Pts',(0.0973607872422648,0.11478989273738,
-2.10868367397911));
#48577=CARTESIAN_POINT('Ctrl Pts',(-0.0437989327332868,0.14400519385952,
-2.10073638267116));
#48578=CARTESIAN_POINT('Ctrl Pts',(-0.144786925531932,0.0411410811975513,
-2.09278909136321));
#48579=CARTESIAN_POINT('Ctrl Pts',(-0.11297851192793,-0.0994570168949558,
-2.08484180005526));
#48580=CARTESIAN_POINT('Ctrl Pts',(0.0224521060265546,-0.148834624002835,
-2.07689450874731));
#48581=CARTESIAN_POINT('Ctrl Pts',(0.137289987547526,-0.0617033361034314,
-2.06894721743936));
#48582=CARTESIAN_POINT('Ctrl Pts',(0.126207542254494,0.0820213304279625,
-2.0609999261314));
#48583=CARTESIAN_POINT('Ctrl Pts',(-0.000630576492705186,0.150517257284272,
-2.05305263482345));
#48584=CARTESIAN_POINT('Ctrl Pts',(-0.126890339895417,0.0809610030095871,
-2.0451053435155));
#48585=CARTESIAN_POINT('Ctrl Pts',(-0.136768178042001,-0.0628514744629297,
-2.03715805220755));
#48586=CARTESIAN_POINT('Ctrl Pts',(-0.021204285262339,-0.149017517942039,
-2.0292107608996));
#48587=CARTESIAN_POINT('Ctrl Pts',(0.11380786137609,-0.0985069188234697,
-2.02126346959164));
#48588=CARTESIAN_POINT('Ctrl Pts',(0.144437136732523,0.0423527555137007,
-2.0133161782837));
#48589=CARTESIAN_POINT('Ctrl Pts',(0.0425908267507145,0.144367114828078,
-2.00536888697574));
#48590=CARTESIAN_POINT('Ctrl Pts',(-0.0983191536380268,0.113970111849532,
-1.99742159566779));
#48591=CARTESIAN_POINT('Ctrl Pts',(-0.14905227423289,-0.0209585761228194,
-1.98947430435984));
#48592=CARTESIAN_POINT('Ctrl Pts',(-0.0630768742790228,-0.136664370990691,
-1.98152701305189));
#48593=CARTESIAN_POINT('Ctrl Pts',(0.0807516930143136,-0.127023645209918,
-1.97357972174394));
#48594=CARTESIAN_POINT('Ctrl Pts',(0.150516013112444,-0.000878728528827487,
-1.96563243043598));
#48595=CARTESIAN_POINT('Ctrl Pts',(0.0822292932154056,0.126072144839324,
-1.95768513912803));
#48596=CARTESIAN_POINT('Ctrl Pts',(-0.061476906720437,0.137391529240996,
-1.94973784782008));
#48597=CARTESIAN_POINT('Ctrl Pts',(-0.148797405673741,0.0226974543034491,
-1.94179055651213));
#48598=CARTESIAN_POINT('Ctrl Pts',(-0.0996431457155294,-0.112814386844085,
-1.93384326520418));
#48599=CARTESIAN_POINT('Ctrl Pts',(0.040902319802603,-0.14485455671762,
-1.92589597389623));
#48600=CARTESIAN_POINT('Ctrl Pts',(0.143932788276891,-0.0440362898747423,
-1.91794868258827));
#48601=CARTESIAN_POINT('Ctrl Pts',(0.114950252286431,0.0971714045714007,
-1.91000139128032));
#48602=CARTESIAN_POINT('Ctrl Pts',(-0.019462938872886,0.149254937531471,
-1.90205409997237));
#48603=CARTESIAN_POINT('Ctrl Pts',(-0.136025013083223,0.0644440701911498,
-1.89410680866442));
#48604=CARTESIAN_POINT('Ctrl Pts',(-0.127826976171915,-0.0794739361667551,
-1.88615951735647));
#48605=CARTESIAN_POINT('Ctrl Pts',(-0.00238794519582686,-0.150499634832894,
-1.87821222604852));
#48606=CARTESIAN_POINT('Ctrl Pts',(0.125241273461417,-0.0834893154173368,
-1.87026493474057));
#48607=CARTESIAN_POINT('Ctrl Pts',(0.138001065974934,0.0600961575882769,
-1.86231764343261));
#48608=CARTESIAN_POINT('Ctrl Pts',(0.0241883411573577,0.14856233210053,
-1.85437035212466));
#48609=CARTESIAN_POINT('Ctrl Pts',(-0.111809569033394,0.100769353672927,
-1.84642306081671));
#48610=CARTESIAN_POINT('Ctrl Pts',(-0.145257411844003,-0.0394477714386299,
-1.83847576950876));
#48611=CARTESIAN_POINT('Ctrl Pts',(-0.0454773252309796,-0.143483989549109,
-1.83052847820081));
#48612=CARTESIAN_POINT('Ctrl Pts',(0.0960138850991289,-0.115918834687312,
-1.82258118689285));
#48613=CARTESIAN_POINT('Ctrl Pts',(0.149442593521154,0.0179653446603165,
-1.8146338955849));
#48614=CARTESIAN_POINT('Ctrl Pts',(0.0658047863707909,0.135371978111378,
-1.80668660427695));
#48615=CARTESIAN_POINT('Ctrl Pts',(-0.0781881883613825,0.12861745436704,
-1.798739312969));
#48616=CARTESIAN_POINT('Ctrl Pts',(-0.150468124092429,0.00389692175933637,
-1.79079202166105));
#48617=CARTESIAN_POINT('Ctrl Pts',(-0.0847409429224701,-0.124397809304279,
-1.7828447303531));
#48618=CARTESIAN_POINT('Ctrl Pts',(0.0587093658982245,-0.138596726956018,
-1.77489743904515));
#48619=CARTESIAN_POINT('Ctrl Pts',(0.148312320858622,-0.0256767959181446,
-1.76695014773719));
#48620=CARTESIAN_POINT('Ctrl Pts',(0.101885429457528,0.110793508976599,
-1.75900285642924));
#48621=CARTESIAN_POINT('Ctrl Pts',(-0.0379892566739397,0.14564566160533,
-1.75105556512129));
#48622=CARTESIAN_POINT('Ctrl Pts',(-0.143020763770612,0.0469137879259792,
-1.74310827381334));
#48623=CARTESIAN_POINT('Ctrl Pts',(-0.116875761663,-0.0948467116076595,
-1.73516098250539));
#48624=CARTESIAN_POINT('Ctrl Pts',(0.0164659440654498,-0.149615223333477,
-1.72721369119744));
#48625=CARTESIAN_POINT('Ctrl Pts',(0.13470533173662,-0.0671588860004383,
-1.71926639988949));
#48626=CARTESIAN_POINT('Ctrl Pts',(0.129395000314167,0.0768945788777685,
-1.71131910858153));
#48627=CARTESIAN_POINT('Ctrl Pts',(0.00540550649454605,0.150421484059394,
-1.70337181727358));
#48628=CARTESIAN_POINT('Ctrl Pts',(-0.123541837176675,0.0859840498819692,
-1.69542452596563));
#48629=CARTESIAN_POINT('Ctrl Pts',(-0.139178452291639,-0.0573166710896298,
-1.68747723465768));
#48630=CARTESIAN_POINT('Ctrl Pts',(-0.0271626689244233,-0.148047397086186,
-1.67952994334973));
#48631=CARTESIAN_POINT('Ctrl Pts',(0.109766308836665,-0.10299126084997,
-1.67158265204177));
#48632=CARTESIAN_POINT('Ctrl Pts',(0.146019266963803,0.0365269221595056,
-1.66363536073383));
#48633=CARTESIAN_POINT('Ctrl Pts',(0.0483455335260618,0.142543157517902,
-1.65568806942587));
#48634=CARTESIAN_POINT('Ctrl Pts',(-0.0936700014541382,0.117820936996251,
-1.64774077811792));
#48635=CARTESIAN_POINT('Ctrl Pts',(-0.149772809610831,-0.0149648878502536,
-1.63979348680997));
#48636=CARTESIAN_POINT('Ctrl Pts',(-0.0685062329278706,-0.134025140989014,
-1.63184619550202));
#48637=CARTESIAN_POINT('Ctrl Pts',(0.0755932377859644,-0.130159535832484,
-1.62389890419406));
#48638=CARTESIAN_POINT('Ctrl Pts',(0.150359719423358,-0.006913547716038,
-1.61595161288612));
#48639=CARTESIAN_POINT('Ctrl Pts',(0.0872185113037171,0.122673443145027,
-1.60800432157816));
#48640=CARTESIAN_POINT('Ctrl Pts',(-0.0559182131953897,0.139746183490383,
-1.60005703027021));
#48641=CARTESIAN_POINT('Ctrl Pts',(-0.147767587420821,0.0286458107744018,
-1.59210973896226));
#48642=CARTESIAN_POINT('Ctrl Pts',(-0.104086736660943,-0.108728071896675,
-1.58416244765431));
#48643=CARTESIAN_POINT('Ctrl Pts',(0.0350609149303666,-0.146378190354091,
-1.57621515634636));
#48644=CARTESIAN_POINT('Ctrl Pts',(0.142051218813405,-0.0497724180718481,
-1.5682678650384));
#48645=CARTESIAN_POINT('Ctrl Pts',(0.118754265651428,0.0924838729546011,
-1.56032057373045));
#48646=CARTESIAN_POINT('Ctrl Pts',(-0.0134623269431637,0.149915336508204,
-1.5523732824225));
#48647=CARTESIAN_POINT('Ctrl Pts',(-0.133331474260487,0.0698466916798358,
-1.54442599111455));
#48648=CARTESIAN_POINT('Ctrl Pts',(-0.130910984049351,-0.074284295933417,
-1.5364786998066));
#48649=CARTESIAN_POINT('Ctrl Pts',(-0.00842089379304925,-0.150282836394643,
-1.52853140849865));
#48650=CARTESIAN_POINT('Ctrl Pts',(0.121792714524754,-0.0884442030648959,
-1.52058411719069));
#48651=CARTESIAN_POINT('Ctrl Pts',(0.140299863467925,0.0545141328278685,
-1.51263682588274));
#48652=CARTESIAN_POINT('Ctrl Pts',(0.0301260723408991,0.147472919996872,
-1.50468953457479));
#48653=CARTESIAN_POINT('Ctrl Pts',(-0.107678902549438,0.105171746742371,
-1.49674224326684));
#48654=CARTESIAN_POINT('Ctrl Pts',(-0.146722395687109,-0.0335913823908467,
-1.48879495195889));
#48655=CARTESIAN_POINT('Ctrl Pts',(-0.0511942980927276,-0.141544997120653,
-1.48084766065094));
#48656=CARTESIAN_POINT('Ctrl Pts',(0.0912884453720831,-0.119675653784055,
-1.47290036934298));
#48657=CARTESIAN_POINT('Ctrl Pts',(0.150042789694782,0.0119584124239118,
-1.46495307803503));
#48658=CARTESIAN_POINT('Ctrl Pts',(0.071180127475677,0.132624401297949,
-1.45700578672708));
#48659=CARTESIAN_POINT('Ctrl Pts',(-0.0729678849318161,0.131649269408037,
-1.44905849541913));
#48660=CARTESIAN_POINT('Ctrl Pts',(-0.150190842703695,0.00992739316471041,
-1.44111120411118));
#48661=CARTESIAN_POINT('Ctrl Pts',(-0.0896610019244564,-0.120899739871496,
-1.43316391280323));
#48662=CARTESIAN_POINT('Ctrl Pts',(0.0531045711647607,-0.140839436552763,
-1.42521662149528));
#48663=CARTESIAN_POINT('Ctrl Pts',(0.147163424442606,-0.0316033047863433,
-1.41726933018732));
#48664=CARTESIAN_POINT('Ctrl Pts',(0.106246181998494,0.106618906286998,
-1.40932203887937));
#48665=CARTESIAN_POINT('Ctrl Pts',(-0.0321184722997344,0.147051848353647,
-1.40137474757142));
#48666=CARTESIAN_POINT('Ctrl Pts',(-0.141024543339304,0.0526110306212836,
-1.39342745626347));
#48667=CARTESIAN_POINT('Ctrl Pts',(-0.120585008750252,-0.0900838389046252,
-1.38548016495552));
#48668=CARTESIAN_POINT('Ctrl Pts',(0.0104532955083284,-0.15015515635538,
-1.37753287364757));
#48669=CARTESIAN_POINT('Ctrl Pts',(0.131903993196282,-0.0725064062408852,
-1.36958558233961));
#48670=CARTESIAN_POINT('Ctrl Pts',(0.132374317675311,0.0716441371438625,
-1.36163829103166));
#48671=CARTESIAN_POINT('Ctrl Pts',(0.0114328943552846,0.15008374760031,
-1.35369099972371));
#48672=CARTESIAN_POINT('Ctrl Pts',(-0.119994608972208,0.0908687855355161,
-1.34574370841576));
#48673=CARTESIAN_POINT('Ctrl Pts',(-0.141364848491819,-0.0516896699348911,
-1.33779641710781));
#48674=CARTESIAN_POINT('Ctrl Pts',(-0.0330773595777369,-0.146839131877228,
-1.32984912579986));
#48675=CARTESIAN_POINT('Ctrl Pts',(0.105548189690026,-0.107309934396826,
-1.3219018344919));
#48676=CARTESIAN_POINT('Ctrl Pts',(0.147366515227844,0.0306423327554257,
-1.31395454318395));
#48677=CARTESIAN_POINT('Ctrl Pts',(0.054022473207671,0.140489909800025,
-1.306007251876));
#48678=CARTESIAN_POINT('Ctrl Pts',(-0.0888701746731883,0.121482239116054,
-1.29805996056805));
#48679=CARTESIAN_POINT('Ctrl Pts',(-0.150252425191737,-0.00894712753314866,
-1.2901126692601));
#48680=CARTESIAN_POINT('Ctrl Pts',(-0.0738253946205713,-0.131170322391194,
-1.28216537795214));
#48681=CARTESIAN_POINT('Ctrl Pts',(0.0703131856699568,-0.133086055948905,
-1.2742180866442));
#48682=CARTESIAN_POINT('Ctrl Pts',(0.149961561852704,-0.0129372459894017,
-1.26627079533624));
#48683=CARTESIAN_POINT('Ctrl Pts',(0.0920674324576578,0.119077412836136,
-1.25832350402829));
#48684=CARTESIAN_POINT('Ctrl Pts',(-0.0502695714039735,0.14187604645589,
-1.25037621272034));
#48685=CARTESIAN_POINT('Ctrl Pts',(-0.146500074907761,0.0345480885015839,
-1.24242892141239));
#48686=CARTESIAN_POINT('Ctrl Pts',(-0.108362896979023,-0.104466860417102,
-1.23448163010444));
#48687=CARTESIAN_POINT('Ctrl Pts',(0.0291631121810312,-0.147666364670528,
-1.22653433879648));
#48688=CARTESIAN_POINT('Ctrl Pts',(0.139941150259236,-0.0554284839339382,
-1.21858704748853));
#48689=CARTESIAN_POINT('Ctrl Pts',(0.122367254666599,0.0876475747094732,
-1.21063975618058));
#48690=CARTESIAN_POINT('Ctrl Pts',(-0.00744005994078389,0.150334586423651,
-1.20269246487263));
#48691=CARTESIAN_POINT('Ctrl Pts',(-0.130423462651932,0.0751369599928877,
-1.19474517356468));
#48692=CARTESIAN_POINT('Ctrl Pts',(-0.133784412664846,-0.0689751643348171,
-1.18679788225673));
#48693=CARTESIAN_POINT('Ctrl Pts',(-0.0144402968072766,-0.149824297746429,
-1.17885059094878));
#48694=CARTESIAN_POINT('Ctrl Pts',(0.118148243685659,-0.0932568221691426,
-1.17090329964082));
#48695=CARTESIAN_POINT('Ctrl Pts',(0.142372979044962,0.0488444183602959,
-1.16295600833287));
#48696=CARTESIAN_POINT('Ctrl Pts',(0.0360153436788049,0.146146287625756,
-1.15500871702492));
#48697=CARTESIAN_POINT('Ctrl Pts',(-0.103375027193893,0.109404963871639,
-1.14706142571697));
#48698=CARTESIAN_POINT('Ctrl Pts',(-0.147951366532389,-0.0276809593094551,
-1.13911413440902));
#48699=CARTESIAN_POINT('Ctrl Pts',(-0.0568289214282981,-0.139378319893695,
-1.13116684310107));
#48700=CARTESIAN_POINT('Ctrl Pts',(0.086416161943652,-0.123239966415207,
-1.12321955179311));
#48701=CARTESIAN_POINT('Ctrl Pts',(0.150401631789964,0.0059322442641027,
-1.11527226048516));
#48702=CARTESIAN_POINT('Ctrl Pts',(0.076440970482352,0.129663489073867,
-1.10732496917721));
#48703=CARTESIAN_POINT('Ctrl Pts',(-0.0676302076740239,0.134469317604654,
-1.09937767786926));
#48704=CARTESIAN_POINT('Ctrl Pts',(-0.149671969083137,0.0159418956799199,
-1.09143038656131));
#48705=CARTESIAN_POINT('Ctrl Pts',(-0.0944368350790274,-0.117207194947022,
-1.08348309525336));
#48706=CARTESIAN_POINT('Ctrl Pts',(0.0474143541003698,-0.142855596293381,
-1.0755358039454));
#48707=CARTESIAN_POINT('Ctrl Pts',(0.145777805603875,-0.037478977579594,
-1.06758851263745));
#48708=CARTESIAN_POINT('Ctrl Pts',(0.110436030296767,0.102272799802216,
-1.0596412213295));
#48709=CARTESIAN_POINT('Ctrl Pts',(-0.0261960231684342,0.148221492157014,
-1.05169393002155));
#48710=CARTESIAN_POINT('Ctrl Pts',(-0.138801475294959,0.0582236448793441,
-1.0437466387136));
#48711=CARTESIAN_POINT('Ctrl Pts',(-0.12410028661232,-0.0851760601920076,
-1.03579934740565));
#48712=CARTESIAN_POINT('Ctrl Pts',(0.00442383211119069,-0.150453554549384,
-1.02785205609769));
#48713=CARTESIAN_POINT('Ctrl Pts',(0.12889047807094,-0.0777372949731165,
-1.01990476478974));
#48714=CARTESIAN_POINT('Ctrl Pts',(0.135140701902402,0.066278450920486,
-1.01195747348179));
#48715=CARTESIAN_POINT('Ctrl Pts',(0.017441891624336,0.149504591179195,
-1.00401018217384));
#48716=CARTESIAN_POINT('Ctrl Pts',(-0.116254361240943,0.0956073525391913,
-0.996062890865889));
#48717=CARTESIAN_POINT('Ctrl Pts',(-0.143323849674872,-0.0459795224145226,
-0.988115599557936));
#48718=CARTESIAN_POINT('Ctrl Pts',(-0.0389388430382602,-0.145394665892303,
-0.980168308249987));
#48719=CARTESIAN_POINT('Ctrl Pts',(0.101160289069005,-0.11145599258258,
-0.972221016942033));
#48720=CARTESIAN_POINT('Ctrl Pts',(0.14847671438377,0.0247084530655609,
-0.964273725634083));
#48721=CARTESIAN_POINT('Ctrl Pts',(0.0596125140502044,0.138210674463686,
-0.95632643432613));
#48722=CARTESIAN_POINT('Ctrl Pts',(-0.0839273941444871,0.12494812875433,
-0.94837914301818));
#48723=CARTESIAN_POINT('Ctrl Pts',(-0.150490349481178,-0.00291497515011473,
-0.940431851710227));
#48724=CARTESIAN_POINT('Ctrl Pts',(-0.0790258031221334,-0.128104507367988,
-0.932484560402276));
#48725=CARTESIAN_POINT('Ctrl Pts',(0.0649200299908625,-0.135798498051631,
-0.924537269094323));
#48726=CARTESIAN_POINT('Ctrl Pts',(0.14932218086414,-0.0189401338186902,
-0.916589977786373));
#48727=CARTESIAN_POINT('Ctrl Pts',(0.0967682568562582,0.115289838373093,
-0.90864268647842));
#48728=CARTESIAN_POINT('Ctrl Pts',(-0.044540067572435,0.143777692107419,
-0.90069539517047));
#48729=CARTESIAN_POINT('Ctrl Pts',(-0.144996907015034,0.0403947932680219,
-0.892748103862517));
#48730=CARTESIAN_POINT('Ctrl Pts',(-0.112464748173748,-0.100037606855164,
-0.884800812554567));
#48731=CARTESIAN_POINT('Ctrl Pts',(0.02321839857327,-0.148717007550534,
-0.876853521246614));
#48732=CARTESIAN_POINT('Ctrl Pts',(0.137605976803818,-0.0609953892926366,
-0.868906229938663));
#48733=CARTESIAN_POINT('Ctrl Pts',(0.125783407592265,0.0826702893521688,
-0.860958938630711));
#48734=CARTESIAN_POINT('Ctrl Pts',(-0.00140582509366957,0.150512012885679,
-0.85301164732276));
#48735=CARTESIAN_POINT('Ctrl Pts',(-0.127305655992913,0.0803063653722841,
-0.845064356014808));
#48736=CARTESIAN_POINT('Ctrl Pts',(-0.136442639912152,-0.0635550814718675,
-0.837117064706856));
#48737=CARTESIAN_POINT('Ctrl Pts',(-0.0204364716174977,-0.149124756478997,
-0.829169773398905));
#48738=CARTESIAN_POINT('Ctrl Pts',(0.114313723324471,-0.0979194313034393,
-0.821222482090953));
#48739=CARTESIAN_POINT('Ctrl Pts',(0.144217077958002,0.0430961343086391,
-0.813275190783001));
#48740=CARTESIAN_POINT('Ctrl Pts',(0.0418466818757667,0.14458456896599,
-0.805327899475051));
#48741=CARTESIAN_POINT('Ctrl Pts',(-0.0989048660443189,0.113462195641756,
-0.797380608167098));
#48742=CARTESIAN_POINT('Ctrl Pts',(-0.14894234749627,-0.0217260095137962,
-0.789433316859148));
#48743=CARTESIAN_POINT('Ctrl Pts',(-0.0623721315610867,-0.136987443116585,
-0.781486025551194));
#48744=CARTESIAN_POINT('Ctrl Pts',(0.0814048722146108,-0.126606039140381,
-0.773538734243244));
#48745=CARTESIAN_POINT('Ctrl Pts',(0.150518542584674,-0.000103466315906723,
-0.765591442935292));
#48746=CARTESIAN_POINT('Ctrl Pts',(0.081578852965405,0.126494004268746,
-0.75764415162734));
#48747=CARTESIAN_POINT('Ctrl Pts',(-0.0621837426065592,0.137073062716691,
-0.749696860319388));
#48748=CARTESIAN_POINT('Ctrl Pts',(-0.148912337874421,0.0219307545667479,
-0.741749569011437));
#48749=CARTESIAN_POINT('Ctrl Pts',(-0.0990607601322656,-0.113326114241646,
-0.733802277703485));
#48750=CARTESIAN_POINT('Ctrl Pts',(0.0416478678079634,-0.144641963047185,
-0.725854986395535));
#48751=CARTESIAN_POINT('Ctrl Pts',(0.144157693205001,-0.0432943628767713,
-0.717907695087582));
#48752=CARTESIAN_POINT('Ctrl Pts',(0.114448234695099,0.0977621805314748,
-0.709960403779631));
#48753=CARTESIAN_POINT('Ctrl Pts',(-0.0202314359441068,0.14915271156346,
-0.702013112471679));
#48754=CARTESIAN_POINT('Ctrl Pts',(-0.136355135594409,0.0637426024266583,
-0.694065821163728));
#48755=CARTESIAN_POINT('Ctrl Pts',(-0.127415940684595,-0.0801312699671765,
-0.686118529855775));
#48756=CARTESIAN_POINT('Ctrl Pts',(-0.00161274732213549,-0.150509937921613,
-0.678171238547825));
#48757=CARTESIAN_POINT('Ctrl Pts',(0.125669633805575,-0.0828431379552073,
-0.670223947239872));
#48758=CARTESIAN_POINT('Ctrl Pts',(0.137689703077396,0.0608061512805342,
-0.662276655931922));
#48759=CARTESIAN_POINT('Ctrl Pts',(0.0234228324190441,0.148684946408714,
-0.654329364623969));
#48760=CARTESIAN_POINT('Ctrl Pts',(-0.112327110426889,0.100192128584226,
-0.646382073316018));
#48761=CARTESIAN_POINT('Ctrl Pts',(-0.145052304653554,-0.0401954136909352,
-0.638434782008066));
#48762=CARTESIAN_POINT('Ctrl Pts',(-0.0447376907093767,-0.143716322653641,
-0.630487490700114));
#48763=CARTESIAN_POINT('Ctrl Pts',(0.0966096652115508,-0.115422766189367,
-0.622540199392163));
#48764=CARTESIAN_POINT('Ctrl Pts',(0.149348078600385,0.0187348281408182,
-0.614592908084211));
#48765=CARTESIAN_POINT('Ctrl Pts',(0.0651066640910347,0.135709117814648,
-0.60664561677626));
#48766=CARTESIAN_POINT('Ctrl Pts',(-0.0788496106682267,0.128213030790797,
-0.598698325468307));
#48767=CARTESIAN_POINT('Ctrl Pts',(-0.150486199761679,0.00312186616959324,
-0.590751034160356));
#48768=CARTESIAN_POINT('Ctrl Pts',(-0.0840990932201657,-0.124832627492329,
-0.582803742852406));
#48769=CARTESIAN_POINT('Ctrl Pts',(0.059422446008062,-0.138292498992215,
-0.574856451544453));
#48770=CARTESIAN_POINT('Ctrl Pts',(0.148442604945667,-0.024912555148708,
-0.566909160236502));
#48771=CARTESIAN_POINT('Ctrl Pts',(0.101313422902309,0.111316812328195,
-0.55896186892855));
#48772=CARTESIAN_POINT('Ctrl Pts',(-0.0387389179991394,0.145448061518017,
-0.551014577620599));
#48773=CARTESIAN_POINT('Ctrl Pts',(-0.1432605016909,0.0461765202496334,
-0.543067286312647));
#48774=CARTESIAN_POINT('Ctrl Pts',(-0.116385692137217,-0.0954474359678359,
-0.535119995004695));
#48775=CARTESIAN_POINT('Ctrl Pts',(0.0172363365850853,-0.149528428963252,
-0.527172703696744));
#48776=CARTESIAN_POINT('Ctrl Pts',(0.135049454733197,-0.0664641794003264,
-0.519225412388791));
#48777=CARTESIAN_POINT('Ctrl Pts',(0.128997229313045,0.0775600231862417,
-0.511278121080841));
#48778=CARTESIAN_POINT('Ctrl Pts',(0.00463067111916099,0.1504473304917,
-0.503330829772888));
#48779=CARTESIAN_POINT('Ctrl Pts',(-0.123983069488452,0.0853465924762928,
-0.495383538464938));
#48780=CARTESIAN_POINT('Ctrl Pts',(-0.138881389851128,-0.0580327659181574,
-0.487436247156985));
#48781=CARTESIAN_POINT('Ctrl Pts',(-0.0263997729668648,-0.148185337852268,
-0.479488955849035));
#48782=CARTESIAN_POINT('Ctrl Pts',(0.110295321529175,-0.102424530342436,
-0.471541664541082));
#48783=CARTESIAN_POINT('Ctrl Pts',(0.145829193847951,0.0372785271805361,
-0.463594373233131));
#48784=CARTESIAN_POINT('Ctrl Pts',(0.0476107068258777,0.14279027614874,
-0.455647081925179));
#48785=CARTESIAN_POINT('Ctrl Pts',(-0.0942756096603422,0.117336915718215,
-0.447699790617227));
#48786=CARTESIAN_POINT('Ctrl Pts',(-0.149693744518164,-0.0157361119474745,
-0.439752499309277));
#48787=CARTESIAN_POINT('Ctrl Pts',(-0.0678150118588708,-0.134376212677966,
-0.431805208001324));
#48788=CARTESIAN_POINT('Ctrl Pts',(0.0762626371868661,-0.129768457401624,
-0.423857916693373));
#48789=CARTESIAN_POINT('Ctrl Pts',(0.150393334019911,-0.00613901046328226,
-0.415910625385421));
#48790=CARTESIAN_POINT('Ctrl Pts',(0.0865855102898376,0.123121045215435,
-0.40796333407747));
#48791=CARTESIAN_POINT('Ctrl Pts',(-0.0566372507405924,0.139456316442247,
-0.400016042769518));
#48792=CARTESIAN_POINT('Ctrl Pts',(-0.147913170996249,0.027884336336504,
-0.392068751461567));
#48793=CARTESIAN_POINT('Ctrl Pts',(-0.103525339184802,-0.109262740738849,
-0.384121460153615));
#48794=CARTESIAN_POINT('Ctrl Pts',(0.0358143880747286,-0.146195663321201,
-0.376174168845663));
#48795=CARTESIAN_POINT('Ctrl Pts',(0.14230569330747,-0.0490401062332962,
-0.368226877537712));
#48796=CARTESIAN_POINT('Ctrl Pts',(0.118276341288589,0.0930943041140431,
-0.36027958622976));
#48797=CARTESIAN_POINT('Ctrl Pts',(-0.0142343050728087,0.149844008642945,
-0.352332294921809));
#48798=CARTESIAN_POINT('Ctrl Pts',(-0.133689459342201,0.069159025642954,
-0.344385003613857));
#48799=CARTESIAN_POINT('Ctrl Pts',(-0.13052663751097,-0.0749575831198715,
-0.336437712305905));
#48800=CARTESIAN_POINT('Ctrl Pts',(-0.00764673254121637,-0.150324215775555,
-0.328490420997954));
#48801=CARTESIAN_POINT('Ctrl Pts',(0.122246641348232,-0.087815722089899,
-0.320543129690002));
#48802=CARTESIAN_POINT('Ctrl Pts',(0.140017220957756,0.0552360407918496,
-0.312595838382051));
#48803=CARTESIAN_POINT('Ctrl Pts',(0.0293660959875197,0.14762613174348,
-0.304648547074098));
#48804=CARTESIAN_POINT('Ctrl Pts',(-0.108219173781323,0.104615738745118,
-0.296701255766147));
#48805=CARTESIAN_POINT('Ctrl Pts',(-0.14654743308991,-0.0343466478982285,
-0.288753964458195));
#48806=CARTESIAN_POINT('Ctrl Pts',(-0.0504645747484669,-0.141806801890957,
-0.280806673150244));
#48807=CARTESIAN_POINT('Ctrl Pts',(0.0919036381071333,-0.119203874390914,
-0.272859381842292));
#48808=CARTESIAN_POINT('Ctrl Pts',(0.149979206228629,0.0127310669651685,
-0.264912090534341));
#48809=CARTESIAN_POINT('Ctrl Pts',(0.0704960856148191,0.132989263777368,
-0.256964799226389));
#48810=CARTESIAN_POINT('Ctrl Pts',(-0.0736449922067076,0.131271693408073,
-0.249017507918438));
#48811=CARTESIAN_POINT('Ctrl Pts',(-0.150239982707076,0.00915368575314346,
-0.241070216610486));
#48812=CARTESIAN_POINT('Ctrl Pts',(-0.0890371041833558,-0.121359945804369,
-0.233122925302535));
#48813=CARTESIAN_POINT('Ctrl Pts',(0.0538292769655777,-0.140564047003862,
-0.225175633994583));
#48814=CARTESIAN_POINT('Ctrl Pts',(0.147324248946552,-0.0308449029238937,
-0.217228342686632));
#48815=CARTESIAN_POINT('Ctrl Pts',(0.105695619402189,0.107164725570485,
-0.209281051378679));
#48816=CARTESIAN_POINT('Ctrl Pts',(-0.0328754542608603,0.146884467812456,
-0.201333760070728));
#48817=CARTESIAN_POINT('Ctrl Pts',(-0.141293652002486,0.0518839690902201,
-0.193386468762776));
#48818=CARTESIAN_POINT('Ctrl Pts',(-0.120119421876057,-0.090703731257369,
-0.185439177454825));
#48819=CARTESIAN_POINT('Ctrl Pts',(0.0112265489861225,-0.150099323874037,
-0.177491886146873));
#48820=CARTESIAN_POINT('Ctrl Pts',(0.132275695981123,-0.0718260569698057,
-0.169544594838922));
#48821=CARTESIAN_POINT('Ctrl Pts',(0.132003550949032,0.0723249957317478,
-0.16159730353097));
#48822=CARTESIAN_POINT('Ctrl Pts',(0.0106597171159664,0.150140644601668,
-0.153650012223019));
#48823=CARTESIAN_POINT('Ctrl Pts',(-0.120461044964925,0.0902495312613209,
-0.145702720915067));
#48824=CARTESIAN_POINT('Ctrl Pts',(-0.141096744864573,-0.0524170959617924,
-0.137755429607115));
#48825=CARTESIAN_POINT('Ctrl Pts',(-0.032320598458173,-0.147007561970503,
-0.129808138299163));
#48826=CARTESIAN_POINT('Ctrl Pts',(0.106099483155384,-0.106764855471587,
-0.121860846991212));
#48827=CARTESIAN_POINT('Ctrl Pts',(0.147206769614965,0.0314009226223516,
-0.11391355568326));
#48828=CARTESIAN_POINT('Ctrl Pts',(0.05329807818182,0.140766356862578,-0.105966264375309));
#48829=CARTESIAN_POINT('Ctrl Pts',(-0.0894945744596918,0.121022774717712,
-0.0980189730673573));
#48830=CARTESIAN_POINT('Ctrl Pts',(-0.150204595788142,-0.00972068039065458,
-0.0900716817594055));
#48831=CARTESIAN_POINT('Ctrl Pts',(-0.0731483385023079,-0.131549249123061,
-0.0821243904514539));
#48832=CARTESIAN_POINT('Ctrl Pts',(0.0709968390897382,-0.132721336641146,
-0.0741770991435026));
#48833=CARTESIAN_POINT('Ctrl Pts',(0.150027895699077,-0.012166193515216,
-0.0662298078355508));
#48834=CARTESIAN_POINT('Ctrl Pts',(0.0914496844930611,0.119552911175019,
-0.0582825165275994));
#48835=CARTESIAN_POINT('Ctrl Pts',(-0.0509935714328428,0.1416097904161,
-0.0503352252196474));
#48836=CARTESIAN_POINT('Ctrl Pts',(-0.146687622928925,0.0338034202871001,
-0.042387933911696));
#48837=CARTESIAN_POINT('Ctrl Pts',(-0.10780145671892,-0.10504328737295,
-0.034440642603744));
#48838=CARTESIAN_POINT('Ctrl Pts',(0.0298815302181444,-0.147476681637548,
-0.0264933512957927));
#48839=CARTESIAN_POINT('Ctrl Pts',(0.140305210183422,-0.0547795936720048,
-0.018546059987841));
#48840=CARTESIAN_POINT('Ctrl Pts',(0.121751854094744,0.0884264404128374,
-0.0105987686798896));
#48841=CARTESIAN_POINT('Ctrl Pts',(0.0353672614029874,0.129422973420375,
-0.00530057447458853));
#48842=CARTESIAN_POINT('Ctrl Pts',(-0.00694716572162589,0.127110294187514,
-0.00265147737193801));
#48843=CARTESIAN_POINT('Ctrl Pts',(-0.111717694016322,0.037284145003949,
-2.93765));
#48844=CARTESIAN_POINT('Ctrl Pts',(-0.124129412884235,9.3843052402752E-5,
-2.93500090289735));
#48845=CARTESIAN_POINT('Ctrl Pts',(-0.108675196282194,-0.0870103938020027,
-2.92970270869205));
#48846=CARTESIAN_POINT('Ctrl Pts',(0.0145658909989512,-0.138586676302172,
-2.92175541738409));
#48847=CARTESIAN_POINT('Ctrl Pts',(0.12428129992797,-0.0627284744858215,
-2.91380812607615));
#48848=CARTESIAN_POINT('Ctrl Pts',(0.120090271076318,0.0704991524890691,
-2.9058608347682));
#48849=CARTESIAN_POINT('Ctrl Pts',(0.00571135947086689,0.139151690834859,
-2.89791354346024));
#48850=CARTESIAN_POINT('Ctrl Pts',(-0.113883405466689,0.0801313327482367,
-2.8899662521523));
#48851=CARTESIAN_POINT('Ctrl Pts',(-0.129037867514933,-0.0523605683294571,
-2.88201896084434));
#48852=CARTESIAN_POINT('Ctrl Pts',(-0.0258344786463291,-0.136840632652599,
-2.87407166953639));
#48853=CARTESIAN_POINT('Ctrl Pts',(0.101060618120367,-0.0958059291879449,
-2.86612437822844));
#48854=CARTESIAN_POINT('Ctrl Pts',(0.13526615819552,0.0330970741869585,
-2.85817708692048));
#48855=CARTESIAN_POINT('Ctrl Pts',(0.0454066843029653,0.131645762308753,
-2.85022979561253));
#48856=CARTESIAN_POINT('Ctrl Pts',(-0.0860986413824693,0.10944996017671,
-2.84228250430459));
#48857=CARTESIAN_POINT('Ctrl Pts',(-0.138635832133158,-0.0131312042072307,
-2.83433521299663));
#48858=CARTESIAN_POINT('Ctrl Pts',(-0.064018173970134,-0.123668891311378,
-2.82638792168868));
#48859=CARTESIAN_POINT('Ctrl Pts',(0.0693159272014078,-0.120779176949328,
-2.81844063038073));
#48860=CARTESIAN_POINT('Ctrl Pts',(0.139074531908459,-0.00711267889956292,
-2.81049333907277));
#48861=CARTESIAN_POINT('Ctrl Pts',(0.0812760328298283,0.113077501111085,
-2.80254604776482));
#48862=CARTESIAN_POINT('Ctrl Pts',(-0.0510676198065011,0.129554664787932,
-2.79459875645687));
#48863=CARTESIAN_POINT('Ctrl Pts',(-0.13657281942522,0.0272062350397427,
-2.78665146514892));
#48864=CARTESIAN_POINT('Ctrl Pts',(-0.0968154652687815,-0.100095353005703,
-2.77870417384097));
#48865=CARTESIAN_POINT('Ctrl Pts',(0.0317395866552255,-0.135590974706457,
-2.77075688253302));
#48866=CARTESIAN_POINT('Ctrl Pts',(0.131183564369451,-0.0467245803901248,
-2.76280959122507));
#48867=CARTESIAN_POINT('Ctrl Pts',(0.110307935021035,0.0849969022889005,
-2.75486229991711));
#48868=CARTESIAN_POINT('Ctrl Pts',(-0.0117404851910752,0.138760494767705,
-2.74691500860916));
#48869=CARTESIAN_POINT('Ctrl Pts',(-0.123020707789416,0.0652550333969683,
-2.73896771730121));
#48870=CARTESIAN_POINT('Ctrl Pts',(-0.12146817386388,-0.0681013704580597,
-2.73102042599325));
#48871=CARTESIAN_POINT('Ctrl Pts',(-0.00850684444458044,-0.138996214030495,
-2.72307313468531));
#48872=CARTESIAN_POINT('Ctrl Pts',(0.112256835707494,-0.0824058053669272,
-2.71512584337735));
#48873=CARTESIAN_POINT('Ctrl Pts',(0.130060222154785,0.0497659776633264,
-2.70717855206941));
#48874=CARTESIAN_POINT('Ctrl Pts',(0.02857431466928,0.136293148986501,-2.69923126076145));
#48875=CARTESIAN_POINT('Ctrl Pts',(-0.0991195276136302,0.0978142789458203,
-2.6912839694535));
#48876=CARTESIAN_POINT('Ctrl Pts',(-0.135902419040663,-0.0303783873615306,
-2.68333667814555));
#48877=CARTESIAN_POINT('Ctrl Pts',(-0.0480376407722225,-0.130708450334381,
-2.67538938683759));
#48878=CARTESIAN_POINT('Ctrl Pts',(0.0838865444021125,-0.111154674162296,
-2.66744209552965));
#48879=CARTESIAN_POINT('Ctrl Pts',(0.138871243492067,0.0103485095922432,
-2.65949480422169));
#48880=CARTESIAN_POINT('Ctrl Pts',(0.0664853114242254,0.122360194853714,
-2.65154751291374));
#48881=CARTESIAN_POINT('Ctrl Pts',(-0.0668799556441275,0.12214493625552,
-2.64360022160579));
#48882=CARTESIAN_POINT('Ctrl Pts',(-0.13890392592561,0.00990016576991218,
-2.63565293029784));
#48883=CARTESIAN_POINT('Ctrl Pts',(-0.0835272892091199,-0.111424888948546,
-2.62770563898989));
#48884=CARTESIAN_POINT('Ctrl Pts',(0.0484593300923006,-0.130552699117355,
-2.61975834768194));
#48885=CARTESIAN_POINT('Ctrl Pts',(0.135999775339708,-0.0299395228313577,
-2.61181105637398));
#48886=CARTESIAN_POINT('Ctrl Pts',(0.0988032571470193,0.0981337367930133,
-2.60386376506603));
#48887=CARTESIAN_POINT('Ctrl Pts',(-0.0290141333502425,0.136200198185447,
-2.59591647375808));
#48888=CARTESIAN_POINT('Ctrl Pts',(-0.130220193924971,0.0493458712960201,
-2.58796918245013));
#48889=CARTESIAN_POINT('Ctrl Pts',(-0.111990236842994,-0.082767752003245,
-2.58002189114218));
#48890=CARTESIAN_POINT('Ctrl Pts',(0.00895549343668939,-0.138968028902788,
-2.57207459983422));
#48891=CARTESIAN_POINT('Ctrl Pts',(0.121687378843393,-0.0677089045107432,
-2.56412730852628));
#48892=CARTESIAN_POINT('Ctrl Pts',(0.122809417189726,0.0656518161922446,
-2.55618001721832));
#48893=CARTESIAN_POINT('Ctrl Pts',(0.011292491656669,0.138797671277311,
-2.54823272591037));
#48894=CARTESIAN_POINT('Ctrl Pts',(-0.110581738624922,0.0846403745414082,
-2.54028543460242));
#48895=CARTESIAN_POINT('Ctrl Pts',(-0.131032049245288,-0.0471478100276249,
-2.53233814329447));
#48896=CARTESIAN_POINT('Ctrl Pts',(-0.0313017206303005,-0.135692727164734,
-2.52439085198651));
#48897=CARTESIAN_POINT('Ctrl Pts',(0.0971380788063926,-0.0997823008635477,
-2.51644356067857));
#48898=CARTESIAN_POINT('Ctrl Pts',(0.136484282651119,0.0276469620217102,
-2.50849626937061));
#48899=CARTESIAN_POINT('Ctrl Pts',(0.0506491401835047,0.129718844114848,
-2.50054897806267));
#48900=CARTESIAN_POINT('Ctrl Pts',(-0.0816406374595077,0.112814539111879,
-2.49260168675471));
#48901=CARTESIAN_POINT('Ctrl Pts',(-0.139050841334286,-0.00756157682283278,
-2.48465439544676));
#48902=CARTESIAN_POINT('Ctrl Pts',(-0.0689256895917136,-0.121002327391366,
-2.47670710413881));
#48903=CARTESIAN_POINT('Ctrl Pts',(0.0644170755712456,-0.123461549863384,
-2.46875981283085));
#48904=CARTESIAN_POINT('Ctrl Pts',(0.138677460778961,-0.0126836821041933,
-2.46081252152291));
#48905=CARTESIAN_POINT('Ctrl Pts',(0.0857449494400285,0.109727469511273,
-2.45286523021495));
#48906=CARTESIAN_POINT('Ctrl Pts',(-0.0458315493375432,0.131498224342159,
-2.444917938907));
#48907=CARTESIAN_POINT('Ctrl Pts',(-0.135372035336123,0.0326607710989214,
-2.43697064759905));
#48908=CARTESIAN_POINT('Ctrl Pts',(-0.10075131165362,-0.0961326537649701,
-2.4290233562911));
#48909=CARTESIAN_POINT('Ctrl Pts',(0.0262770108420999,-0.136754643873708,
-2.42107606498315));
#48910=CARTESIAN_POINT('Ctrl Pts',(0.129204451314017,-0.0519473163932888,
-2.41312877367519));
#48911=CARTESIAN_POINT('Ctrl Pts',(0.113627498086771,0.0805053141001346,
-2.40518148236725));
#48912=CARTESIAN_POINT('Ctrl Pts',(-0.00616689990636303,0.139119672459956,
-2.39723419105929));
#48913=CARTESIAN_POINT('Ctrl Pts',(-0.120305109378322,0.0701355443216227,
-2.38928689975134));
#48914=CARTESIAN_POINT('Ctrl Pts',(-0.124101268705739,-0.0631758579320174,
-2.38133960844339));
#48915=CARTESIAN_POINT('Ctrl Pts',(-0.0140735972308577,-0.138543306517508,
-2.37339231713544));
#48916=CARTESIAN_POINT('Ctrl Pts',(0.10886216750279,-0.086840902842008,
-2.36544502582749));
#48917=CARTESIAN_POINT('Ctrl Pts',(0.13195117753492,0.044510680369643,-2.35749773451953));
#48918=CARTESIAN_POINT('Ctrl Pts',(0.0340165375872002,0.135037732098843,
-2.34955044321158));
#48919=CARTESIAN_POINT('Ctrl Pts',(-0.0951175627623812,0.101710192084987,
-2.34160315190363));
#48920=CARTESIAN_POINT('Ctrl Pts',(-0.13701125466889,-0.0249044175574768,
-2.33365586059568));
#48921=CARTESIAN_POINT('Ctrl Pts',(-0.0532402693961469,-0.128677067243725,
-2.32570856928773));
#48922=CARTESIAN_POINT('Ctrl Pts',(0.0793618960797965,-0.114429032026143,
-2.31776127797978));
#48923=CARTESIAN_POINT('Ctrl Pts',(0.139174515358953,0.00477160291947143,
-2.30981398667182));
#48924=CARTESIAN_POINT('Ctrl Pts',(0.0713383470518088,0.11959579490825,
-2.30186669536388));
#48925=CARTESIAN_POINT('Ctrl Pts',(-0.0619282880767048,0.124728509394241,
-2.29391940405591));
#48926=CARTESIAN_POINT('Ctrl Pts',(-0.138395221981915,0.0154620972832579,
-2.28597211274797));
#48927=CARTESIAN_POINT('Ctrl Pts',(-0.0879281245512522,-0.107985919603993,
-2.27802482144002));
#48928=CARTESIAN_POINT('Ctrl Pts',(0.0431853359348615,-0.132390863279962,
-2.27007753013206));
#48929=CARTESIAN_POINT('Ctrl Pts',(0.134689851066473,-0.0353688837753169,
-2.26213023882412));
#48930=CARTESIAN_POINT('Ctrl Pts',(0.102658845743989,0.0940929078641549,
-2.25418294751616));
#48931=CARTESIAN_POINT('Ctrl Pts',(-0.0235293201795658,0.137254089234922,
-2.24623565620821));
#48932=CARTESIAN_POINT('Ctrl Pts',(-0.128136744931471,0.0545278691880376,
-2.23828836490026));
#48933=CARTESIAN_POINT('Ctrl Pts',(-0.115219060337234,-0.0782104983670698,
-2.23034107359231));
#48934=CARTESIAN_POINT('Ctrl Pts',(0.00337582615670157,-0.139215364516925,
-2.22239378228436));
#48935=CARTESIAN_POINT('Ctrl Pts',(0.118874455301411,-0.0725339768426726,
-2.21444649097641));
#48936=CARTESIAN_POINT('Ctrl Pts',(0.125343208860993,0.0606744914461575,
-2.20649919966845));
#48937=CARTESIAN_POINT('Ctrl Pts',(0.0168490426502724,0.138233222061811,
-2.19855190836051));
#48938=CARTESIAN_POINT('Ctrl Pts',(-0.107098813919995,0.0890065052496212,
-2.19060461705255));
#48939=CARTESIAN_POINT('Ctrl Pts',(-0.132817237367694,-0.0418556492941425,
-2.1826573257446));
#48940=CARTESIAN_POINT('Ctrl Pts',(-0.0367176736873534,-0.134328427217807,
-2.17471003443665));
#48941=CARTESIAN_POINT('Ctrl Pts',(0.093058792097453,-0.103597177245249,
-2.16676274312869));
#48942=CARTESIAN_POINT('Ctrl Pts',(0.137483123155237,0.022151856971875,
-2.15881545182074));
#48943=CARTESIAN_POINT('Ctrl Pts',(0.0558099863031745,0.127583538705665,
-2.1508681605128));
#48944=CARTESIAN_POINT('Ctrl Pts',(-0.0770512367328716,0.115997503584152,
-2.14292086920484));
#48945=CARTESIAN_POINT('Ctrl Pts',(-0.139242215826564,-0.00197970996083189,
-2.13497357789689));
#48946=CARTESIAN_POINT('Ctrl Pts',(-0.0737223134758439,-0.118141163087173,
-2.12702628658893));
#48947=CARTESIAN_POINT('Ctrl Pts',(0.0594145941073171,-0.125945305299099,
-2.11907899528099));
#48948=CARTESIAN_POINT('Ctrl Pts',(0.138057323045987,-0.0182342938771007,
-2.11113170397303));
#48949=CARTESIAN_POINT('Ctrl Pts',(0.0900759365079238,0.106200939647636,
-2.10318441266508));
#48950=CARTESIAN_POINT('Ctrl Pts',(-0.0405217541450246,0.133230256926986,
-2.09523712135713));
#48951=CARTESIAN_POINT('Ctrl Pts',(-0.133953496893346,0.0380627717049713,
-2.08728983004918));
#48952=CARTESIAN_POINT('Ctrl Pts',(-0.104525092241263,-0.0920153194407107,
-2.07934253874123));
#48953=CARTESIAN_POINT('Ctrl Pts',(0.0207721664357911,-0.137698333400896,
-2.07139524743328));
#48954=CARTESIAN_POINT('Ctrl Pts',(0.127017504190175,-0.0570864918270448,
-2.06344795612532));
#48955=CARTESIAN_POINT('Ctrl Pts',(0.116764283495866,0.0758842277388233,
-2.05550066481737));
#48956=CARTESIAN_POINT('Ctrl Pts',(-0.000583394708775192,0.139255066588021,
-2.04755337350942));
#48957=CARTESIAN_POINT('Ctrl Pts',(-0.117395991996717,0.0749032374662622,
-2.03960608220147));
#48958=CARTESIAN_POINT('Ctrl Pts',(-0.12653473816887,-0.058148722740537,
-2.03165879089352));
#48959=CARTESIAN_POINT('Ctrl Pts',(-0.0196177116792869,-0.137867542620766,
-2.02371149958557));
#48960=CARTESIAN_POINT('Ctrl Pts',(0.105292387066522,-0.0911363107968193,
-2.01576420827761));
#48961=CARTESIAN_POINT('Ctrl Pts',(0.133629880429484,0.039183784608208,
-2.00781691696966));
#48962=CARTESIAN_POINT('Ctrl Pts',(0.0394040425810417,0.133565097791645,
-1.99986962566171));
#48963=CARTESIAN_POINT('Ctrl Pts',(-0.0909625948131785,0.105442497431889,
-1.99192233435376));
#48964=CARTESIAN_POINT('Ctrl Pts',(-0.137899698332905,-0.019390387296652,
-1.98397504304581));
#48965=CARTESIAN_POINT('Ctrl Pts',(-0.058357257409372,-0.126438698298729,
-1.97602775173786));
#48966=CARTESIAN_POINT('Ctrl Pts',(0.0747095887255279,-0.117519322974067,
-1.9680804604299));
#48967=CARTESIAN_POINT('Ctrl Pts',(0.139253915509176,-0.000812979202544665,
-1.96013316912196));
#48968=CARTESIAN_POINT('Ctrl Pts',(0.0760766300741984,0.116639016955623,
-1.952185877814));
#48969=CARTESIAN_POINT('Ctrl Pts',(-0.0568770046268523,0.127111448203918,
-1.94423858650605));
#48970=CARTESIAN_POINT('Ctrl Pts',(-0.137663899868222,0.0209991569567163,
-1.9362912951981));
#48971=CARTESIAN_POINT('Ctrl Pts',(-0.0921875214976232,-0.104373247529939,
-1.92834400389015));
#48972=CARTESIAN_POINT('Ctrl Pts',(0.037841875214064,-0.134016067693779,
-1.92039671258219));
#48973=CARTESIAN_POINT('Ctrl Pts',(0.133163268965518,-0.0407413514532521,
-1.91244942127425));
#48974=CARTESIAN_POINT('Ctrl Pts',(0.106349300573725,0.0899007240643813,
-1.90450212996629));
#48975=CARTESIAN_POINT('Ctrl Pts',(-0.0180066584898106,0.138087197704393,
-1.89655483865834));
#48976=CARTESIAN_POINT('Ctrl Pts',(-0.125847179229191,0.0596221552770135,
-1.88860754735039));
#48977=CARTESIAN_POINT('Ctrl Pts',(-0.118262546100927,-0.0735274378007737,
-1.88066025604244));
#48978=CARTESIAN_POINT('Ctrl Pts',(-0.00220927137030462,-0.139238762705767,
-1.87271296473448));
#48979=CARTESIAN_POINT('Ctrl Pts',(0.115870314076337,-0.077242373317187,
-1.86476567342653));
#48980=CARTESIAN_POINT('Ctrl Pts',(0.127675377417112,0.0555995676351779,
-1.85681838211858));
#48981=CARTESIAN_POINT('Ctrl Pts',(0.0223784908076123,0.137446415264255,
-1.84887109081063));
#48982=CARTESIAN_POINT('Ctrl Pts',(-0.103443613455673,0.0932294629130393,
-1.84092379950268));
#48983=CARTESIAN_POINT('Ctrl Pts',(-0.134388779889457,-0.0364961608891077,
-1.83297650819473));
#48984=CARTESIAN_POINT('Ctrl Pts',(-0.0420745638576578,-0.132748050818114,
-1.82502921688678));
#48985=CARTESIAN_POINT('Ctrl Pts',(0.0888298139634637,-0.107245410489387,
-1.81708192557882));
#48986=CARTESIAN_POINT('Ctrl Pts',(0.13826081266264,0.0166211191466418,
-1.80913463427087));
#48987=CARTESIAN_POINT('Ctrl Pts',(0.0608810582468267,0.125243006457714,
-1.80118734296292));
#48988=CARTESIAN_POINT('Ctrl Pts',(-0.072337893827657,0.118993878146731,
-1.79324005165497));
#48989=CARTESIAN_POINT('Ctrl Pts',(-0.139209609701381,0.00360534139989891,
-1.78529276034702));
#48990=CARTESIAN_POINT('Ctrl Pts',(-0.078400349981893,-0.115089960650516,
-1.77734546903907));
#48991=CARTESIAN_POINT('Ctrl Pts',(0.054316540209444,-0.128226469106407,
-1.76939817773111));
#48992=CARTESIAN_POINT('Ctrl Pts',(0.137215110676543,-0.0237555745425038,
-1.76145088642316));
#48993=CARTESIAN_POINT('Ctrl Pts',(0.0942620302777797,0.102503578316717,
-1.75350359511521));
#48994=CARTESIAN_POINT('Ctrl Pts',(-0.0351467769424353,0.13474797954099,
-1.74555630380726));
#48995=CARTESIAN_POINT('Ctrl Pts',(-0.132319485098849,0.0434035457422106,
-1.73760901249931));
#48996=CARTESIAN_POINT('Ctrl Pts',(-0.108130737076674,-0.0877499721884613,
-1.72966172119136));
#48997=CARTESIAN_POINT('Ctrl Pts',(0.0152339085805741,-0.138420525750985,
-1.72171442988341));
#48998=CARTESIAN_POINT('Ctrl Pts',(0.124626240732756,-0.062133839738435,
-1.71376713857545));
#48999=CARTESIAN_POINT('Ctrl Pts',(0.11971324557739,0.0711410764126323,
-1.7058198472675));
#49000=CARTESIAN_POINT('Ctrl Pts',(0.00500104891906081,0.139166459427298,
-1.69787255595955));
#49001=CARTESIAN_POINT('Ctrl Pts',(-0.114298035141258,0.0795504436358992,
-1.6899252646516));
#49002=CARTESIAN_POINT('Ctrl Pts',(-0.128764667860552,-0.0530280513556949,
-1.68197797334364));
#49003=CARTESIAN_POINT('Ctrl Pts',(-0.0251302696981556,-0.136970009362336,
-1.6740306820357));
#49004=CARTESIAN_POINT('Ctrl Pts',(0.101553236631872,-0.0952851197690979,
-1.66608339072774));
#49005=CARTESIAN_POINT('Ctrl Pts',(0.135093630531518,0.0337938590521173,
-1.65813609941979));
#49006=CARTESIAN_POINT('Ctrl Pts',(0.0447281634802288,0.131877614899218,
-1.65018880811184));
#49007=CARTESIAN_POINT('Ctrl Pts',(-0.0866613073154762,0.109005191317629,
-1.64224151680389));
#49008=CARTESIAN_POINT('Ctrl Pts',(-0.138566320910571,-0.0138451662730742,
-1.63429422549594));
#49009=CARTESIAN_POINT('Ctrl Pts',(-0.0633803737869685,-0.123996944068975,
-1.62634693418799));
#49010=CARTESIAN_POINT('Ctrl Pts',(0.0699371058934867,-0.120420576061834,
-1.61839964288003));
#49011=CARTESIAN_POINT('Ctrl Pts',(0.139109316222199,-0.00639625359196896,
-1.61045235157208));
#49012=CARTESIAN_POINT('Ctrl Pts',(0.0806925386394054,0.113494617175214,
-1.60250506026413));
#49013=CARTESIAN_POINT('Ctrl Pts',(-0.051734230629111,0.129289919564653,
-1.59455776895618));
#49014=CARTESIAN_POINT('Ctrl Pts',(-0.136711135966119,0.0265024380515037,
-1.58661047764823));
#49015=CARTESIAN_POINT('Ctrl Pts',(-0.0962986285172303,-0.100592683956246,
-1.57866318634028));
#49016=CARTESIAN_POINT('Ctrl Pts',(0.0324375432515528,-0.135425698106468,
-1.57071589503233));
#49017=CARTESIAN_POINT('Ctrl Pts',(0.131422484648456,-0.0460482838838423,
-1.56276860372437));
#49018=CARTESIAN_POINT('Ctrl Pts',(0.109868685287492,0.0855639288077546,
-1.55482131241642));
#49019=CARTESIAN_POINT('Ctrl Pts',(-0.0124550318596216,0.138698183481963,
-1.54687402110847));
#49020=CARTESIAN_POINT('Ctrl Pts',(-0.123355179740992,0.0646205350557252,
-1.53892672980052));
#49021=CARTESIAN_POINT('Ctrl Pts',(-0.121115798479285,-0.0687261033272357,
-1.53097943849257));
#49022=CARTESIAN_POINT('Ctrl Pts',(-0.00779081513336725,-0.139038185831728,
-1.52303214718461));
#49023=CARTESIAN_POINT('Ctrl Pts',(0.112679787534581,-0.0818265201568669,
-1.51508485587666));
#49024=CARTESIAN_POINT('Ctrl Pts',(0.129802171405619,0.0504352081209822,
-1.50713756456871));
#49025=CARTESIAN_POINT('Ctrl Pts',(0.0278719416335478,0.136438516517136,
-1.49919027326076));
#49026=CARTESIAN_POINT('Ctrl Pts',(-0.0996220168716355,0.0973024546157401,
-1.49124298195281));
#49027=CARTESIAN_POINT('Ctrl Pts',(-0.135744148877059,-0.0310779659157952,
-1.48329569064486));
#49028=CARTESIAN_POINT('Ctrl Pts',(-0.0473637742173777,-0.130954140109069,
-1.47534839933691));
#49029=CARTESIAN_POINT('Ctrl Pts',(0.0844579470046824,-0.110721132163533,
-1.46740110802895));
#49030=CARTESIAN_POINT('Ctrl Pts',(0.138816100206623,0.0110636451156712,
-1.459453816721));
#49031=CARTESIAN_POINT('Ctrl Pts',(0.0658541988487744,0.122701012277025,
-1.45150652541305));
#49032=CARTESIAN_POINT('Ctrl Pts',(-0.0675081904779539,0.121798842926412,
-1.4435592341051));
#49033=CARTESIAN_POINT('Ctrl Pts',(-0.138953075407915,0.00918459332266326,
-1.43561194279715));
#49034=CARTESIAN_POINT('Ctrl Pts',(-0.0829522741685301,-0.111853628148976,
-1.4276646514892));
#49035=CARTESIAN_POINT('Ctrl Pts',(0.0491311144456285,-0.130301371877472,
-1.41971736018124));
#49036=CARTESIAN_POINT('Ctrl Pts',(0.136152178426768,-0.0292386427432272,
-1.41177006887329));
#49037=CARTESIAN_POINT('Ctrl Pts',(0.0982964971317635,0.0986413329768289,
-1.40382277756534));
#49038=CARTESIAN_POINT('Ctrl Pts',(-0.0297152637478395,0.136048950823653,
-1.39587548625739));
#49039=CARTESIAN_POINT('Ctrl Pts',(-0.130472628372239,0.0486745022107058,
-1.38792819494944));
#49040=CARTESIAN_POINT('Ctrl Pts',(-0.111562446233792,-0.0833434731106928,
-1.37998090364148));
#49041=CARTESIAN_POINT('Ctrl Pts',(0.00967114594259312,-0.13892005922824,
-1.37203361233354));
#49042=CARTESIAN_POINT('Ctrl Pts',(0.122034507452407,-0.0670812411234985,
-1.36408632102558));
#49043=CARTESIAN_POINT('Ctrl Pts',(0.122469640724355,0.0662834898045348,
-1.35613902971763));
#49044=CARTESIAN_POINT('Ctrl Pts',(0.0105774480180276,0.138853993508456,
-1.34819173840968));
#49045=CARTESIAN_POINT('Ctrl Pts',(-0.111016222087204,0.0840696874819043,
-1.34024444710173));
#49046=CARTESIAN_POINT('Ctrl Pts',(-0.130787470786524,-0.0478220807272631,
-1.33229715579378));
#49047=CARTESIAN_POINT('Ctrl Pts',(-0.0306024039612664,-0.135852150485784,
-1.32434986448582));
#49048=CARTESIAN_POINT('Ctrl Pts',(0.097650730877784,-0.0992806561161591,
-1.31640257317787));
#49049=CARTESIAN_POINT('Ctrl Pts',(0.136340073298976,0.0283495737648783,
-1.30845528186992));
#49050=CARTESIAN_POINT('Ctrl Pts',(0.0499803360725424,0.129977997853083,
-1.30050799056197));
#49051=CARTESIAN_POINT('Ctrl Pts',(-0.0822206191840827,0.112392542905687,
-1.29256069925402));
#49052=CARTESIAN_POINT('Ctrl Pts',(-0.139010050093927,-0.00827767435361591,
-1.28461340794607));
#49053=CARTESIAN_POINT('Ctrl Pts',(-0.0683015385030549,-0.121355732282971,
-1.27666611663811));
#49054=CARTESIAN_POINT('Ctrl Pts',(0.0650521244483742,-0.123128124425631,
-1.26871882533016));
#49055=CARTESIAN_POINT('Ctrl Pts',(0.138740950095853,-0.0119692391704875,
-1.26077153402221));
#49056=CARTESIAN_POINT('Ctrl Pts',(0.0851786477431396,0.110167653548901,
-1.25282424271426));
#49057=CARTESIAN_POINT('Ctrl Pts',(-0.0465082385868169,0.131260419256424,
-1.24487695140631));
#49058=CARTESIAN_POINT('Ctrl Pts',(-0.135538462861439,0.0319630881639851,
-1.23692966009836));
#49059=CARTESIAN_POINT('Ctrl Pts',(-0.100254832613553,-0.0966503101777165,
-1.22898236879041));
#49060=CARTESIAN_POINT('Ctrl Pts',(0.0269810332845223,-0.136617487031199,
-1.22103507748245));
#49061=CARTESIAN_POINT('Ctrl Pts',(0.12947029828579,-0.0512811445036981,
-1.2130877861745));
#49062=CARTESIAN_POINT('Ctrl Pts',(0.113211338714528,0.0810894981257437,
-1.20514049486655));
#49063=CARTESIAN_POINT('Ctrl Pts',(-0.00688337045973726,0.139086063755268,
-1.1971932035586));
#49064=CARTESIAN_POINT('Ctrl Pts',(-0.120664755018308,0.0695149682887939,
-1.18924591225065));
#49065=CARTESIAN_POINT('Ctrl Pts',(-0.123774227820918,-0.0638142182209893,
-1.18129862094269));
#49066=CARTESIAN_POINT('Ctrl Pts',(-0.0133598268380069,-0.138613956536415,
-1.17335132963475));
#49067=CARTESIAN_POINT('Ctrl Pts',(0.10930800785607,-0.0862790434483248,
-1.16540403832679));
#49068=CARTESIAN_POINT('Ctrl Pts',(0.131720169733078,0.0451897201286931,
-1.15745674701884));
#49069=CARTESIAN_POINT('Ctrl Pts',(0.0333205585370974,0.135211147094447,
-1.14950945571089));
#49070=CARTESIAN_POINT('Ctrl Pts',(-0.0956401714670842,0.101218928672295,
-1.14156216440294));
#49071=CARTESIAN_POINT('Ctrl Pts',(-0.136881164126884,-0.0256097799109962,
-1.13361487309499));
#49072=CARTESIAN_POINT('Ctrl Pts',(-0.0525767967102828,-0.128949580718614,
-1.12566758178704));
#49073=CARTESIAN_POINT('Ctrl Pts',(0.0799502236678128,-0.114018751331906,
-1.11772029047908));
#49074=CARTESIAN_POINT('Ctrl Pts',(0.13914809256923,0.00548837445564355,
-1.10977299917113));
#49075=CARTESIAN_POINT('Ctrl Pts',(0.0707214084725853,0.11996164513491,
-1.10182570786318));
#49076=CARTESIAN_POINT('Ctrl Pts',(-0.0625698955915714,0.124407885945709,
-1.09387841655523));
#49077=CARTESIAN_POINT('Ctrl Pts',(-0.138473025599107,0.0147490711995586,
-1.08593112524728));
#49078=CARTESIAN_POINT('Ctrl Pts',(-0.0873707639547012,-0.108437371444499,
-1.07798383393932));
#49079=CARTESIAN_POINT('Ctrl Pts',(0.043866657927493,-0.132166675989422,
-1.07003654263137));
#49080=CARTESIAN_POINT('Ctrl Pts',(0.134870236095805,-0.0346746785894572,
-1.06208925132342));
#49081=CARTESIAN_POINT('Ctrl Pts',(0.102172847354302,0.0946204163134727,
-1.05414196001547));
#49082=CARTESIAN_POINT('Ctrl Pts',(-0.0242359515212969,0.137131078073783,
-1.04619466870752));
#49083=CARTESIAN_POINT('Ctrl Pts',(-0.128415897508745,0.0538671624168572,
-1.03824737739957));
#49084=CARTESIAN_POINT('Ctrl Pts',(-0.114814699573973,-0.078802910362236,
-1.03030008609162));
#49085=CARTESIAN_POINT('Ctrl Pts',(0.00409282660561049,-0.13919613029893,
-1.02235279478367));
#49086=CARTESIAN_POINT('Ctrl Pts',(0.119246473329177,-0.0719207377490957,
-1.01440550347571));
#49087=CARTESIAN_POINT('Ctrl Pts',(0.12502903508685,0.0613192816744626,
-1.00645821216776));
#49088=CARTESIAN_POINT('Ctrl Pts',(0.0161368325691865,0.138318171454277,
-0.998510920859808));
#49089=CARTESIAN_POINT('Ctrl Pts',(-0.107555831855076,0.0884536994917849,
-0.990563629551857));
#49090=CARTESIAN_POINT('Ctrl Pts',(-0.132599893130074,-0.0425391850146832,
-0.982616338243906));
#49091=CARTESIAN_POINT('Ctrl Pts',(-0.0360253121667897,-0.134515764143485,
-0.974669046935953));
#49092=CARTESIAN_POINT('Ctrl Pts',(0.0935911472513838,-0.103116492744809,
-0.966721755628004));
#49093=CARTESIAN_POINT('Ctrl Pts',(0.13736720374351,0.0228596862513367,
-0.958774464320049));
#49094=CARTESIAN_POINT('Ctrl Pts',(0.0551521118795285,0.127869302317047,
-0.950827173012101));
#49095=CARTESIAN_POINT('Ctrl Pts',(-0.077647673569253,0.115599103409599,
-0.942879881704147));
#49096=CARTESIAN_POINT('Ctrl Pts',(-0.139230172114263,-0.00269686722940675,
-0.934932590396197));
#49097=CARTESIAN_POINT('Ctrl Pts',(-0.0731128355279682,-0.118519311510323,
-0.926985299088244));
#49098=CARTESIAN_POINT('Ctrl Pts',(0.0600625022165961,-0.125637612788934,
-0.919038007780293));
#49099=CARTESIAN_POINT('Ctrl Pts',(0.138149409672222,-0.0175229714100354,
-0.911090716472342));
#49100=CARTESIAN_POINT('Ctrl Pts',(0.0895277411724023,0.106663477724982,
-0.903143425164389));
#49101=CARTESIAN_POINT('Ctrl Pts',(-0.0412074348652185,0.133019777595849,
-0.895196133856439));
#49102=CARTESIAN_POINT('Ctrl Pts',(-0.134147766878989,0.0373723234653771,
-0.887248842548486));
#49103=CARTESIAN_POINT('Ctrl Pts',(-0.104049769962011,-0.0925524677719242,
-0.879301551240536));
#49104=CARTESIAN_POINT('Ctrl Pts',(0.0214811224820551,-0.137589517394064,
-0.871354259932582));
#49105=CARTESIAN_POINT('Ctrl Pts',(0.127309850102664,-0.0564315158989901,
-0.863406968624633));
#49106=CARTESIAN_POINT('Ctrl Pts',(0.116371883968419,0.0764846294458023,
-0.855459677316679));
#49107=CARTESIAN_POINT('Ctrl Pts',(-0.0013006366881828,0.139250214592387,
-0.847512386008729));
#49108=CARTESIAN_POINT('Ctrl Pts',(-0.117780232793124,0.074297581945969,
-0.839565094700777));
#49109=CARTESIAN_POINT('Ctrl Pts',(-0.126233557860599,-0.0587996835848236,
-0.831617803392825));
#49110=CARTESIAN_POINT('Ctrl Pts',(-0.0189073483484057,-0.137966757221631,
-0.823670512084875));
#49111=CARTESIAN_POINT('Ctrl Pts',(0.105760398778781,-0.0905927810036414,
-0.81572322077692));
#49112=CARTESIAN_POINT('Ctrl Pts',(0.133426287168139,0.0398715413841222,
-0.807775929468972));
#49113=CARTESIAN_POINT('Ctrl Pts',(0.038715577045716,0.133766281303764,
-0.799828638161018));
#49114=CARTESIAN_POINT('Ctrl Pts',(-0.0915044823124013,0.104972585166604,
-0.791881346853068));
#49115=CARTESIAN_POINT('Ctrl Pts',(-0.137797996672218,-0.0201003988254995,
-0.783934055545116));
#49116=CARTESIAN_POINT('Ctrl Pts',(-0.0577052458335282,-0.126737597117481,
-0.775986764237163));
#49117=CARTESIAN_POINT('Ctrl Pts',(0.0753138949338155,-0.117132963548775,
-0.768039472929213));
#49118=CARTESIAN_POINT('Ctrl Pts',(0.139256255718067,-9.57246296715326E-5,
-0.760092181621259));
#49119=CARTESIAN_POINT('Ctrl Pts',(0.075474857879039,0.117029311490581,
-0.75214489031331));
#49120=CARTESIAN_POINT('Ctrl Pts',(-0.0575309527532313,0.126816810380666,
-0.744197599005357));
#49121=CARTESIAN_POINT('Ctrl Pts',(-0.13777023246787,0.0202898241877454,
-0.736250307697407));
#49122=CARTESIAN_POINT('Ctrl Pts',(-0.0916487118977105,-0.104846685819395,
-0.728303016389454));
#49123=CARTESIAN_POINT('Ctrl Pts',(0.0385316388930217,-0.133819380973154,
-0.720355725081504));
#49124=CARTESIAN_POINT('Ctrl Pts',(0.13337134577548,-0.0400549378461348,
-0.712408433773551));
#49125=CARTESIAN_POINT('Ctrl Pts',(0.105884845571219,0.0904472962458246,
-0.7044611424656));
#49126=CARTESIAN_POINT('Ctrl Pts',(-0.018717654110887,0.137992620615763,
-0.696513851157648));
#49127=CARTESIAN_POINT('Ctrl Pts',(-0.126152600900479,0.058973173611947,
-0.688566559849696));
#49128=CARTESIAN_POINT('Ctrl Pts',(-0.117882265625521,-0.0741355877484928,
-0.680619268541745));
#49129=CARTESIAN_POINT('Ctrl Pts',(-0.00149207632259066,-0.13924829488388,
-0.672671977233793));
#49130=CARTESIAN_POINT('Ctrl Pts',(0.116266623106448,-0.0766445449542468,
-0.664724685925842));
#49131=CARTESIAN_POINT('Ctrl Pts',(0.12738731170417,0.0562564372903673,
-0.65677739461789));
#49132=CARTESIAN_POINT('Ctrl Pts',(0.0216702599226566,0.13755985517114,
-0.648830103309939));
#49133=CARTESIAN_POINT('Ctrl Pts',(-0.103922430718979,0.0926954276827039,
-0.640882812001986));
#49134=CARTESIAN_POINT('Ctrl Pts',(-0.134199019486038,-0.0371878621166431,
-0.632935520694035));
#49135=CARTESIAN_POINT('Ctrl Pts',(-0.0413902711963712,-0.13296300000418,
-0.624988229386083));
#49136=CARTESIAN_POINT('Ctrl Pts',(0.0893810158703018,-0.106786459449753,
-0.617040938078132));
#49137=CARTESIAN_POINT('Ctrl Pts',(0.138173369655621,0.0173330273706489,
-0.60909364677018));
#49138=CARTESIAN_POINT('Ctrl Pts',(0.0602351717464476,0.125554920271953,
-0.60114635546223));
#49139=CARTESIAN_POINT('Ctrl Pts',(-0.072949826366452,0.118619714857712,
-0.593199064154276));
#49140=CARTESIAN_POINT('Ctrl Pts',(-0.139226332890273,0.00288827798998521,
-0.585251772846326));
#49141=CARTESIAN_POINT('Ctrl Pts',(-0.0778065255617132,-0.115492244327638,
-0.577304481538374));
#49142=CARTESIAN_POINT('Ctrl Pts',(0.0549762653464128,-0.127945004468253,
-0.569357190230422));
#49143=CARTESIAN_POINT('Ctrl Pts',(0.137335646484491,-0.02304851675287,
-0.561409898922471));
#49144=CARTESIAN_POINT('Ctrl Pts',(0.0937328231132788,0.102987726409681,
-0.553462607614519));
#49145=CARTESIAN_POINT('Ctrl Pts',(-0.0358403461692648,0.134565164534837,
-0.545515316306567));
#49146=CARTESIAN_POINT('Ctrl Pts',(-0.132541285048275,0.0427214428311217,
-0.537568024998616));
#49147=CARTESIAN_POINT('Ctrl Pts',(-0.107677336146595,-0.0883057483983573,
-0.529620733690664));
#49148=CARTESIAN_POINT('Ctrl Pts',(0.0159466578264506,-0.13834022561781,
-0.521673442382713));
#49149=CARTESIAN_POINT('Ctrl Pts',(0.124944615327587,-0.0614911133454406,
-0.513726151074761));
#49150=CARTESIAN_POINT('Ctrl Pts',(0.119345237096187,0.071756730013814,
-0.50577885976681));
#49151=CARTESIAN_POINT('Ctrl Pts',(0.00428418924635087,0.139190371945483,
-0.497831568458857));
#49152=CARTESIAN_POINT('Ctrl Pts',(-0.11470625301651,0.0789606828664291,
-0.489884277150907));
#49153=CARTESIAN_POINT('Ctrl Pts',(-0.128489832597935,-0.053690565640297,
-0.481936985842954));
#49154=CARTESIAN_POINT('Ctrl Pts',(-0.0244244560972015,-0.137097628951694,
-0.473989694535004));
#49155=CARTESIAN_POINT('Ctrl Pts',(0.102042666874295,-0.0947607938812361,
-0.466042403227051));
#49156=CARTESIAN_POINT('Ctrl Pts',(0.134917779304342,0.0344892265411343,
-0.4580951119191));
#49157=CARTESIAN_POINT('Ctrl Pts',(0.0440483189035268,0.132106243310428,
-0.450147820611148));
#49158=CARTESIAN_POINT('Ctrl Pts',(-0.0872216019461573,0.108557386085731,
-0.442200529303197));
#49159=CARTESIAN_POINT('Ctrl Pts',(-0.13849317172527,-0.0145586848751967,
-0.434253237995245));
#49160=CARTESIAN_POINT('Ctrl Pts',(-0.0627408721263131,-0.124321747432419,
-0.426305946687293));
#49161=CARTESIAN_POINT('Ctrl Pts',(0.0705564186542189,-0.120058759391021,
-0.418358655379342));
#49162=CARTESIAN_POINT('Ctrl Pts',(0.139140415665318,-0.0056796697353837,
-0.41041136407139));
#49163=CARTESIAN_POINT('Ctrl Pts',(0.0801069008200053,0.113908728203041,
-0.402464072763439));
#49164=CARTESIAN_POINT('Ctrl Pts',(-0.0523994674467565,0.129021741311752,
-0.394516781455487));
#49165=CARTESIAN_POINT('Ctrl Pts',(-0.136845826504972,0.0257979396074864,
-0.386569490147535));
#49166=CARTESIAN_POINT('Ctrl Pts',(-0.0957792366260094,-0.101087347136819,
-0.378622198839584));
#49167=CARTESIAN_POINT('Ctrl Pts',(0.0331346390848385,-0.135256828339786,
-0.370674907531632));
#49168=CARTESIAN_POINT('Ctrl Pts',(0.131657918533283,-0.0453707659986463,
-0.362727616223681));
#49169=CARTESIAN_POINT('Ctrl Pts',(0.109426520779767,0.086128685522627,
-0.354780324915729));
#49170=CARTESIAN_POINT('Ctrl Pts',(-0.0131692480750101,0.138632192599552,
-0.346833033607777));
#49171=CARTESIAN_POINT('Ctrl Pts',(-0.123686379214668,0.0639843224281227,
-0.338885742299826));
#49172=CARTESIAN_POINT('Ctrl Pts',(-0.120760209998862,-0.0693490129767615,
-0.330938450991875));
#49173=CARTESIAN_POINT('Ctrl Pts',(-0.00707457914409293,-0.139076469072788,
-0.322991159683922));
#49174=CARTESIAN_POINT('Ctrl Pts',(0.113099750076884,-0.08124506417234,
-0.315043868375971));
#49175=CARTESIAN_POINT('Ctrl Pts',(0.12954067712726,0.0511031005833377,
-0.307096577068019));
#49176=CARTESIAN_POINT('Ctrl Pts',(0.0271688291824932,0.136580264462594,
-0.299149285760068));
#49177=CARTESIAN_POINT('Ctrl Pts',(-0.100121863252902,0.0967880489450682,
-0.291201994452116));
#49178=CARTESIAN_POINT('Ctrl Pts',(-0.135582277550388,-0.0317767200016701,
-0.283254703144164));
#49179=CARTESIAN_POINT('Ctrl Pts',(-0.0466886511469119,-0.131196355795028,
-0.275307411836213));
#49180=CARTESIAN_POINT('Ctrl Pts',(0.0850271090185907,-0.11028465283889,
-0.267360120528261));
#49181=CARTESIAN_POINT('Ctrl Pts',(0.138757274262191,0.0117784871313546,
-0.25941282922031));
#49182=CARTESIAN_POINT('Ctrl Pts',(0.0652213392245596,0.123038574559143,
-0.251465537912358));
#49183=CARTESIAN_POINT('Ctrl Pts',(-0.0681346343844765,0.121449518390703,
-0.243518246604407));
#49184=CARTESIAN_POINT('Ctrl Pts',(-0.138998538596432,0.00846877721585035,
-0.235570955296455));
#49185=CARTESIAN_POINT('Ctrl Pts',(-0.082375058485434,-0.112279399977289,
-0.227623663988504));
#49186=CARTESIAN_POINT('Ctrl Pts',(0.0498015954015689,-0.130046587870231,
-0.219676372680552));
#49187=CARTESIAN_POINT('Ctrl Pts',(0.136300969518302,-0.0285369869745706,
-0.2117290813726));
#49188=CARTESIAN_POINT('Ctrl Pts',(0.0977871294194325,0.099146312286434,
-0.203781790064648));
#49189=CARTESIAN_POINT('Ctrl Pts',(-0.0304156058568074,0.135894094238902,
-0.195834498756697));
#49190=CARTESIAN_POINT('Ctrl Pts',(-0.130721601450057,0.0480018417879172,
-0.187887207448745));
#49191=CARTESIAN_POINT('Ctrl Pts',(-0.111131696083687,-0.0839169831016152,
-0.179939916140794));
#49192=CARTESIAN_POINT('Ctrl Pts',(0.0103865420804345,-0.138868404314727,
-0.171992624832842));
#49193=CARTESIAN_POINT('Ctrl Pts',(0.12237839822605,-0.0664517977974861,
-0.164045333524891));
#49194=CARTESIAN_POINT('Ctrl Pts',(0.122126615970329,0.0669134043386132,
-0.156098042216939));
#49195=CARTESIAN_POINT('Ctrl Pts',(0.00986212241425144,0.138906633291134,
-0.148150750908988));
#49196=CARTESIAN_POINT('Ctrl Pts',(-0.111447757822021,0.0834967678264184,
-0.140203459601036));
#49197=CARTESIAN_POINT('Ctrl Pts',(-0.130539427544584,-0.0484950783731256,
-0.132256168293084));
#49198=CARTESIAN_POINT('Ctrl Pts',(-0.0299022661697765,-0.136007978091718,
-0.124308876985132));
#49199=CARTESIAN_POINT('Ctrl Pts',(0.0981607747731693,-0.0987763617687909,
-0.116361585677181));
#49200=CARTESIAN_POINT('Ctrl Pts',(0.136192280372371,0.0290514034709051,
-0.108414294369229));
#49201=CARTESIAN_POINT('Ctrl Pts',(0.0493101426383743,0.130233760247366,
-0.100467003061278));
#49202=CARTESIAN_POINT('Ctrl Pts',(-0.0827982993479119,0.111967457127882,
-0.0925197117533262));
#49203=CARTESIAN_POINT('Ctrl Pts',(-0.138965799441858,-0.00899334747060546,
-0.0845724204453746));
#49204=CARTESIAN_POINT('Ctrl Pts',(-0.0676751419254551,-0.12170630648443,
-0.0766251291374228));
#49205=CARTESIAN_POINT('Ctrl Pts',(0.0656846246959371,-0.122790694602604,
-0.0686778378294716));
#49206=CARTESIAN_POINT('Ctrl Pts',(0.138802320628112,-0.0112558793500066,
-0.0607305465215197));
#49207=CARTESIAN_POINT('Ctrl Pts',(0.0846071216902694,0.110607573555673,
-0.0527832552135683));
#49208=CARTESIAN_POINT('Ctrl Pts',(-0.0471780665789619,0.131014085359439,
-0.0448359639056163));
#49209=CARTESIAN_POINT('Ctrl Pts',(-0.135711977929724,0.0312741384470892,
-0.036888672597665));
#49210=CARTESIAN_POINT('Ctrl Pts',(-0.0997354011396044,-0.097183606994095,
-0.028941381289713));
#49211=CARTESIAN_POINT('Ctrl Pts',(0.027645696947688,-0.136441996699627,
-0.0209940899817616));
#49212=CARTESIAN_POINT('Ctrl Pts',(0.129807118062467,-0.0506808063214575,
-0.0130467986738099));
#49213=CARTESIAN_POINT('Ctrl Pts',(0.112641984414841,0.0818100865641861,
-0.00509950736585856));
#49214=CARTESIAN_POINT('Ctrl Pts',(0.0327209678848226,0.11973912564481,
0.000198686839442543));
#49215=CARTESIAN_POINT('Ctrl Pts',(-0.00642735618902915,0.117599488593358,
0.00284778394209306));
#49216=CARTESIAN_POINT('Ctrl Pts',(-0.00798678478681931,0.146131905375825,
-0.0136500000000002));
#49217=CARTESIAN_POINT('Ctrl Pts',(0.0406598484393165,0.148790668971504,
-0.0162990971026507));
#49218=CARTESIAN_POINT('Ctrl Pts',(0.0903157209469338,0.125224908540822,
-0.0189481942053012));
#49219=CARTESIAN_POINT('Ctrl Pts',(0.118698624029206,0.0860026422449412,
-0.0215972913079517));
#49220=CARTESIAN_POINT('Ctrl Pts',(0.147081527111478,0.0467803759490603,
-0.0242463884106022));
#49221=CARTESIAN_POINT('Ctrl Pts',(0.154191460768405,-0.00809839621201944,
-0.0268954855132527));
#49222=CARTESIAN_POINT('Ctrl Pts',(0.136588394652489,-0.0532992628159412,
-0.0295445826159032));
#49223=CARTESIAN_POINT('Ctrl Pts',(0.118985328536573,-0.0985001294198629,
-0.0321936797185537));
#49224=CARTESIAN_POINT('Ctrl Pts',(0.0766692626478151,-0.134023090466627,
-0.0348427768212043));
#49225=CARTESIAN_POINT('Ctrl Pts',(0.0291301022640015,-0.143654003759554,
-0.0374918739238548));
#49226=CARTESIAN_POINT('Ctrl Pts',(-0.0184090581198122,-0.153284917052481,
-0.0401409710265053));
#49227=CARTESIAN_POINT('Ctrl Pts',(-0.071171312998681,-0.137023782591571,
-0.0427900681291558));
#49228=CARTESIAN_POINT('Ctrl Pts',(-0.105003331279745,-0.102289110011485,
-0.0454391652318063));
#49229=CARTESIAN_POINT('Ctrl Pts',(-0.13116431054537,-0.075430143407223,
-0.0474876086264428));
#49230=CARTESIAN_POINT('Ctrl Pts',(-0.146006285598076,-0.0375252474656216,
-0.0495360520210795));
#49231=CARTESIAN_POINT('Ctrl Pts',(-0.146359156828661,0.000134286233873571,
-0.051584495415716));
#49232=CARTESIAN_POINT('Origin',(0.277715786349443,-0.0489687861020744,
0.04));
#49233=CARTESIAN_POINT('',(0.271097754137541,-0.0461628389679574,0.04));
#49234=CARTESIAN_POINT('',(0.27053717987482,-0.0493420135926708,0.04));
#49235=CARTESIAN_POINT('Origin',(0.,0.,0.04));
#49236=CARTESIAN_POINT('',(0.264913285560284,-0.0467113597924043,0.04));
#49237=CARTESIAN_POINT('',(0.29173382438227,-0.044332558140659,0.04));
#49238=CARTESIAN_POINT('',(0.264913285560284,-0.0467113597924043,0.04));
#49239=CARTESIAN_POINT('Origin',(0.264913285560284,-0.0467113597924043,
0.04));
#49240=CARTESIAN_POINT('',(0.27053717987482,-0.0493420135926708,0.285));
#49241=CARTESIAN_POINT('',(0.27053717987482,-0.0493420135926708,0.1425));
#49242=CARTESIAN_POINT('',(0.264913285560284,-0.0467113597924043,0.291));
#49243=CARTESIAN_POINT('',(0.264913285560284,-0.0467113597924043,0.04));
#49244=CARTESIAN_POINT('Ctrl Pts',(0.27053717987482,-0.0493420135926707,
0.285));
#49245=CARTESIAN_POINT('Ctrl Pts',(0.267694218594527,-0.048012179410566,
0.288035430631103));
#49246=CARTESIAN_POINT('Ctrl Pts',(0.264913285560284,-0.0467113597924043,
0.291));
#49247=CARTESIAN_POINT('Origin',(0.29173382438227,-0.044332558140659,0.04));
#49248=CARTESIAN_POINT('',(0.271097754137541,-0.0461628389679574,0.285));
#49249=CARTESIAN_POINT('',(0.271097754137541,-0.0461628389679574,0.1425));
#49250=CARTESIAN_POINT('Ctrl Pts',(0.264913285560284,-0.0467113597924043,
0.291));
#49251=CARTESIAN_POINT('Ctrl Pts',(0.267971414323715,-0.0464401243111941,
0.288035430631094));
#49252=CARTESIAN_POINT('Ctrl Pts',(0.271097754137541,-0.0461628389679575,
0.285));
#49253=CARTESIAN_POINT('Origin',(0.264993319061626,-0.0964496804178388,
0.04));
#49254=CARTESIAN_POINT('',(0.25896307723613,-0.0925371526922802,0.04));
#49255=CARTESIAN_POINT('',(0.257858961475997,-0.0955706858117092,0.04));
#49256=CARTESIAN_POINT('Origin',(0.,0.,0.04));
#49257=CARTESIAN_POINT('',(0.252777314991409,-0.0920034185546051,0.04));
#49258=CARTESIAN_POINT('',(0.279603464135123,-0.0943180939355711,0.04));
#49259=CARTESIAN_POINT('',(0.252777314991409,-0.0920034185546051,0.04));
#49260=CARTESIAN_POINT('Origin',(0.252777314991409,-0.0920034185546051,
0.04));
#49261=CARTESIAN_POINT('',(0.257858961475997,-0.0955706858117092,0.285));
#49262=CARTESIAN_POINT('',(0.257858961475997,-0.0955706858117092,0.1425));
#49263=CARTESIAN_POINT('',(0.252777314991409,-0.0920034185546051,0.291));
#49264=CARTESIAN_POINT('',(0.252777314991409,-0.0920034185546051,0.04));
#49265=CARTESIAN_POINT('Ctrl Pts',(0.257858961475997,-0.0955706858117092,
0.285));
#49266=CARTESIAN_POINT('Ctrl Pts',(0.255290114447966,-0.0937673797534469,
0.28803543063111));
#49267=CARTESIAN_POINT('Ctrl Pts',(0.252777314991409,-0.0920034185546051,
0.291));
#49268=CARTESIAN_POINT('Origin',(0.279603464135123,-0.0943180939355711,
0.04));
#49269=CARTESIAN_POINT('',(0.25896307723613,-0.0925371526922802,0.285));
#49270=CARTESIAN_POINT('',(0.25896307723613,-0.0925371526922802,0.1425));
#49271=CARTESIAN_POINT('Ctrl Pts',(0.252777314991409,-0.0920034185546051,
0.291));
#49272=CARTESIAN_POINT('Ctrl Pts',(0.255836083454352,-0.0922673422366557,
0.288035430631118));
#49273=CARTESIAN_POINT('Ctrl Pts',(0.25896307723613,-0.0925371526922802,
0.285));
#49274=CARTESIAN_POINT('Origin',(0.244219163867212,-0.141,0.04));
#49275=CARTESIAN_POINT('',(0.238959938274539,-0.136099771858106,0.04));
#49276=CARTESIAN_POINT('',(0.237345829015656,-0.138895491103459,0.04));
#49277=CARTESIAN_POINT('Origin',(0.,0.,0.04));
#49278=CARTESIAN_POINT('',(0.232960833618014,-0.1345,0.04));
#49279=CARTESIAN_POINT('',(0.258977494116409,-0.141437822173509,0.04));
#49280=CARTESIAN_POINT('',(0.232960833618014,-0.1345,0.04));
#49281=CARTESIAN_POINT('Origin',(0.232960833618014,-0.1345,0.04));
#49282=CARTESIAN_POINT('',(0.237345829015656,-0.138895491103459,0.285));
#49283=CARTESIAN_POINT('',(0.237345829015656,-0.138895491103459,0.1425));
#49284=CARTESIAN_POINT('',(0.232960833618014,-0.1345,0.291));
#49285=CARTESIAN_POINT('',(0.232960833618014,-0.1345,0.04));
#49286=CARTESIAN_POINT('Ctrl Pts',(0.237345829015656,-0.138895491103459,
0.285));
#49287=CARTESIAN_POINT('Ctrl Pts',(0.235129149356958,-0.136673505711122,
0.288035430631088));
#49288=CARTESIAN_POINT('Ctrl Pts',(0.232960833618014,-0.1345,0.291));
#49289=CARTESIAN_POINT('Origin',(0.258977494116409,-0.141437822173509,0.04));
#49290=CARTESIAN_POINT('',(0.238959938274539,-0.136099771858106,0.285));
#49291=CARTESIAN_POINT('',(0.238959938274539,-0.136099771858106,0.1425));
#49292=CARTESIAN_POINT('Ctrl Pts',(0.232960833618014,-0.1345,0.291));
#49293=CARTESIAN_POINT('Ctrl Pts',(0.235927302648582,-0.135291063657789,
0.288035430631094));
#49294=CARTESIAN_POINT('Ctrl Pts',(0.238959938274539,-0.136099771858106,
0.285));
#49295=CARTESIAN_POINT('Origin',(0.216024532959552,-0.181266105931604,0.04));
#49296=CARTESIAN_POINT('',(0.211696122508039,-0.175527068325832,0.04));
#49297=CARTESIAN_POINT('',(0.209621063643459,-0.17800002718254,0.04));
#49298=CARTESIAN_POINT('Origin',(0.,0.,0.04));
#49299=CARTESIAN_POINT('',(0.206065955199005,-0.172909867005679,0.04));
#49300=CARTESIAN_POINT('',(0.230482623987904,-0.184260033755696,0.04));
#49301=CARTESIAN_POINT('',(0.206065955199005,-0.172909867005679,0.04));
#49302=CARTESIAN_POINT('Origin',(0.206065955199005,-0.172909867005679,0.04));
#49303=CARTESIAN_POINT('',(0.209621063643459,-0.17800002718254,0.285));
#49304=CARTESIAN_POINT('',(0.209621063643459,-0.17800002718254,0.1425));
#49305=CARTESIAN_POINT('',(0.206065955199005,-0.172909867005679,0.291));
#49306=CARTESIAN_POINT('',(0.206065955199005,-0.172909867005679,0.04));
#49307=CARTESIAN_POINT('Ctrl Pts',(0.209621063643459,-0.17800002718254,
0.285));
#49308=CARTESIAN_POINT('Ctrl Pts',(0.207823904043776,-0.175426876357833,
0.288035430631146));
#49309=CARTESIAN_POINT('Ctrl Pts',(0.206065955199005,-0.172909867005679,
0.291));
#49310=CARTESIAN_POINT('Origin',(0.230482623987904,-0.184260033755696,0.04));
#49311=CARTESIAN_POINT('',(0.211696122508039,-0.175527068325832,0.285));
#49312=CARTESIAN_POINT('',(0.211696122508039,-0.175527068325832,0.1425));
#49313=CARTESIAN_POINT('Ctrl Pts',(0.206065955199005,-0.172909867005679,
0.291));
#49314=CARTESIAN_POINT('Ctrl Pts',(0.208849990136834,-0.174204034570282,
0.288035430631042));
#49315=CARTESIAN_POINT('Ctrl Pts',(0.211696122508039,-0.175527068325832,
0.285));
#49316=CARTESIAN_POINT('Origin',(0.181266105931604,-0.216024532959552,0.04));
#49317=CARTESIAN_POINT('',(0.17800002718254,-0.209621063643459,0.04));
#49318=CARTESIAN_POINT('',(0.175527068325832,-0.211696122508039,0.04));
#49319=CARTESIAN_POINT('Origin',(0.,0.,0.04));
#49320=CARTESIAN_POINT('',(0.172909867005679,-0.206065955199005,0.04));
#49321=CARTESIAN_POINT('',(0.194984655959362,-0.221483597452293,0.04));
#49322=CARTESIAN_POINT('',(0.172909867005679,-0.206065955199005,0.04));
#49323=CARTESIAN_POINT('Origin',(0.172909867005679,-0.206065955199005,0.04));
#49324=CARTESIAN_POINT('',(0.175527068325832,-0.211696122508039,0.285));
#49325=CARTESIAN_POINT('',(0.175527068325832,-0.211696122508039,0.1425));
#49326=CARTESIAN_POINT('',(0.172909867005679,-0.206065955199005,0.291));
#49327=CARTESIAN_POINT('',(0.172909867005679,-0.206065955199005,0.04));
#49328=CARTESIAN_POINT('Ctrl Pts',(0.175527068325832,-0.211696122508039,
0.285));
#49329=CARTESIAN_POINT('Ctrl Pts',(0.174204034570244,-0.208849990136752,
0.288035430631129));
#49330=CARTESIAN_POINT('Ctrl Pts',(0.172909867005679,-0.206065955199005,
0.291));
#49331=CARTESIAN_POINT('Origin',(0.194984655959362,-0.221483597452293,0.04));
#49332=CARTESIAN_POINT('',(0.17800002718254,-0.209621063643459,0.285));
#49333=CARTESIAN_POINT('',(0.17800002718254,-0.209621063643459,0.1425));
#49334=CARTESIAN_POINT('Ctrl Pts',(0.172909867005679,-0.206065955199005,
0.291));
#49335=CARTESIAN_POINT('Ctrl Pts',(0.175426876357872,-0.207823904043804,
0.2880354306311));
#49336=CARTESIAN_POINT('Ctrl Pts',(0.17800002718254,-0.209621063643459,
0.285));
#49337=CARTESIAN_POINT('Origin',(0.141,-0.244219163867212,0.04));
#49338=CARTESIAN_POINT('',(0.138895491103459,-0.237345829015656,0.04));
#49339=CARTESIAN_POINT('',(0.136099771858106,-0.238959938274539,0.04));
#49340=CARTESIAN_POINT('Origin',(0.,0.,0.04));
#49341=CARTESIAN_POINT('',(0.1345,-0.232960833618014,0.04));
#49342=CARTESIAN_POINT('',(0.153562177826491,-0.251977494116409,0.04));
#49343=CARTESIAN_POINT('',(0.1345,-0.232960833618014,0.04));
#49344=CARTESIAN_POINT('Origin',(0.1345,-0.232960833618014,0.04));
#49345=CARTESIAN_POINT('',(0.136099771858106,-0.238959938274539,0.285));
#49346=CARTESIAN_POINT('',(0.136099771858106,-0.238959938274539,0.1425));
#49347=CARTESIAN_POINT('',(0.1345,-0.232960833618014,0.291));
#49348=CARTESIAN_POINT('',(0.1345,-0.232960833618014,0.04));
#49349=CARTESIAN_POINT('Ctrl Pts',(0.136099771858106,-0.238959938274539,
0.285));
#49350=CARTESIAN_POINT('Ctrl Pts',(0.135291063657772,-0.23592730264852,
0.288035430631155));
#49351=CARTESIAN_POINT('Ctrl Pts',(0.1345,-0.232960833618014,0.291));
#49352=CARTESIAN_POINT('Origin',(0.153562177826491,-0.251977494116409,0.04));
#49353=CARTESIAN_POINT('',(0.138895491103459,-0.237345829015656,0.285));
#49354=CARTESIAN_POINT('',(0.138895491103459,-0.237345829015656,0.1425));
#49355=CARTESIAN_POINT('Ctrl Pts',(0.1345,-0.232960833618014,0.291));
#49356=CARTESIAN_POINT('Ctrl Pts',(0.136673505711114,-0.23512914935695,
0.288035430631099));
#49357=CARTESIAN_POINT('Ctrl Pts',(0.138895491103459,-0.237345829015656,
0.285));
#49358=CARTESIAN_POINT('Origin',(0.0964496804178385,-0.264993319061626,
0.04));
#49359=CARTESIAN_POINT('',(0.0955706858117088,-0.257858961475997,0.04));
#49360=CARTESIAN_POINT('',(0.0925371526922799,-0.25896307723613,0.04));
#49361=CARTESIAN_POINT('Origin',(0.,0.,0.04));
#49362=CARTESIAN_POINT('',(0.0920034185546048,-0.252777314991409,0.04));
#49363=CARTESIAN_POINT('',(0.107473790626574,-0.274815182128563,0.04));
#49364=CARTESIAN_POINT('',(0.0920034185546048,-0.252777314991409,0.04));
#49365=CARTESIAN_POINT('Origin',(0.0920034185546048,-0.252777314991409,
0.04));
#49366=CARTESIAN_POINT('',(0.0925371526922799,-0.25896307723613,0.285));
#49367=CARTESIAN_POINT('',(0.0925371526922799,-0.25896307723613,0.1425));
#49368=CARTESIAN_POINT('',(0.0920034185546048,-0.252777314991409,0.291));
#49369=CARTESIAN_POINT('',(0.0920034185546048,-0.252777314991409,0.04));
#49370=CARTESIAN_POINT('Ctrl Pts',(0.0925371526922799,-0.25896307723613,
0.285));
#49371=CARTESIAN_POINT('Ctrl Pts',(0.0922673422366487,-0.255836083454274,
0.288035430631194));
#49372=CARTESIAN_POINT('Ctrl Pts',(0.0920034185546048,-0.252777314991409,
0.291));
#49373=CARTESIAN_POINT('Origin',(0.107473790626574,-0.274815182128563,0.04));
#49374=CARTESIAN_POINT('',(0.0955706858117089,-0.257858961475997,0.285));
#49375=CARTESIAN_POINT('',(0.0955706858117089,-0.257858961475997,0.1425));
#49376=CARTESIAN_POINT('Ctrl Pts',(0.0920034185546048,-0.252777314991409,
0.291));
#49377=CARTESIAN_POINT('Ctrl Pts',(0.0937673797534969,-0.255290114448038,
0.288035430631026));
#49378=CARTESIAN_POINT('Ctrl Pts',(0.0955706858117088,-0.257858961475997,
0.285));
#49379=CARTESIAN_POINT('Origin',(0.0489687861020743,-0.277715786349443,
0.04));
#49380=CARTESIAN_POINT('',(0.0493420135926707,-0.27053717987482,0.04));
#49381=CARTESIAN_POINT('',(0.0461628389679573,-0.271097754137541,0.04));
#49382=CARTESIAN_POINT('Origin',(0.,0.,0.04));
#49383=CARTESIAN_POINT('',(0.0467113597924042,-0.264913285560284,0.04));
#49384=CARTESIAN_POINT('',(0.0581198666828298,-0.289302749894933,0.04));
#49385=CARTESIAN_POINT('',(0.0467113597924042,-0.264913285560284,0.04));
#49386=CARTESIAN_POINT('Origin',(0.0467113597924042,-0.264913285560284,
0.04));
#49387=CARTESIAN_POINT('',(0.0461628389679573,-0.271097754137541,0.285));
#49388=CARTESIAN_POINT('',(0.0461628389679573,-0.271097754137541,0.1425));
#49389=CARTESIAN_POINT('',(0.0467113597924042,-0.264913285560284,0.291));
#49390=CARTESIAN_POINT('',(0.0467113597924042,-0.264913285560284,0.04));
#49391=CARTESIAN_POINT('Ctrl Pts',(0.0461628389679573,-0.271097754137541,
0.285));
#49392=CARTESIAN_POINT('Ctrl Pts',(0.0464401243112015,-0.26797141432363,
0.288035430631177));
#49393=CARTESIAN_POINT('Ctrl Pts',(0.0467113597924042,-0.264913285560284,
0.291));
#49394=CARTESIAN_POINT('Origin',(0.0581198666828298,-0.289302749894933,
0.04));
#49395=CARTESIAN_POINT('',(0.0493420135926707,-0.27053717987482,0.285));
#49396=CARTESIAN_POINT('',(0.0493420135926707,-0.27053717987482,0.1425));
#49397=CARTESIAN_POINT('Ctrl Pts',(0.0467113597924042,-0.264913285560284,
0.291));
#49398=CARTESIAN_POINT('Ctrl Pts',(0.0480121794105309,-0.267694218594452,
0.288035430631183));
#49399=CARTESIAN_POINT('Ctrl Pts',(0.0493420135926707,-0.27053717987482,
0.285));
#49400=CARTESIAN_POINT('Origin',(-4.85722573273506E-17,-0.282,0.04));
#49401=CARTESIAN_POINT('',(0.00161410925888288,-0.274995262961565,0.04));
#49402=CARTESIAN_POINT('',(-0.00161410925888299,-0.274995262961565,0.04));
#49403=CARTESIAN_POINT('Origin',(0.,0.,0.04));
#49404=CARTESIAN_POINT('',(-6.24500451351651E-17,-0.269,0.04));
#49405=CARTESIAN_POINT('',(0.00699999999999995,-0.295,0.04));
#49406=CARTESIAN_POINT('',(-6.24500451351651E-17,-0.269,0.04));
#49407=CARTESIAN_POINT('Origin',(-6.24500451351651E-17,-0.269,0.04));
#49408=CARTESIAN_POINT('',(-0.00161410925888297,-0.274995262961565,0.285));
#49409=CARTESIAN_POINT('',(-0.00161410925888297,-0.274995262961565,0.1425));
#49410=CARTESIAN_POINT('',(-6.2450045135165E-17,-0.269,0.291));
#49411=CARTESIAN_POINT('',(-6.24500451351651E-17,-0.269,0.04));
#49412=CARTESIAN_POINT('Ctrl Pts',(-0.00161410925888296,-0.274995262961565,
0.285));
#49413=CARTESIAN_POINT('Ctrl Pts',(-0.000798153291622722,-0.271964569368884,
0.288035430631116));
#49414=CARTESIAN_POINT('Ctrl Pts',(-6.24500451351651E-17,-0.269,0.291));
#49415=CARTESIAN_POINT('Origin',(0.00699999999999995,-0.295,0.04));
#49416=CARTESIAN_POINT('',(0.00161410925888286,-0.274995262961565,0.285));
#49417=CARTESIAN_POINT('',(0.00161410925888286,-0.274995262961565,0.1425));
#49418=CARTESIAN_POINT('Ctrl Pts',(-6.2450045135165E-17,-0.269,0.291));
#49419=CARTESIAN_POINT('Ctrl Pts',(0.000798153291617013,-0.271964569368863,
0.288035430631137));
#49420=CARTESIAN_POINT('Ctrl Pts',(0.00161410925888284,-0.274995262961565,
0.285));
#49421=CARTESIAN_POINT('Origin',(-0.0489687861020744,-0.277715786349443,
0.04));
#49422=CARTESIAN_POINT('',(-0.0461628389679574,-0.271097754137541,0.04));
#49423=CARTESIAN_POINT('',(-0.0493420135926708,-0.27053717987482,0.04));
#49424=CARTESIAN_POINT('Origin',(0.,0.,0.04));
#49425=CARTESIAN_POINT('',(-0.0467113597924043,-0.264913285560284,0.04));
#49426=CARTESIAN_POINT('',(-0.044332558140659,-0.29173382438227,0.04));
#49427=CARTESIAN_POINT('',(-0.0467113597924043,-0.264913285560284,0.04));
#49428=CARTESIAN_POINT('Origin',(-0.0467113597924043,-0.264913285560284,
0.04));
#49429=CARTESIAN_POINT('',(-0.0493420135926708,-0.27053717987482,0.285));
#49430=CARTESIAN_POINT('',(-0.0493420135926708,-0.27053717987482,0.1425));
#49431=CARTESIAN_POINT('',(-0.0467113597924043,-0.264913285560284,0.291));
#49432=CARTESIAN_POINT('',(-0.0467113597924043,-0.264913285560284,0.04));
#49433=CARTESIAN_POINT('Ctrl Pts',(-0.0493420135926708,-0.27053717987482,
0.285));
#49434=CARTESIAN_POINT('Ctrl Pts',(-0.0480121794105265,-0.267694218594442,
0.288035430631193));
#49435=CARTESIAN_POINT('Ctrl Pts',(-0.0467113597924043,-0.264913285560284,
0.291));
#49436=CARTESIAN_POINT('Origin',(-0.044332558140659,-0.29173382438227,0.04));
#49437=CARTESIAN_POINT('',(-0.0461628389679574,-0.271097754137541,0.285));
#49438=CARTESIAN_POINT('',(-0.0461628389679574,-0.271097754137541,0.1425));
#49439=CARTESIAN_POINT('Ctrl Pts',(-0.0467113597924043,-0.264913285560284,
0.291));
#49440=CARTESIAN_POINT('Ctrl Pts',(-0.046440124311189,-0.267971414323772,
0.288035430631039));
#49441=CARTESIAN_POINT('Ctrl Pts',(-0.0461628389679575,-0.271097754137541,
0.285));
#49442=CARTESIAN_POINT('Origin',(-0.0964496804178388,-0.264993319061626,
0.04));
#49443=CARTESIAN_POINT('',(-0.0925371526922802,-0.25896307723613,0.04));
#49444=CARTESIAN_POINT('',(-0.0955706858117092,-0.257858961475997,0.04));
#49445=CARTESIAN_POINT('Origin',(0.,0.,0.04));
#49446=CARTESIAN_POINT('',(-0.0920034185546051,-0.252777314991409,0.04));
#49447=CARTESIAN_POINT('',(-0.0943180939355711,-0.279603464135123,0.04));
#49448=CARTESIAN_POINT('',(-0.0920034185546051,-0.252777314991409,0.04));
#49449=CARTESIAN_POINT('Origin',(-0.0920034185546051,-0.252777314991409,
0.04));
#49450=CARTESIAN_POINT('',(-0.0955706858117092,-0.257858961475997,0.285));
#49451=CARTESIAN_POINT('',(-0.0955706858117092,-0.257858961475997,0.1425));
#49452=CARTESIAN_POINT('',(-0.0920034185546051,-0.252777314991409,0.291));
#49453=CARTESIAN_POINT('',(-0.0920034185546051,-0.252777314991409,0.04));
#49454=CARTESIAN_POINT('Ctrl Pts',(-0.0955706858117091,-0.257858961475997,
0.285));
#49455=CARTESIAN_POINT('Ctrl Pts',(-0.0937673797534664,-0.255290114447994,
0.288035430631078));
#49456=CARTESIAN_POINT('Ctrl Pts',(-0.0920034185546051,-0.252777314991409,
0.291));
#49457=CARTESIAN_POINT('Origin',(-0.0943180939355711,-0.279603464135123,
0.04));
#49458=CARTESIAN_POINT('',(-0.0925371526922802,-0.25896307723613,0.285));
#49459=CARTESIAN_POINT('',(-0.0925371526922802,-0.25896307723613,0.1425));
#49460=CARTESIAN_POINT('Ctrl Pts',(-0.0920034185546051,-0.252777314991409,
0.291));
#49461=CARTESIAN_POINT('Ctrl Pts',(-0.0922673422366578,-0.255836083454375,
0.288035430631095));
#49462=CARTESIAN_POINT('Ctrl Pts',(-0.0925371526922802,-0.25896307723613,
0.285));
#49463=CARTESIAN_POINT('Origin',(-0.141,-0.244219163867212,0.04));
#49464=CARTESIAN_POINT('',(-0.136099771858106,-0.238959938274539,0.04));
#49465=CARTESIAN_POINT('',(-0.138895491103459,-0.237345829015656,0.04));
#49466=CARTESIAN_POINT('Origin',(0.,0.,0.04));
#49467=CARTESIAN_POINT('',(-0.1345,-0.232960833618014,0.04));
#49468=CARTESIAN_POINT('',(-0.141437822173509,-0.258977494116409,0.04));
#49469=CARTESIAN_POINT('',(-0.1345,-0.232960833618014,0.04));
#49470=CARTESIAN_POINT('Origin',(-0.1345,-0.232960833618014,0.04));
#49471=CARTESIAN_POINT('',(-0.138895491103459,-0.237345829015656,0.285));
#49472=CARTESIAN_POINT('',(-0.138895491103459,-0.237345829015656,0.1425));
#49473=CARTESIAN_POINT('',(-0.1345,-0.232960833618014,0.291));
#49474=CARTESIAN_POINT('',(-0.1345,-0.232960833618014,0.04));
#49475=CARTESIAN_POINT('Ctrl Pts',(-0.138895491103459,-0.237345829015656,
0.285));
#49476=CARTESIAN_POINT('Ctrl Pts',(-0.136673505711122,-0.235129149356958,
0.288035430631088));
#49477=CARTESIAN_POINT('Ctrl Pts',(-0.1345,-0.232960833618014,0.291));
#49478=CARTESIAN_POINT('Origin',(-0.141437822173509,-0.258977494116409,
0.04));
#49479=CARTESIAN_POINT('',(-0.136099771858106,-0.238959938274539,0.285));
#49480=CARTESIAN_POINT('',(-0.136099771858106,-0.238959938274539,0.1425));
#49481=CARTESIAN_POINT('Ctrl Pts',(-0.1345,-0.232960833618014,0.291));
#49482=CARTESIAN_POINT('Ctrl Pts',(-0.135291063657789,-0.235927302648582,
0.288035430631094));
#49483=CARTESIAN_POINT('Ctrl Pts',(-0.136099771858106,-0.238959938274539,
0.285));
#49484=CARTESIAN_POINT('Origin',(-0.181266105931604,-0.216024532959552,
0.04));
#49485=CARTESIAN_POINT('',(-0.175527068325832,-0.211696122508039,0.04));
#49486=CARTESIAN_POINT('',(-0.17800002718254,-0.209621063643459,0.04));
#49487=CARTESIAN_POINT('Origin',(0.,0.,0.04));
#49488=CARTESIAN_POINT('',(-0.172909867005679,-0.206065955199005,0.04));
#49489=CARTESIAN_POINT('',(-0.184260033755696,-0.230482623987904,0.04));
#49490=CARTESIAN_POINT('',(-0.172909867005679,-0.206065955199005,0.04));
#49491=CARTESIAN_POINT('Origin',(-0.172909867005679,-0.206065955199005,
0.04));
#49492=CARTESIAN_POINT('',(-0.17800002718254,-0.209621063643459,0.285));
#49493=CARTESIAN_POINT('',(-0.17800002718254,-0.209621063643459,0.1425));
#49494=CARTESIAN_POINT('',(-0.172909867005679,-0.206065955199005,0.291));
#49495=CARTESIAN_POINT('',(-0.172909867005679,-0.206065955199005,0.04));
#49496=CARTESIAN_POINT('Ctrl Pts',(-0.17800002718254,-0.209621063643459,
0.285));
#49497=CARTESIAN_POINT('Ctrl Pts',(-0.175426876357765,-0.207823904043728,
0.288035430631226));
#49498=CARTESIAN_POINT('Ctrl Pts',(-0.172909867005679,-0.206065955199005,
0.291));
#49499=CARTESIAN_POINT('Origin',(-0.184260033755696,-0.230482623987904,
0.04));
#49500=CARTESIAN_POINT('',(-0.175527068325832,-0.211696122508039,0.285));
#49501=CARTESIAN_POINT('',(-0.175527068325832,-0.211696122508039,0.1425));
#49502=CARTESIAN_POINT('Ctrl Pts',(-0.172909867005679,-0.206065955199005,
0.291));
#49503=CARTESIAN_POINT('Ctrl Pts',(-0.174204034570293,-0.208849990136858,
0.288035430631017));
#49504=CARTESIAN_POINT('Ctrl Pts',(-0.175527068325832,-0.211696122508039,
0.285));
#49505=CARTESIAN_POINT('Origin',(-0.216024532959552,-0.181266105931604,
0.04));
#49506=CARTESIAN_POINT('',(-0.209621063643459,-0.17800002718254,0.04));
#49507=CARTESIAN_POINT('',(-0.211696122508039,-0.175527068325832,0.04));
#49508=CARTESIAN_POINT('Origin',(0.,0.,0.04));
#49509=CARTESIAN_POINT('',(-0.206065955199005,-0.172909867005679,0.04));
#49510=CARTESIAN_POINT('',(-0.221483597452293,-0.194984655959362,0.04));
#49511=CARTESIAN_POINT('',(-0.206065955199005,-0.172909867005679,0.04));
#49512=CARTESIAN_POINT('Origin',(-0.206065955199005,-0.172909867005679,
0.04));
#49513=CARTESIAN_POINT('',(-0.211696122508039,-0.175527068325832,0.285));
#49514=CARTESIAN_POINT('',(-0.211696122508039,-0.175527068325832,0.1425));
#49515=CARTESIAN_POINT('',(-0.206065955199005,-0.172909867005679,0.291));
#49516=CARTESIAN_POINT('',(-0.206065955199005,-0.172909867005679,0.04));
#49517=CARTESIAN_POINT('Ctrl Pts',(-0.211696122508039,-0.175527068325832,
0.285));
#49518=CARTESIAN_POINT('Ctrl Pts',(-0.208849990136656,-0.174204034570199,
0.288035430631232));
#49519=CARTESIAN_POINT('Ctrl Pts',(-0.206065955199005,-0.172909867005679,
0.291));
#49520=CARTESIAN_POINT('Origin',(-0.221483597452293,-0.194984655959362,
0.04));
#49521=CARTESIAN_POINT('',(-0.209621063643459,-0.17800002718254,0.285));
#49522=CARTESIAN_POINT('',(-0.209621063643459,-0.17800002718254,0.1425));
#49523=CARTESIAN_POINT('Ctrl Pts',(-0.206065955199005,-0.172909867005679,
0.291));
#49524=CARTESIAN_POINT('Ctrl Pts',(-0.207823904043843,-0.175426876357928,
0.288035430631034));
#49525=CARTESIAN_POINT('Ctrl Pts',(-0.209621063643459,-0.17800002718254,
0.285));
#49526=CARTESIAN_POINT('Origin',(-0.244219163867212,-0.141,0.04));
#49527=CARTESIAN_POINT('',(-0.237345829015656,-0.138895491103459,0.04));
#49528=CARTESIAN_POINT('',(-0.238959938274539,-0.136099771858106,0.04));
#49529=CARTESIAN_POINT('Origin',(0.,0.,0.04));
#49530=CARTESIAN_POINT('',(-0.232960833618014,-0.1345,0.04));
#49531=CARTESIAN_POINT('',(-0.25197749411641,-0.153562177826491,0.04));
#49532=CARTESIAN_POINT('',(-0.232960833618014,-0.1345,0.04));
#49533=CARTESIAN_POINT('Origin',(-0.232960833618014,-0.1345,0.04));
#49534=CARTESIAN_POINT('',(-0.238959938274539,-0.136099771858106,0.285));
#49535=CARTESIAN_POINT('',(-0.238959938274539,-0.136099771858106,0.1425));
#49536=CARTESIAN_POINT('',(-0.232960833618014,-0.1345,0.291));
#49537=CARTESIAN_POINT('',(-0.232960833618014,-0.1345,0.04));
#49538=CARTESIAN_POINT('Ctrl Pts',(-0.238959938274539,-0.136099771858106,
0.285));
#49539=CARTESIAN_POINT('Ctrl Pts',(-0.23592730264851,-0.135291063657769,
0.288035430631166));
#49540=CARTESIAN_POINT('Ctrl Pts',(-0.232960833618014,-0.1345,0.291));
#49541=CARTESIAN_POINT('Origin',(-0.25197749411641,-0.153562177826491,0.04));
#49542=CARTESIAN_POINT('',(-0.237345829015656,-0.138895491103459,0.285));
#49543=CARTESIAN_POINT('',(-0.237345829015656,-0.138895491103459,0.1425));
#49544=CARTESIAN_POINT('Ctrl Pts',(-0.232960833618014,-0.1345,0.291));
#49545=CARTESIAN_POINT('Ctrl Pts',(-0.235129149356959,-0.136673505711123,
0.288035430631086));
#49546=CARTESIAN_POINT('Ctrl Pts',(-0.237345829015656,-0.138895491103459,
0.285));
#49547=CARTESIAN_POINT('Origin',(-0.264993319061626,-0.0964496804178386,
0.04));
#49548=CARTESIAN_POINT('',(-0.257858961475997,-0.095570685811709,0.04));
#49549=CARTESIAN_POINT('',(-0.25896307723613,-0.09253715269228,0.04));
#49550=CARTESIAN_POINT('Origin',(0.,0.,0.04));
#49551=CARTESIAN_POINT('',(-0.252777314991409,-0.0920034185546049,0.04));
#49552=CARTESIAN_POINT('',(-0.274815182128563,-0.107473790626574,0.04));
#49553=CARTESIAN_POINT('',(-0.252777314991409,-0.0920034185546049,0.04));
#49554=CARTESIAN_POINT('Origin',(-0.252777314991409,-0.0920034185546049,
0.04));
#49555=CARTESIAN_POINT('',(-0.25896307723613,-0.09253715269228,0.285));
#49556=CARTESIAN_POINT('',(-0.25896307723613,-0.09253715269228,0.1425));
#49557=CARTESIAN_POINT('',(-0.252777314991409,-0.0920034185546049,0.291));
#49558=CARTESIAN_POINT('',(-0.252777314991409,-0.0920034185546049,0.04));
#49559=CARTESIAN_POINT('Ctrl Pts',(-0.25896307723613,-0.09253715269228,
0.285));
#49560=CARTESIAN_POINT('Ctrl Pts',(-0.255836083454338,-0.0922673422366543,
0.288035430631132));
#49561=CARTESIAN_POINT('Ctrl Pts',(-0.252777314991409,-0.0920034185546049,
0.291));
#49562=CARTESIAN_POINT('Origin',(-0.274815182128563,-0.107473790626574,
0.04));
#49563=CARTESIAN_POINT('',(-0.257858961475997,-0.095570685811709,0.285));
#49564=CARTESIAN_POINT('',(-0.257858961475997,-0.095570685811709,0.1425));
#49565=CARTESIAN_POINT('Ctrl Pts',(-0.252777314991409,-0.0920034185546049,
0.291));
#49566=CARTESIAN_POINT('Ctrl Pts',(-0.255290114448016,-0.0937673797534821,
0.288035430631051));
#49567=CARTESIAN_POINT('Ctrl Pts',(-0.257858961475997,-0.0955706858117089,
0.285));
#49568=CARTESIAN_POINT('Origin',(-0.277715786349443,-0.0489687861020743,
0.04));
#49569=CARTESIAN_POINT('',(-0.27053717987482,-0.0493420135926707,0.04));
#49570=CARTESIAN_POINT('',(-0.271097754137541,-0.0461628389679573,0.04));
#49571=CARTESIAN_POINT('Origin',(0.,0.,0.04));
#49572=CARTESIAN_POINT('',(-0.264913285560284,-0.0467113597924042,0.04));
#49573=CARTESIAN_POINT('',(-0.289302749894933,-0.0581198666828298,0.04));
#49574=CARTESIAN_POINT('',(-0.264913285560284,-0.0467113597924042,0.04));
#49575=CARTESIAN_POINT('Origin',(-0.264913285560284,-0.0467113597924042,
0.04));
#49576=CARTESIAN_POINT('',(-0.271097754137541,-0.0461628389679573,0.285));
#49577=CARTESIAN_POINT('',(-0.271097754137541,-0.0461628389679573,0.1425));
#49578=CARTESIAN_POINT('',(-0.264913285560284,-0.0467113597924042,0.291));
#49579=CARTESIAN_POINT('',(-0.264913285560284,-0.0467113597924042,0.04));
#49580=CARTESIAN_POINT('Ctrl Pts',(-0.271097754137541,-0.0461628389679573,
0.285));
#49581=CARTESIAN_POINT('Ctrl Pts',(-0.267971414323669,-0.0464401243111981,
0.288035430631139));
#49582=CARTESIAN_POINT('Ctrl Pts',(-0.264913285560284,-0.0467113597924042,
0.291));
#49583=CARTESIAN_POINT('Origin',(-0.289302749894933,-0.0581198666828298,
0.04));
#49584=CARTESIAN_POINT('',(-0.27053717987482,-0.0493420135926707,0.285));
#49585=CARTESIAN_POINT('',(-0.27053717987482,-0.0493420135926707,0.1425));
#49586=CARTESIAN_POINT('Ctrl Pts',(-0.264913285560284,-0.0467113597924042,
0.291));
#49587=CARTESIAN_POINT('Ctrl Pts',(-0.2676942185945,-0.0480121794105537,
0.288035430631131));
#49588=CARTESIAN_POINT('Ctrl Pts',(-0.27053717987482,-0.0493420135926707,
0.285));
#49589=CARTESIAN_POINT('Origin',(-0.282,2.77555756156289E-17,0.04));
#49590=CARTESIAN_POINT('',(-0.274995262961565,-0.0016141092588829,0.04));
#49591=CARTESIAN_POINT('',(-0.275,-3.36777869765522E-17,0.04));
#49592=CARTESIAN_POINT('Origin',(0.,0.,0.04));
#49593=CARTESIAN_POINT('',(-0.269,4.16333634234434E-17,0.04));
#49594=CARTESIAN_POINT('',(-0.295,-0.00699999999999998,0.04));
#49595=CARTESIAN_POINT('',(-0.274995262961565,0.00161410925888296,0.04));
#49596=CARTESIAN_POINT('',(-0.269,4.16333634234434E-17,0.04));
#49597=CARTESIAN_POINT('Origin',(0.,0.,0.04));
#49598=CARTESIAN_POINT('Origin',(-0.269,4.16333634234434E-17,0.04));
#49599=CARTESIAN_POINT('',(-0.274995262961565,0.00161410925888297,0.285));
#49600=CARTESIAN_POINT('',(-0.274995262961565,0.00161410925888297,0.1425));
#49601=CARTESIAN_POINT('',(-0.269,4.16333634234434E-17,0.291));
#49602=CARTESIAN_POINT('',(-0.269,4.16333634234434E-17,0.04));
#49603=CARTESIAN_POINT('Ctrl Pts',(-0.274995262961565,0.00161410925888294,
0.285));
#49604=CARTESIAN_POINT('Ctrl Pts',(-0.271964569368884,0.000798153291622702,
0.288035430631116));
#49605=CARTESIAN_POINT('Ctrl Pts',(-0.269,4.16333634234434E-17,0.291));
#49606=CARTESIAN_POINT('Origin',(-0.295,-0.00699999999999998,0.04));
#49607=CARTESIAN_POINT('',(-0.274995262961565,-0.0016141092588829,0.285));
#49608=CARTESIAN_POINT('',(-0.274995262961565,-0.0016141092588829,0.1425));
#49609=CARTESIAN_POINT('Ctrl Pts',(-0.269,4.16333634234434E-17,0.291));
#49610=CARTESIAN_POINT('Ctrl Pts',(-0.271964569368901,-0.000798153291627193,
0.288035430631099));
#49611=CARTESIAN_POINT('Ctrl Pts',(-0.274995262961565,-0.00161410925888289,
0.285));
#49612=CARTESIAN_POINT('Origin',(-0.277715786349443,0.0489687861020745,
0.04));
#49613=CARTESIAN_POINT('',(-0.271097754137541,0.0461628389679575,0.04));
#49614=CARTESIAN_POINT('',(-0.27053717987482,0.0493420135926709,0.04));
#49615=CARTESIAN_POINT('Origin',(0.,0.,0.04));
#49616=CARTESIAN_POINT('',(-0.264913285560284,0.0467113597924044,0.04));
#49617=CARTESIAN_POINT('',(-0.29173382438227,0.0443325581406591,0.04));
#49618=CARTESIAN_POINT('',(-0.264913285560284,0.0467113597924044,0.04));
#49619=CARTESIAN_POINT('Origin',(-0.264913285560284,0.0467113597924044,
0.04));
#49620=CARTESIAN_POINT('',(-0.27053717987482,0.0493420135926709,0.285));
#49621=CARTESIAN_POINT('',(-0.27053717987482,0.0493420135926709,0.1425));
#49622=CARTESIAN_POINT('',(-0.264913285560284,0.0467113597924044,0.291));
#49623=CARTESIAN_POINT('',(-0.264913285560284,0.0467113597924044,0.04));
#49624=CARTESIAN_POINT('Ctrl Pts',(-0.27053717987482,0.0493420135926709,
0.285));
#49625=CARTESIAN_POINT('Ctrl Pts',(-0.267694218594536,0.0480121794105704,
0.288035430631093));
#49626=CARTESIAN_POINT('Ctrl Pts',(-0.264913285560284,0.0467113597924044,
0.291));
#49627=CARTESIAN_POINT('Origin',(-0.29173382438227,0.0443325581406591,0.04));
#49628=CARTESIAN_POINT('',(-0.271097754137541,0.0461628389679575,0.285));
#49629=CARTESIAN_POINT('',(-0.271097754137541,0.0461628389679575,0.1425));
#49630=CARTESIAN_POINT('Ctrl Pts',(-0.264913285560284,0.0467113597924044,
0.291));
#49631=CARTESIAN_POINT('Ctrl Pts',(-0.267971414323744,0.0464401243111915,
0.288035430631066));
#49632=CARTESIAN_POINT('Ctrl Pts',(-0.271097754137541,0.0461628389679575,
0.285));
#49633=CARTESIAN_POINT('Origin',(-0.264993319061626,0.0964496804178386,
0.04));
#49634=CARTESIAN_POINT('',(-0.25896307723613,0.09253715269228,0.04));
#49635=CARTESIAN_POINT('',(-0.257858961475997,0.095570685811709,0.04));
#49636=CARTESIAN_POINT('Origin',(0.,0.,0.04));
#49637=CARTESIAN_POINT('',(-0.252777314991409,0.0920034185546049,0.04));
#49638=CARTESIAN_POINT('',(-0.279603464135123,0.094318093935571,0.04));
#49639=CARTESIAN_POINT('',(-0.252777314991409,0.0920034185546049,0.04));
#49640=CARTESIAN_POINT('Origin',(-0.252777314991409,0.0920034185546049,
0.04));
#49641=CARTESIAN_POINT('',(-0.257858961475997,0.095570685811709,0.285));
#49642=CARTESIAN_POINT('',(-0.257858961475997,0.095570685811709,0.1425));
#49643=CARTESIAN_POINT('',(-0.252777314991409,0.0920034185546049,0.291));
#49644=CARTESIAN_POINT('',(-0.252777314991409,0.0920034185546049,0.04));
#49645=CARTESIAN_POINT('Ctrl Pts',(-0.257858961475997,0.095570685811709,
0.285));
#49646=CARTESIAN_POINT('Ctrl Pts',(-0.255290114447956,0.0937673797534397,
0.288035430631122));
#49647=CARTESIAN_POINT('Ctrl Pts',(-0.252777314991409,0.0920034185546049,
0.291));
#49648=CARTESIAN_POINT('Origin',(-0.279603464135123,0.094318093935571,0.04));
#49649=CARTESIAN_POINT('',(-0.25896307723613,0.09253715269228,0.285));
#49650=CARTESIAN_POINT('',(-0.25896307723613,0.09253715269228,0.1425));
#49651=CARTESIAN_POINT('Ctrl Pts',(-0.252777314991409,0.0920034185546049,
0.291));
#49652=CARTESIAN_POINT('Ctrl Pts',(-0.255836083454369,0.0922673422366571,
0.288035430631101));
#49653=CARTESIAN_POINT('Ctrl Pts',(-0.25896307723613,0.09253715269228,0.285));
#49654=CARTESIAN_POINT('Origin',(-0.244219163867212,0.141,0.04));
#49655=CARTESIAN_POINT('',(-0.238959938274539,0.136099771858106,0.04));
#49656=CARTESIAN_POINT('',(-0.237345829015656,0.138895491103459,0.04));
#49657=CARTESIAN_POINT('Origin',(0.,0.,0.04));
#49658=CARTESIAN_POINT('',(-0.232960833618014,0.1345,0.04));
#49659=CARTESIAN_POINT('',(-0.25897749411641,0.141437822173509,0.04));
#49660=CARTESIAN_POINT('',(-0.232960833618014,0.1345,0.04));
#49661=CARTESIAN_POINT('Origin',(-0.232960833618014,0.1345,0.04));
#49662=CARTESIAN_POINT('',(-0.237345829015656,0.138895491103459,0.285));
#49663=CARTESIAN_POINT('',(-0.237345829015656,0.138895491103459,0.1425));
#49664=CARTESIAN_POINT('',(-0.232960833618014,0.1345,0.291));
#49665=CARTESIAN_POINT('',(-0.232960833618014,0.1345,0.04));
#49666=CARTESIAN_POINT('Ctrl Pts',(-0.237345829015656,0.138895491103459,
0.285));
#49667=CARTESIAN_POINT('Ctrl Pts',(-0.23512914935695,0.136673505711114,
0.288035430631098));
#49668=CARTESIAN_POINT('Ctrl Pts',(-0.232960833618014,0.1345,0.291));
#49669=CARTESIAN_POINT('Origin',(-0.25897749411641,0.141437822173509,0.04));
#49670=CARTESIAN_POINT('',(-0.238959938274539,0.136099771858106,0.285));
#49671=CARTESIAN_POINT('',(-0.238959938274539,0.136099771858106,0.1425));
#49672=CARTESIAN_POINT('Ctrl Pts',(-0.232960833618014,0.1345,0.291));
#49673=CARTESIAN_POINT('Ctrl Pts',(-0.235927302648541,0.135291063657777,
0.288035430631136));
#49674=CARTESIAN_POINT('Ctrl Pts',(-0.238959938274539,0.136099771858106,
0.285));
#49675=CARTESIAN_POINT('Origin',(-0.216024532959552,0.181266105931604,0.04));
#49676=CARTESIAN_POINT('',(-0.211696122508039,0.175527068325832,0.04));
#49677=CARTESIAN_POINT('',(-0.209621063643459,0.17800002718254,0.04));
#49678=CARTESIAN_POINT('Origin',(0.,0.,0.04));
#49679=CARTESIAN_POINT('',(-0.206065955199005,0.172909867005679,0.04));
#49680=CARTESIAN_POINT('',(-0.230482623987904,0.184260033755696,0.04));
#49681=CARTESIAN_POINT('',(-0.206065955199005,0.172909867005679,0.04));
#49682=CARTESIAN_POINT('Origin',(-0.206065955199005,0.172909867005679,0.04));
#49683=CARTESIAN_POINT('',(-0.209621063643459,0.17800002718254,0.285));
#49684=CARTESIAN_POINT('',(-0.209621063643459,0.17800002718254,0.1425));
#49685=CARTESIAN_POINT('',(-0.206065955199005,0.172909867005679,0.291));
#49686=CARTESIAN_POINT('',(-0.206065955199005,0.172909867005679,0.04));
#49687=CARTESIAN_POINT('Ctrl Pts',(-0.209621063643459,0.17800002718254,
0.285));
#49688=CARTESIAN_POINT('Ctrl Pts',(-0.207823904043728,0.175426876357765,
0.288035430631226));
#49689=CARTESIAN_POINT('Ctrl Pts',(-0.206065955199005,0.172909867005679,
0.291));
#49690=CARTESIAN_POINT('Origin',(-0.230482623987904,0.184260033755696,0.04));
#49691=CARTESIAN_POINT('',(-0.211696122508039,0.175527068325832,0.285));
#49692=CARTESIAN_POINT('',(-0.211696122508039,0.175527068325832,0.1425));
#49693=CARTESIAN_POINT('Ctrl Pts',(-0.206065955199005,0.172909867005679,
0.291));
#49694=CARTESIAN_POINT('Ctrl Pts',(-0.208849990136858,0.174204034570293,
0.288035430631017));
#49695=CARTESIAN_POINT('Ctrl Pts',(-0.211696122508039,0.175527068325832,
0.285));
#49696=CARTESIAN_POINT('Origin',(-0.181266105931604,0.216024532959552,0.04));
#49697=CARTESIAN_POINT('',(-0.17800002718254,0.209621063643459,0.04));
#49698=CARTESIAN_POINT('',(-0.175527068325832,0.211696122508039,0.04));
#49699=CARTESIAN_POINT('Origin',(0.,0.,0.04));
#49700=CARTESIAN_POINT('',(-0.172909867005679,0.206065955199005,0.04));
#49701=CARTESIAN_POINT('',(-0.194984655959362,0.221483597452293,0.04));
#49702=CARTESIAN_POINT('',(-0.172909867005679,0.206065955199005,0.04));
#49703=CARTESIAN_POINT('Origin',(-0.172909867005679,0.206065955199005,0.04));
#49704=CARTESIAN_POINT('',(-0.175527068325832,0.211696122508039,0.285));
#49705=CARTESIAN_POINT('',(-0.175527068325832,0.211696122508039,0.1425));
#49706=CARTESIAN_POINT('',(-0.172909867005679,0.206065955199005,0.291));
#49707=CARTESIAN_POINT('',(-0.172909867005679,0.206065955199005,0.04));
#49708=CARTESIAN_POINT('Ctrl Pts',(-0.175527068325832,0.211696122508039,
0.285));
#49709=CARTESIAN_POINT('Ctrl Pts',(-0.174204034570238,0.208849990136741,
0.288035430631142));
#49710=CARTESIAN_POINT('Ctrl Pts',(-0.172909867005679,0.206065955199005,
0.291));
#49711=CARTESIAN_POINT('Origin',(-0.194984655959362,0.221483597452293,0.04));
#49712=CARTESIAN_POINT('',(-0.17800002718254,0.209621063643459,0.285));
#49713=CARTESIAN_POINT('',(-0.17800002718254,0.209621063643459,0.1425));
#49714=CARTESIAN_POINT('Ctrl Pts',(-0.172909867005679,0.206065955199005,
0.291));
#49715=CARTESIAN_POINT('Ctrl Pts',(-0.175426876357856,0.207823904043792,
0.288035430631119));
#49716=CARTESIAN_POINT('Ctrl Pts',(-0.17800002718254,0.209621063643459,
0.285));
#49717=CARTESIAN_POINT('Origin',(-0.141,0.244219163867212,0.04));
#49718=CARTESIAN_POINT('',(-0.138895491103459,0.237345829015656,0.04));
#49719=CARTESIAN_POINT('',(-0.136099771858106,0.238959938274539,0.04));
#49720=CARTESIAN_POINT('Origin',(0.,0.,0.04));
#49721=CARTESIAN_POINT('',(-0.1345,0.232960833618014,0.04));
#49722=CARTESIAN_POINT('',(-0.153562177826491,0.25197749411641,0.04));
#49723=CARTESIAN_POINT('',(-0.1345,0.232960833618014,0.04));
#49724=CARTESIAN_POINT('Origin',(-0.1345,0.232960833618014,0.04));
#49725=CARTESIAN_POINT('',(-0.136099771858106,0.238959938274539,0.285));
#49726=CARTESIAN_POINT('',(-0.136099771858106,0.238959938274539,0.1425));
#49727=CARTESIAN_POINT('',(-0.1345,0.232960833618014,0.291));
#49728=CARTESIAN_POINT('',(-0.1345,0.232960833618014,0.04));
#49729=CARTESIAN_POINT('Ctrl Pts',(-0.136099771858106,0.238959938274539,
0.285));
#49730=CARTESIAN_POINT('Ctrl Pts',(-0.135291063657772,0.235927302648521,
0.288035430631155));
#49731=CARTESIAN_POINT('Ctrl Pts',(-0.1345,0.232960833618014,0.291));
#49732=CARTESIAN_POINT('Origin',(-0.153562177826491,0.25197749411641,0.04));
#49733=CARTESIAN_POINT('',(-0.138895491103459,0.237345829015656,0.285));
#49734=CARTESIAN_POINT('',(-0.138895491103459,0.237345829015656,0.1425));
#49735=CARTESIAN_POINT('Ctrl Pts',(-0.1345,0.232960833618014,0.291));
#49736=CARTESIAN_POINT('Ctrl Pts',(-0.13667350571114,0.235129149356976,
0.288035430631063));
#49737=CARTESIAN_POINT('Ctrl Pts',(-0.138895491103459,0.237345829015656,
0.285));
#49738=CARTESIAN_POINT('Origin',(-0.0964496804178386,0.264993319061626,
0.04));
#49739=CARTESIAN_POINT('',(-0.095570685811709,0.257858961475997,0.04));
#49740=CARTESIAN_POINT('',(-0.09253715269228,0.25896307723613,0.04));
#49741=CARTESIAN_POINT('Origin',(0.,0.,0.04));
#49742=CARTESIAN_POINT('',(-0.0920034185546049,0.252777314991409,0.04));
#49743=CARTESIAN_POINT('',(-0.107473790626574,0.274815182128563,0.04));
#49744=CARTESIAN_POINT('',(-0.0920034185546049,0.252777314991409,0.04));
#49745=CARTESIAN_POINT('Origin',(-0.0920034185546049,0.252777314991409,
0.04));
#49746=CARTESIAN_POINT('',(-0.09253715269228,0.25896307723613,0.285));
#49747=CARTESIAN_POINT('',(-0.09253715269228,0.25896307723613,0.1425));
#49748=CARTESIAN_POINT('',(-0.0920034185546049,0.252777314991409,0.291));
#49749=CARTESIAN_POINT('',(-0.0920034185546049,0.252777314991409,0.04));
#49750=CARTESIAN_POINT('Ctrl Pts',(-0.09253715269228,0.25896307723613,0.285));
#49751=CARTESIAN_POINT('Ctrl Pts',(-0.0922673422366543,0.255836083454338,
0.288035430631132));
#49752=CARTESIAN_POINT('Ctrl Pts',(-0.0920034185546049,0.252777314991409,
0.291));
#49753=CARTESIAN_POINT('Origin',(-0.107473790626574,0.274815182128563,0.04));
#49754=CARTESIAN_POINT('',(-0.095570685811709,0.257858961475997,0.285));
#49755=CARTESIAN_POINT('',(-0.095570685811709,0.257858961475997,0.1425));
#49756=CARTESIAN_POINT('Ctrl Pts',(-0.0920034185546049,0.252777314991409,
0.291));
#49757=CARTESIAN_POINT('Ctrl Pts',(-0.0937673797534821,0.255290114448016,
0.288035430631051));
#49758=CARTESIAN_POINT('Ctrl Pts',(-0.0955706858117089,0.257858961475997,
0.285));
#49759=CARTESIAN_POINT('Origin',(-0.0489687861020744,0.277715786349443,
0.04));
#49760=CARTESIAN_POINT('',(-0.0493420135926708,0.27053717987482,0.04));
#49761=CARTESIAN_POINT('',(-0.0461628389679574,0.271097754137541,0.04));
#49762=CARTESIAN_POINT('Origin',(0.,0.,0.04));
#49763=CARTESIAN_POINT('',(-0.0467113597924043,0.264913285560284,0.04));
#49764=CARTESIAN_POINT('',(-0.0581198666828299,0.289302749894933,0.04));
#49765=CARTESIAN_POINT('',(-0.0467113597924043,0.264913285560284,0.04));
#49766=CARTESIAN_POINT('Origin',(-0.0467113597924043,0.264913285560284,
0.04));
#49767=CARTESIAN_POINT('',(-0.0461628389679574,0.271097754137541,0.285));
#49768=CARTESIAN_POINT('',(-0.0461628389679574,0.271097754137541,0.1425));
#49769=CARTESIAN_POINT('',(-0.0467113597924043,0.264913285560284,0.291));
#49770=CARTESIAN_POINT('',(-0.0467113597924043,0.264913285560284,0.04));
#49771=CARTESIAN_POINT('Ctrl Pts',(-0.0461628389679575,0.271097754137541,
0.285));
#49772=CARTESIAN_POINT('Ctrl Pts',(-0.0464401243112017,0.267971414323629,
0.288035430631178));
#49773=CARTESIAN_POINT('Ctrl Pts',(-0.0467113597924043,0.264913285560284,
0.291));
#49774=CARTESIAN_POINT('Origin',(-0.0581198666828299,0.289302749894933,
0.04));
#49775=CARTESIAN_POINT('',(-0.0493420135926708,0.27053717987482,0.285));
#49776=CARTESIAN_POINT('',(-0.0493420135926708,0.27053717987482,0.1425));
#49777=CARTESIAN_POINT('Ctrl Pts',(-0.0467113597924043,0.264913285560284,
0.291));
#49778=CARTESIAN_POINT('Ctrl Pts',(-0.0480121794105643,0.267694218594523,
0.288035430631107));
#49779=CARTESIAN_POINT('Ctrl Pts',(-0.0493420135926707,0.27053717987482,
0.285));
#49780=CARTESIAN_POINT('Origin',(1.38777878078145E-17,0.282,0.04));
#49781=CARTESIAN_POINT('',(-0.0016141092588829,0.274995262961565,0.04));
#49782=CARTESIAN_POINT('',(0.00161410925888293,0.274995262961565,0.04));
#49783=CARTESIAN_POINT('Origin',(0.,0.,0.04));
#49784=CARTESIAN_POINT('',(2.08166817117217E-17,0.269,0.04));
#49785=CARTESIAN_POINT('',(-0.00699999999999999,0.295,0.04));
#49786=CARTESIAN_POINT('',(2.08166817117217E-17,0.269,0.04));
#49787=CARTESIAN_POINT('Origin',(2.08166817117217E-17,0.269,0.04));
#49788=CARTESIAN_POINT('',(0.00161410925888295,0.274995262961565,0.285));
#49789=CARTESIAN_POINT('',(0.00161410925888295,0.274995262961565,0.1425));
#49790=CARTESIAN_POINT('',(2.08166817117217E-17,0.269,0.291));
#49791=CARTESIAN_POINT('',(2.08166817117217E-17,0.269,0.04));
#49792=CARTESIAN_POINT('Ctrl Pts',(0.00161410925888293,0.274995262961565,
0.285));
#49793=CARTESIAN_POINT('Ctrl Pts',(0.000798153291618306,0.271964569368868,
0.288035430631132));
#49794=CARTESIAN_POINT('Ctrl Pts',(2.08166817117217E-17,0.269,0.291));
#49795=CARTESIAN_POINT('Origin',(-0.00699999999999999,0.295,0.04));
#49796=CARTESIAN_POINT('',(-0.00161410925888292,0.274995262961565,0.285));
#49797=CARTESIAN_POINT('',(-0.00161410925888292,0.274995262961565,0.1425));
#49798=CARTESIAN_POINT('Ctrl Pts',(2.08166817117217E-17,0.269,0.291));
#49799=CARTESIAN_POINT('Ctrl Pts',(-0.000798153291634971,0.27196456936893,
0.28803543063107));
#49800=CARTESIAN_POINT('Ctrl Pts',(-0.00161410925888289,0.274995262961565,
0.285));
#49801=CARTESIAN_POINT('Origin',(0.0489687861020744,0.277715786349443,0.04));
#49802=CARTESIAN_POINT('',(0.0461628389679574,0.271097754137541,0.04));
#49803=CARTESIAN_POINT('',(0.0493420135926708,0.27053717987482,0.04));
#49804=CARTESIAN_POINT('Origin',(0.,0.,0.04));
#49805=CARTESIAN_POINT('',(0.0467113597924043,0.264913285560284,0.04));
#49806=CARTESIAN_POINT('',(0.044332558140659,0.29173382438227,0.04));
#49807=CARTESIAN_POINT('',(0.0467113597924043,0.264913285560284,0.04));
#49808=CARTESIAN_POINT('Origin',(0.0467113597924043,0.264913285560284,0.04));
#49809=CARTESIAN_POINT('',(0.0493420135926708,0.27053717987482,0.285));
#49810=CARTESIAN_POINT('',(0.0493420135926708,0.27053717987482,0.1425));
#49811=CARTESIAN_POINT('',(0.0467113597924043,0.264913285560284,0.291));
#49812=CARTESIAN_POINT('',(0.0467113597924043,0.264913285560284,0.04));
#49813=CARTESIAN_POINT('Ctrl Pts',(0.0493420135926708,0.27053717987482,
0.285));
#49814=CARTESIAN_POINT('Ctrl Pts',(0.048012179410518,0.267694218594424,
0.288035430631212));
#49815=CARTESIAN_POINT('Ctrl Pts',(0.0467113597924043,0.264913285560284,
0.291));
#49816=CARTESIAN_POINT('Origin',(0.044332558140659,0.29173382438227,0.04));
#49817=CARTESIAN_POINT('',(0.0461628389679575,0.271097754137541,0.285));
#49818=CARTESIAN_POINT('',(0.0461628389679575,0.271097754137541,0.1425));
#49819=CARTESIAN_POINT('Ctrl Pts',(0.0467113597924043,0.264913285560284,
0.291));
#49820=CARTESIAN_POINT('Ctrl Pts',(0.0464401243111968,0.267971414323684,
0.288035430631124));
#49821=CARTESIAN_POINT('Ctrl Pts',(0.0461628389679575,0.271097754137541,
0.285));
#49822=CARTESIAN_POINT('Origin',(0.0964496804178386,0.264993319061626,0.04));
#49823=CARTESIAN_POINT('',(0.09253715269228,0.25896307723613,0.04));
#49824=CARTESIAN_POINT('',(0.095570685811709,0.257858961475997,0.04));
#49825=CARTESIAN_POINT('Origin',(0.,0.,0.04));
#49826=CARTESIAN_POINT('',(0.0920034185546049,0.252777314991409,0.04));
#49827=CARTESIAN_POINT('',(0.094318093935571,0.279603464135123,0.04));
#49828=CARTESIAN_POINT('',(0.0920034185546049,0.252777314991409,0.04));
#49829=CARTESIAN_POINT('Origin',(0.0920034185546049,0.252777314991409,0.04));
#49830=CARTESIAN_POINT('',(0.095570685811709,0.257858961475997,0.285));
#49831=CARTESIAN_POINT('',(0.095570685811709,0.257858961475997,0.1425));
#49832=CARTESIAN_POINT('',(0.0920034185546049,0.252777314991409,0.291));
#49833=CARTESIAN_POINT('',(0.0920034185546049,0.252777314991409,0.04));
#49834=CARTESIAN_POINT('Ctrl Pts',(0.095570685811709,0.257858961475997,
0.285));
#49835=CARTESIAN_POINT('Ctrl Pts',(0.0937673797534397,0.255290114447956,
0.288035430631122));
#49836=CARTESIAN_POINT('Ctrl Pts',(0.0920034185546049,0.252777314991409,
0.291));
#49837=CARTESIAN_POINT('Origin',(0.094318093935571,0.279603464135123,0.04));
#49838=CARTESIAN_POINT('',(0.09253715269228,0.25896307723613,0.285));
#49839=CARTESIAN_POINT('',(0.09253715269228,0.25896307723613,0.1425));
#49840=CARTESIAN_POINT('Ctrl Pts',(0.0920034185546049,0.252777314991409,
0.291));
#49841=CARTESIAN_POINT('Ctrl Pts',(0.0922673422366571,0.255836083454369,
0.288035430631101));
#49842=CARTESIAN_POINT('Ctrl Pts',(0.09253715269228,0.25896307723613,0.285));
#49843=CARTESIAN_POINT('Origin',(0.141,0.244219163867212,0.04));
#49844=CARTESIAN_POINT('',(0.136099771858106,0.238959938274539,0.04));
#49845=CARTESIAN_POINT('',(0.138895491103459,0.237345829015656,0.04));
#49846=CARTESIAN_POINT('Origin',(0.,0.,0.04));
#49847=CARTESIAN_POINT('',(0.1345,0.232960833618014,0.04));
#49848=CARTESIAN_POINT('',(0.141437822173509,0.258977494116409,0.04));
#49849=CARTESIAN_POINT('',(0.1345,0.232960833618014,0.04));
#49850=CARTESIAN_POINT('Origin',(0.1345,0.232960833618014,0.04));
#49851=CARTESIAN_POINT('',(0.138895491103459,0.237345829015656,0.285));
#49852=CARTESIAN_POINT('',(0.138895491103459,0.237345829015656,0.1425));
#49853=CARTESIAN_POINT('',(0.1345,0.232960833618014,0.291));
#49854=CARTESIAN_POINT('',(0.1345,0.232960833618014,0.04));
#49855=CARTESIAN_POINT('Ctrl Pts',(0.138895491103459,0.237345829015656,
0.285));
#49856=CARTESIAN_POINT('Ctrl Pts',(0.136673505711127,0.235129149356963,
0.288035430631081));
#49857=CARTESIAN_POINT('Ctrl Pts',(0.1345,0.232960833618014,0.291));
#49858=CARTESIAN_POINT('Origin',(0.141437822173509,0.258977494116409,0.04));
#49859=CARTESIAN_POINT('',(0.136099771858106,0.238959938274539,0.285));
#49860=CARTESIAN_POINT('',(0.136099771858106,0.238959938274539,0.1425));
#49861=CARTESIAN_POINT('Ctrl Pts',(0.1345,0.232960833618014,0.291));
#49862=CARTESIAN_POINT('Ctrl Pts',(0.1352910636578,0.235927302648627,0.28803543063105));
#49863=CARTESIAN_POINT('Ctrl Pts',(0.136099771858106,0.238959938274539,
0.285));
#49864=CARTESIAN_POINT('Origin',(0.181266105931604,0.216024532959552,0.04));
#49865=CARTESIAN_POINT('',(0.175527068325832,0.211696122508039,0.04));
#49866=CARTESIAN_POINT('',(0.17800002718254,0.209621063643459,0.04));
#49867=CARTESIAN_POINT('Origin',(0.,0.,0.04));
#49868=CARTESIAN_POINT('',(0.172909867005679,0.206065955199005,0.04));
#49869=CARTESIAN_POINT('',(0.184260033755696,0.230482623987904,0.04));
#49870=CARTESIAN_POINT('',(0.172909867005679,0.206065955199005,0.04));
#49871=CARTESIAN_POINT('Origin',(0.172909867005679,0.206065955199005,0.04));
#49872=CARTESIAN_POINT('',(0.17800002718254,0.209621063643459,0.285));
#49873=CARTESIAN_POINT('',(0.17800002718254,0.209621063643459,0.1425));
#49874=CARTESIAN_POINT('',(0.172909867005679,0.206065955199005,0.291));
#49875=CARTESIAN_POINT('',(0.172909867005679,0.206065955199005,0.04));
#49876=CARTESIAN_POINT('Ctrl Pts',(0.17800002718254,0.209621063643459,0.285));
#49877=CARTESIAN_POINT('Ctrl Pts',(0.175426876357847,0.207823904043786,
0.28803543063113));
#49878=CARTESIAN_POINT('Ctrl Pts',(0.172909867005679,0.206065955199005,
0.291));
#49879=CARTESIAN_POINT('Origin',(0.184260033755696,0.230482623987904,0.04));
#49880=CARTESIAN_POINT('',(0.175527068325832,0.211696122508039,0.285));
#49881=CARTESIAN_POINT('',(0.175527068325832,0.211696122508039,0.1425));
#49882=CARTESIAN_POINT('Ctrl Pts',(0.172909867005679,0.206065955199005,
0.291));
#49883=CARTESIAN_POINT('Ctrl Pts',(0.174204034570257,0.208849990136781,
0.288035430631099));
#49884=CARTESIAN_POINT('Ctrl Pts',(0.175527068325832,0.211696122508039,
0.285));
#49885=CARTESIAN_POINT('Origin',(0.216024532959552,0.181266105931604,0.04));
#49886=CARTESIAN_POINT('',(0.209621063643459,0.17800002718254,0.04));
#49887=CARTESIAN_POINT('',(0.211696122508039,0.175527068325832,0.04));
#49888=CARTESIAN_POINT('Origin',(0.,0.,0.04));
#49889=CARTESIAN_POINT('',(0.206065955199005,0.172909867005679,0.04));
#49890=CARTESIAN_POINT('',(0.221483597452293,0.194984655959362,0.04));
#49891=CARTESIAN_POINT('',(0.206065955199005,0.172909867005679,0.04));
#49892=CARTESIAN_POINT('Origin',(0.206065955199005,0.172909867005679,0.04));
#49893=CARTESIAN_POINT('',(0.211696122508039,0.175527068325832,0.285));
#49894=CARTESIAN_POINT('',(0.211696122508039,0.175527068325832,0.1425));
#49895=CARTESIAN_POINT('',(0.206065955199005,0.172909867005679,0.291));
#49896=CARTESIAN_POINT('',(0.206065955199005,0.172909867005679,0.04));
#49897=CARTESIAN_POINT('Ctrl Pts',(0.211696122508039,0.175527068325832,
0.285));
#49898=CARTESIAN_POINT('Ctrl Pts',(0.208849990136656,0.174204034570199,
0.288035430631232));
#49899=CARTESIAN_POINT('Ctrl Pts',(0.206065955199005,0.172909867005679,
0.291));
#49900=CARTESIAN_POINT('Origin',(0.221483597452293,0.194984655959362,0.04));
#49901=CARTESIAN_POINT('',(0.209621063643459,0.17800002718254,0.285));
#49902=CARTESIAN_POINT('',(0.209621063643459,0.17800002718254,0.1425));
#49903=CARTESIAN_POINT('Ctrl Pts',(0.206065955199005,0.172909867005679,
0.291));
#49904=CARTESIAN_POINT('Ctrl Pts',(0.207823904043843,0.175426876357928,
0.288035430631034));
#49905=CARTESIAN_POINT('Ctrl Pts',(0.209621063643459,0.17800002718254,0.285));
#49906=CARTESIAN_POINT('Origin',(0.244219163867212,0.141,0.04));
#49907=CARTESIAN_POINT('',(0.237345829015656,0.138895491103459,0.04));
#49908=CARTESIAN_POINT('',(0.238959938274539,0.136099771858106,0.04));
#49909=CARTESIAN_POINT('Origin',(0.,0.,0.04));
#49910=CARTESIAN_POINT('',(0.232960833618014,0.1345,0.04));
#49911=CARTESIAN_POINT('',(0.25197749411641,0.153562177826491,0.04));
#49912=CARTESIAN_POINT('',(0.232960833618014,0.1345,0.04));
#49913=CARTESIAN_POINT('Origin',(0.232960833618014,0.1345,0.04));
#49914=CARTESIAN_POINT('',(0.238959938274539,0.136099771858106,0.285));
#49915=CARTESIAN_POINT('',(0.238959938274539,0.136099771858106,0.1425));
#49916=CARTESIAN_POINT('',(0.232960833618014,0.1345,0.291));
#49917=CARTESIAN_POINT('',(0.232960833618014,0.1345,0.04));
#49918=CARTESIAN_POINT('Ctrl Pts',(0.238959938274539,0.136099771858106,
0.285));
#49919=CARTESIAN_POINT('Ctrl Pts',(0.235927302648562,0.135291063657783,
0.288035430631114));
#49920=CARTESIAN_POINT('Ctrl Pts',(0.232960833618014,0.1345,0.291));
#49921=CARTESIAN_POINT('Origin',(0.25197749411641,0.153562177826491,0.04));
#49922=CARTESIAN_POINT('',(0.237345829015656,0.138895491103459,0.285));
#49923=CARTESIAN_POINT('',(0.237345829015656,0.138895491103459,0.1425));
#49924=CARTESIAN_POINT('Ctrl Pts',(0.232960833618014,0.1345,0.291));
#49925=CARTESIAN_POINT('Ctrl Pts',(0.235129149356992,0.136673505711156,
0.288035430631041));
#49926=CARTESIAN_POINT('Ctrl Pts',(0.237345829015656,0.138895491103459,
0.285));
#49927=CARTESIAN_POINT('Origin',(0.264993319061626,0.0964496804178386,0.04));
#49928=CARTESIAN_POINT('',(0.257858961475997,0.095570685811709,0.04));
#49929=CARTESIAN_POINT('',(0.25896307723613,0.09253715269228,0.04));
#49930=CARTESIAN_POINT('Origin',(0.,0.,0.04));
#49931=CARTESIAN_POINT('',(0.252777314991409,0.0920034185546049,0.04));
#49932=CARTESIAN_POINT('',(0.274815182128563,0.107473790626574,0.04));
#49933=CARTESIAN_POINT('',(0.252777314991409,0.0920034185546049,0.04));
#49934=CARTESIAN_POINT('Origin',(0.252777314991409,0.0920034185546049,0.04));
#49935=CARTESIAN_POINT('',(0.25896307723613,0.09253715269228,0.285));
#49936=CARTESIAN_POINT('',(0.25896307723613,0.09253715269228,0.1425));
#49937=CARTESIAN_POINT('',(0.252777314991409,0.0920034185546049,0.291));
#49938=CARTESIAN_POINT('',(0.252777314991409,0.0920034185546049,0.04));
#49939=CARTESIAN_POINT('Ctrl Pts',(0.25896307723613,0.09253715269228,0.285));
#49940=CARTESIAN_POINT('Ctrl Pts',(0.255836083454338,0.0922673422366543,
0.288035430631132));
#49941=CARTESIAN_POINT('Ctrl Pts',(0.252777314991409,0.0920034185546049,
0.291));
#49942=CARTESIAN_POINT('Origin',(0.274815182128563,0.107473790626574,0.04));
#49943=CARTESIAN_POINT('',(0.257858961475997,0.095570685811709,0.285));
#49944=CARTESIAN_POINT('',(0.257858961475997,0.095570685811709,0.1425));
#49945=CARTESIAN_POINT('Ctrl Pts',(0.252777314991409,0.0920034185546049,
0.291));
#49946=CARTESIAN_POINT('Ctrl Pts',(0.255290114448016,0.0937673797534821,
0.288035430631051));
#49947=CARTESIAN_POINT('Ctrl Pts',(0.257858961475997,0.0955706858117089,
0.285));
#49948=CARTESIAN_POINT('Origin',(0.277715786349443,0.0489687861020744,0.04));
#49949=CARTESIAN_POINT('',(0.27053717987482,0.0493420135926708,0.04));
#49950=CARTESIAN_POINT('',(0.271097754137541,0.0461628389679574,0.04));
#49951=CARTESIAN_POINT('Origin',(0.,0.,0.04));
#49952=CARTESIAN_POINT('',(0.264913285560284,0.0467113597924043,0.04));
#49953=CARTESIAN_POINT('',(0.289302749894933,0.0581198666828299,0.04));
#49954=CARTESIAN_POINT('',(0.264913285560284,0.0467113597924043,0.04));
#49955=CARTESIAN_POINT('Origin',(0.264913285560284,0.0467113597924043,0.04));
#49956=CARTESIAN_POINT('',(0.271097754137541,0.0461628389679574,0.285));
#49957=CARTESIAN_POINT('',(0.271097754137541,0.0461628389679574,0.1425));
#49958=CARTESIAN_POINT('',(0.264913285560284,0.0467113597924043,0.291));
#49959=CARTESIAN_POINT('',(0.264913285560284,0.0467113597924043,0.04));
#49960=CARTESIAN_POINT('Ctrl Pts',(0.271097754137541,0.0461628389679574,
0.285));
#49961=CARTESIAN_POINT('Ctrl Pts',(0.267971414323704,0.0464401243111951,
0.288035430631105));
#49962=CARTESIAN_POINT('Ctrl Pts',(0.264913285560284,0.0467113597924043,
0.291));
#49963=CARTESIAN_POINT('Origin',(0.289302749894933,0.0581198666828299,0.04));
#49964=CARTESIAN_POINT('',(0.27053717987482,0.0493420135926708,0.285));
#49965=CARTESIAN_POINT('',(0.27053717987482,0.0493420135926708,0.1425));
#49966=CARTESIAN_POINT('Ctrl Pts',(0.264913285560284,0.0467113597924043,
0.291));
#49967=CARTESIAN_POINT('Ctrl Pts',(0.26769421859449,0.0480121794105489,
0.288035430631142));
#49968=CARTESIAN_POINT('Ctrl Pts',(0.27053717987482,0.0493420135926708,
0.285));
#49969=CARTESIAN_POINT('Origin',(0.,0.,0.1425));
#49970=CARTESIAN_POINT('Origin',(0.,0.,0.285));
#49971=CARTESIAN_POINT('Origin',(0.,0.,0.285));
#49972=CARTESIAN_POINT('Origin',(0.,0.,0.285));
#49973=CARTESIAN_POINT('Origin',(0.,0.,0.285));
#49974=CARTESIAN_POINT('Origin',(0.,0.,0.285));
#49975=CARTESIAN_POINT('Origin',(0.,0.,0.285));
#49976=CARTESIAN_POINT('Origin',(0.,0.,0.285));
#49977=CARTESIAN_POINT('Origin',(0.,0.,0.285));
#49978=CARTESIAN_POINT('Origin',(0.,0.,0.285));
#49979=CARTESIAN_POINT('Origin',(0.,0.,0.285));
#49980=CARTESIAN_POINT('Origin',(0.,0.,0.285));
#49981=CARTESIAN_POINT('Origin',(0.,0.,0.285));
#49982=CARTESIAN_POINT('Origin',(0.,0.,0.285));
#49983=CARTESIAN_POINT('Origin',(0.,0.,0.285));
#49984=CARTESIAN_POINT('Origin',(0.,0.,0.285));
#49985=CARTESIAN_POINT('Origin',(0.,0.,0.285));
#49986=CARTESIAN_POINT('Origin',(0.,0.,0.285));
#49987=CARTESIAN_POINT('',(-0.275,-3.36777869765522E-17,0.));
#49988=CARTESIAN_POINT('',(-0.275,-3.36777869765522E-17,0.1425));
#49989=CARTESIAN_POINT('Origin',(0.,0.,0.));
#49990=CARTESIAN_POINT('Origin',(0.,0.,0.285));
#49991=CARTESIAN_POINT('Origin',(0.,0.,0.285));
#49992=CARTESIAN_POINT('Origin',(0.,0.,0.285));
#49993=CARTESIAN_POINT('Origin',(0.,0.,0.285));
#49994=CARTESIAN_POINT('Origin',(0.,0.,0.285));
#49995=CARTESIAN_POINT('Origin',(0.,0.,0.285));
#49996=CARTESIAN_POINT('Origin',(0.,0.,0.285));
#49997=CARTESIAN_POINT('Origin',(0.,0.,0.285));
#49998=CARTESIAN_POINT('Origin',(0.,0.,0.285));
#49999=CARTESIAN_POINT('Origin',(0.,0.,0.285));
#50000=CARTESIAN_POINT('Origin',(0.,0.,0.285));
#50001=CARTESIAN_POINT('Origin',(0.,0.,0.285));
#50002=CARTESIAN_POINT('Origin',(0.,0.,0.285));
#50003=CARTESIAN_POINT('Origin',(0.,0.,0.285));
#50004=CARTESIAN_POINT('Origin',(0.,0.,0.285));
#50005=CARTESIAN_POINT('Origin',(0.,0.,0.285));
#50006=CARTESIAN_POINT('Origin',(0.,0.,0.285));
#50007=CARTESIAN_POINT('',(0.274995262961565,0.00161410925888293,0.285));
#50008=CARTESIAN_POINT('Origin',(0.,0.,0.285));
#50009=CARTESIAN_POINT('',(0.274995262961565,0.00161410925888293,0.04));
#50010=CARTESIAN_POINT('',(0.274995262961565,0.00161410925888293,0.1425));
#50011=CARTESIAN_POINT('',(0.274995262961565,-0.00161410925888293,0.04));
#50012=CARTESIAN_POINT('Origin',(0.,0.,0.04));
#50013=CARTESIAN_POINT('',(0.274995262961565,-0.00161410925888293,0.285));
#50014=CARTESIAN_POINT('',(0.274995262961565,-0.00161410925888293,0.1425));
#50015=CARTESIAN_POINT('Origin',(0.,0.,0.285));
#50016=CARTESIAN_POINT('Origin',(0.269,0.,0.04));
#50017=CARTESIAN_POINT('',(0.269,0.,0.04));
#50018=CARTESIAN_POINT('',(0.269,0.,0.04));
#50019=CARTESIAN_POINT('',(0.269,0.,0.291));
#50020=CARTESIAN_POINT('',(0.269,0.,0.04));
#50021=CARTESIAN_POINT('Ctrl Pts',(0.274995262961565,-0.00161410925888293,
0.285));
#50022=CARTESIAN_POINT('Ctrl Pts',(0.271964569368838,-0.000798153291610108,
0.288035430631162));
#50023=CARTESIAN_POINT('Ctrl Pts',(0.269,0.,0.291));
#50024=CARTESIAN_POINT('Origin',(0.295,0.007,0.04));
#50025=CARTESIAN_POINT('Ctrl Pts',(0.269,0.,0.291));
#50026=CARTESIAN_POINT('Ctrl Pts',(0.27196456936891,0.000798153291629561,
0.28803543063109));
#50027=CARTESIAN_POINT('Ctrl Pts',(0.274995262961565,0.00161410925888293,
0.285));
#50028=CARTESIAN_POINT('',(0.295,0.007,0.04));
#50029=CARTESIAN_POINT('Origin',(0.282,0.,0.04));
#50030=CARTESIAN_POINT('Origin',(0.,0.,0.2925));
#50031=CARTESIAN_POINT('',(-0.26,-3.18408167778312E-17,0.3));
#50032=CARTESIAN_POINT('Origin',(0.,0.,0.3));
#50033=CARTESIAN_POINT('',(-0.2675,-3.27593018771917E-17,0.2925));
#50034=CARTESIAN_POINT('Origin',(0.,0.,0.134415608175648));
#50035=CARTESIAN_POINT('',(0.,0.,0.0978312163512968));
#50036=CARTESIAN_POINT('',(-0.113891921086774,1.39477376607661E-17,0.17));
#50037=CARTESIAN_POINT('',(-0.0577350269189626,-7.07050159149938E-18,0.134415608175648));
#50038=CARTESIAN_POINT('Origin',(0.,0.,0.17));
#50039=CARTESIAN_POINT('Origin',(0.,0.144337567297406,0.3));
#50040=CARTESIAN_POINT('',(8.83812698937423E-18,0.144337567297406,0.3));
#50041=CARTESIAN_POINT('',(0.125,0.0721687836487032,0.3));
#50042=CARTESIAN_POINT('',(0.03125,0.126295371385231,0.3));
#50043=CARTESIAN_POINT('',(1.38777878078145E-17,0.144337567297406,0.17));
#50044=CARTESIAN_POINT('',(8.83812698937423E-18,0.144337567297406,0.3));
#50045=CARTESIAN_POINT('',(0.125,0.0721687836487032,0.17));
#50046=CARTESIAN_POINT('',(0.125,0.0721687836487032,0.17));
#50047=CARTESIAN_POINT('',(0.125,0.0721687836487032,0.3));
#50048=CARTESIAN_POINT('Origin',(-0.125,0.0721687836487032,0.3));
#50049=CARTESIAN_POINT('',(-0.125,0.0721687836487032,0.3));
#50050=CARTESIAN_POINT('',(-0.09375,0.090210979560879,0.3));
#50051=CARTESIAN_POINT('',(-0.125,0.0721687836487032,0.17));
#50052=CARTESIAN_POINT('',(-0.125,0.0721687836487032,0.3));
#50053=CARTESIAN_POINT('',(8.83812698937423E-18,0.144337567297406,0.17));
#50054=CARTESIAN_POINT('Origin',(-0.125,-0.0721687836487032,0.3));
#50055=CARTESIAN_POINT('',(-0.125,-0.0721687836487032,0.3));
#50056=CARTESIAN_POINT('',(-0.125,-0.0360843918243516,0.3));
#50057=CARTESIAN_POINT('',(-0.125,-0.0721687836487032,0.17));
#50058=CARTESIAN_POINT('',(-0.125,-0.0721687836487032,0.3));
#50059=CARTESIAN_POINT('',(-0.125,0.0721687836487032,0.17));
#50060=CARTESIAN_POINT('Origin',(-2.77555756156289E-17,-0.144337567297406,
0.3));
#50061=CARTESIAN_POINT('',(-2.65143809681227E-17,-0.144337567297406,0.3));
#50062=CARTESIAN_POINT('',(-0.03125,-0.126295371385231,0.3));
#50063=CARTESIAN_POINT('',(-2.77555756156289E-17,-0.144337567297406,0.17));
#50064=CARTESIAN_POINT('',(-2.65143809681227E-17,-0.144337567297406,0.3));
#50065=CARTESIAN_POINT('',(-0.125,-0.0721687836487032,0.17));
#50066=CARTESIAN_POINT('Origin',(0.125,-0.0721687836487033,0.3));
#50067=CARTESIAN_POINT('',(0.125,-0.0721687836487033,0.3));
#50068=CARTESIAN_POINT('',(0.09375,-0.0902109795608791,0.3));
#50069=CARTESIAN_POINT('',(0.125,-0.0721687836487033,0.17));
#50070=CARTESIAN_POINT('',(0.125,-0.0721687836487033,0.3));
#50071=CARTESIAN_POINT('',(-2.65143809681227E-17,-0.144337567297406,0.17));
#50072=CARTESIAN_POINT('Origin',(0.125,0.0721687836487032,0.3));
#50073=CARTESIAN_POINT('',(0.125,0.0360843918243516,0.3));
#50074=CARTESIAN_POINT('',(0.125,-0.0721687836487033,0.17));
#50075=CARTESIAN_POINT('Origin',(0.,0.,0.17));
#50076=CARTESIAN_POINT('Origin',(0.114,0.,-3.));
#50077=CARTESIAN_POINT('',(-0.114,-1.39609735102798E-17,-3.));
#50078=CARTESIAN_POINT('Origin',(0.,0.,-3.));
#50079=CARTESIAN_POINT('Origin',(0.,0.,-2.982));
#50080=CARTESIAN_POINT('',(-0.132,-1.61653377487451E-17,-2.982));
#50081=CARTESIAN_POINT('Origin',(0.,0.,-1.487));
#50082=CARTESIAN_POINT('Origin',(0.,0.,-0.0136500000000002));
#50083=CARTESIAN_POINT('Origin',(0.,0.,-0.005));
#50084=CARTESIAN_POINT('',(-0.16,-1.95943487863577E-17,-2.60208521396521E-18));
#50085=CARTESIAN_POINT('Origin',(0.,0.,0.));
#50086=CARTESIAN_POINT('',(-0.155,-1.8982025386784E-17,-0.005));
#50087=CARTESIAN_POINT('Origin',(0.275,0.,0.));
#50088=CARTESIAN_POINT('Origin',(0.,0.,0.3));
#50089=CARTESIAN_POINT('',(0.,0.,0.));
#50090=CARTESIAN_POINT('Origin',(0.,0.,-0.775));
#50091=CARTESIAN_POINT('',(-0.245447138551752,4.00299569890614E-5,-1.43916725037879));
#50092=CARTESIAN_POINT('',(-0.245435809527805,6.93114097173611E-5,-1.45073274962121));
#50093=CARTESIAN_POINT('',(-0.24505,-3.00099698131059E-17,-0.775));
#50094=CARTESIAN_POINT('',(-0.232143106254475,-0.0797426101647723,-1.51495));
#50095=CARTESIAN_POINT('Ctrl Pts',(-0.245447138551752,4.00299569890614E-5,
-1.43916725037879));
#50096=CARTESIAN_POINT('Ctrl Pts',(-0.245452129536357,0.0022198044307001,
-1.43928101890267));
#50097=CARTESIAN_POINT('Ctrl Pts',(-0.245425591838023,0.00439945516314897,
-1.43939478742655));
#50098=CARTESIAN_POINT('Ctrl Pts',(-0.24536715191998,0.00657825184837683,
-1.43950855595043));
#50099=CARTESIAN_POINT('Ctrl Pts',(-0.243189299218486,0.0877744342843084,
-1.44374831355743));
#50100=CARTESIAN_POINT('Ctrl Pts',(-0.196705837434329,0.167784521123834,
-1.44798807116442));
#50101=CARTESIAN_POINT('Ctrl Pts',(-0.127250682360293,0.209893324947318,
-1.45222782877142));
#50102=CARTESIAN_POINT('Ctrl Pts',(-0.0577955272862565,0.252002128770801,
-1.45646758637841));
#50103=CARTESIAN_POINT('Ctrl Pts',(0.0346313210776596,0.25620964957824,
-1.46070734398541));
#50104=CARTESIAN_POINT('Ctrl Pts',(0.10763278442824,0.220593165770989,-1.4649471015924));
#50105=CARTESIAN_POINT('Ctrl Pts',(0.18063424777882,0.184976681963739,-1.4691868591994));
#50106=CARTESIAN_POINT('Ctrl Pts',(0.234210326116065,0.109536193541798,
-1.47342661680639));
#50107=CARTESIAN_POINT('Ctrl Pts',(0.243757317623978,0.0288712065516735,
-1.47766637441339));
#50108=CARTESIAN_POINT('Ctrl Pts',(0.253304309131892,-0.0517937804384507,
-1.48190613202038));
#50109=CARTESIAN_POINT('Ctrl Pts',(0.218822213810474,-0.137683265996759,
-1.48614588962738));
#50110=CARTESIAN_POINT('Ctrl Pts',(0.156173226820107,-0.189360044779689,
-1.49038564723437));
#50111=CARTESIAN_POINT('Ctrl Pts',(0.0935242398297384,-0.241036823562619,
-1.49462540484137));
#50112=CARTESIAN_POINT('Ctrl Pts',(0.00270836117041977,-0.258500895570172,
-1.49886516244836));
#50113=CARTESIAN_POINT('Ctrl Pts',(-0.074683455425355,-0.233793976655611,
-1.50310492005536));
#50114=CARTESIAN_POINT('Ctrl Pts',(-0.146756149166573,-0.210785158946641,
-1.50705328003691));
#50115=CARTESIAN_POINT('Ctrl Pts',(-0.20718663426269,-0.151202949907839,
-1.51100164001845));
#50116=CARTESIAN_POINT('Ctrl Pts',(-0.232146081401957,-0.0797429895224405,
-1.51495));
#50117=CARTESIAN_POINT('',(-0.24505,-3.00099698131059E-17,-1.51495));
#50118=CARTESIAN_POINT('Origin',(0.,0.,-1.51495));
#50119=CARTESIAN_POINT('',(-0.24505,-3.00099698131059E-17,-1.54495));
#50120=CARTESIAN_POINT('',(-0.24505,-3.00099698131059E-17,-0.775));
#50121=CARTESIAN_POINT('Origin',(0.,0.,-1.54495));
#50122=CARTESIAN_POINT('',(-0.0796899944392842,-0.231730462577251,-1.51495));
#50123=CARTESIAN_POINT('Origin',(0.,0.,-1.51495));
#50124=CARTESIAN_POINT('Ctrl Pts',(-0.079689994439284,-0.231730462577251,
-1.51495));
#50125=CARTESIAN_POINT('Ctrl Pts',(-0.00252611781080675,-0.258266416594893,
-1.510710242393));
#50126=CARTESIAN_POINT('Ctrl Pts',(0.0882646015602411,-0.242994367587768,
-1.50647048478601));
#50127=CARTESIAN_POINT('Ctrl Pts',(0.151921953058853,-0.192764344174053,
-1.50223072717901));
#50128=CARTESIAN_POINT('Ctrl Pts',(0.215579304557466,-0.142534320760337,
-1.49799096957202));
#50129=CARTESIAN_POINT('Ctrl Pts',(0.252103288183642,-0.0573463229400297,
-1.49375121196502));
#50130=CARTESIAN_POINT('Ctrl Pts',(0.24437106297374,0.0235286269972124,
-1.48951145435803));
#50131=CARTESIAN_POINT('Ctrl Pts',(0.236638837763837,0.104403576934455,
-1.48527169675103));
#50132=CARTESIAN_POINT('Ctrl Pts',(0.184650403717856,0.180965478988632,
-1.48103193914404));
#50133=CARTESIAN_POINT('Ctrl Pts',(0.112428881394831,0.218167306952772,
-1.47679218153704));
#50134=CARTESIAN_POINT('Ctrl Pts',(0.0402073590718059,0.255369134916912,
-1.47255242393005));
#50135=CARTESIAN_POINT('Ctrl Pts',(-0.052247251528263,0.253210888791013,
-1.46831266632305));
#50136=CARTESIAN_POINT('Ctrl Pts',(-0.122600130208318,0.212641738373403,
-1.46407290871606));
#50137=CARTESIAN_POINT('Ctrl Pts',(-0.192953008888373,0.172072587955792,
-1.45983315110906));
#50138=CARTESIAN_POINT('Ctrl Pts',(-0.241204155648414,0.0930925332464675,
-1.45559339350207));
#50139=CARTESIAN_POINT('Ctrl Pts',(-0.245169531263596,0.0119613979719827,
-1.45135363589507));
#50140=CARTESIAN_POINT('Ctrl Pts',(-0.245363099506438,0.00800101368085023,
-1.45114667380378));
#50141=CARTESIAN_POINT('Ctrl Pts',(-0.245451140707558,0.00403550365378323,
-1.45093971171249));
#50142=CARTESIAN_POINT('Ctrl Pts',(-0.245435809527805,6.93114097173611E-5,
-1.45073274962121));
#50143=CARTESIAN_POINT('Origin',(0.,0.,-0.775));
#50144=CARTESIAN_POINT('',(-0.244854737116733,0.000201854273987251,-1.35916725037879));
#50145=CARTESIAN_POINT('',(-0.244810640388203,0.000186482913498504,-1.37073274962121));
#50146=CARTESIAN_POINT('',(-0.24505,-3.00099698131059E-17,-0.775));
#50147=CARTESIAN_POINT('Ctrl Pts',(-0.244854737116733,0.000201854273987251,
-1.35916725037879));
#50148=CARTESIAN_POINT('Ctrl Pts',(-0.245054986723865,0.0260726681896089,
-1.36050913992737));
#50149=CARTESIAN_POINT('Ctrl Pts',(-0.241281085006606,0.0518865600215586,
-1.36185102947594));
#50150=CARTESIAN_POINT('Ctrl Pts',(-0.233287666986612,0.0763200425298408,
-1.36319291902451));
#50151=CARTESIAN_POINT('Ctrl Pts',(-0.20803211976799,0.153518678915402,
-1.36743267663151));
#50152=CARTESIAN_POINT('Ctrl Pts',(-0.140654359094768,0.216937087423053,
-1.3716724342385));
#50153=CARTESIAN_POINT('Ctrl Pts',(-0.0620694940034391,0.237476868429796,
-1.3759121918455));
#50154=CARTESIAN_POINT('Ctrl Pts',(0.0165153710878895,0.25801664943654,
-1.3801519494525));
#50155=CARTESIAN_POINT('Ctrl Pts',(0.106307340597324,0.235677802942377,
-1.38439170705949));
#50156=CARTESIAN_POINT('Ctrl Pts',(0.166107334095492,0.180710241059491,
-1.38863146466649));
#50157=CARTESIAN_POINT('Ctrl Pts',(0.225907327593661,0.125742679176606,
-1.39287122227348));
#50158=CARTESIAN_POINT('Ctrl Pts',(0.255715345080564,0.0381464019049985,
-1.39711097988048));
#50159=CARTESIAN_POINT('Ctrl Pts',(0.241854107162481,-0.0418870385864429,
-1.40135073748747));
#50160=CARTESIAN_POINT('Ctrl Pts',(0.227992869244398,-0.121920479077884,
-1.40559049509447));
#50161=CARTESIAN_POINT('Ctrl Pts',(0.170462375921329,-0.19439108278916,
-1.40983025270146));
#50162=CARTESIAN_POINT('Ctrl Pts',(0.0956602335168951,-0.226046518003429,
-1.41407001030846));
#50163=CARTESIAN_POINT('Ctrl Pts',(0.020858091112461,-0.257701953217699,
-1.41830976791545));
#50164=CARTESIAN_POINT('Ctrl Pts',(-0.0712157003733378,-0.248542219934963,
-1.42254952552245));
#50165=CARTESIAN_POINT('Ctrl Pts',(-0.138316474306822,-0.202771214277427,
-1.42678928312944));
#50166=CARTESIAN_POINT('Ctrl Pts',(-0.203616683984248,-0.158228415567734,
-1.43091527221256));
#50167=CARTESIAN_POINT('Ctrl Pts',(-0.245266132880854,-0.0790128167847663,
-1.43504126129568));
#50168=CARTESIAN_POINT('Ctrl Pts',(-0.245447138551752,4.00299569890614E-5,
-1.43916725037879));
#50169=CARTESIAN_POINT('Ctrl Pts',(-0.245435809527805,6.93114097173611E-5,
-1.45073274962121));
#50170=CARTESIAN_POINT('Ctrl Pts',(-0.245137071181209,-0.0772146114419689,
-1.4466999541055));
#50171=CARTESIAN_POINT('Ctrl Pts',(-0.205588725723683,-0.154757566241512,
-1.44266715858979));
#50172=CARTESIAN_POINT('Ctrl Pts',(-0.142732123706006,-0.199683987839884,
-1.43863436307408));
#50173=CARTESIAN_POINT('Ctrl Pts',(-0.0766497360629118,-0.24691602253762,
-1.43439460546709));
#50174=CARTESIAN_POINT('Ctrl Pts',(0.0151946436936002,-0.258097876093446,
-1.43015484786009));
#50175=CARTESIAN_POINT('Ctrl Pts',(0.0906723427971956,-0.228093108159075,
-1.4259150902531));
#50176=CARTESIAN_POINT('Ctrl Pts',(0.166150041900791,-0.198088340224704,
-1.4216753326461));
#50177=CARTESIAN_POINT('Ctrl Pts',(0.22526106035147,-0.126896950800135,
-1.41743557503911));
#50178=CARTESIAN_POINT('Ctrl Pts',(0.240876966702014,-0.0471868123444759,
-1.41319581743211));
#50179=CARTESIAN_POINT('Ctrl Pts',(0.256492873052558,0.0325233261111841,
-1.40895605982512));
#50180=CARTESIAN_POINT('Ctrl Pts',(0.228613667302968,0.120752213597935,
-1.40471630221812));
#50181=CARTESIAN_POINT('Ctrl Pts',(0.17003458597265,0.177019340192329,-1.40047654461113));
#50182=CARTESIAN_POINT('Ctrl Pts',(0.111455504642331,0.233286466786723,
-1.39623678700413));
#50183=CARTESIAN_POINT('Ctrl Pts',(0.0221765477312852,0.25759183248876,
-1.39199702939714));
#50184=CARTESIAN_POINT('Ctrl Pts',(-0.0568401410365609,0.238782541867253,
-1.38775727179014));
#50185=CARTESIAN_POINT('Ctrl Pts',(-0.135856829804407,0.219973251245746,
-1.38351751418315));
#50186=CARTESIAN_POINT('Ctrl Pts',(-0.204611250429054,0.158049304300695,
-1.37927775657615));
#50187=CARTESIAN_POINT('Ctrl Pts',(-0.231555826218807,0.0814237546635944,
-1.37503799896915));
#50188=CARTESIAN_POINT('Ctrl Pts',(-0.240676089537489,0.0554873585932992,
-1.37360291585317));
#50189=CARTESIAN_POINT('Ctrl Pts',(-0.245006186352852,0.0278665954788627,
-1.37216783273719));
#50190=CARTESIAN_POINT('Ctrl Pts',(-0.244810640388203,0.000186482913498504,
-1.37073274962121));
#50191=CARTESIAN_POINT('Origin',(0.,0.,-0.775));
#50192=CARTESIAN_POINT('',(-0.244719259061378,-0.000134367261369422,-1.27916725037879));
#50193=CARTESIAN_POINT('',(-0.244751695427407,-0.000157197744526027,-1.29073274962121));
#50194=CARTESIAN_POINT('',(-0.24505,-3.00099698131059E-17,-0.775));
#50195=CARTESIAN_POINT('Ctrl Pts',(-0.244719259061378,-0.000134367261369422,
-1.27916725037879));
#50196=CARTESIAN_POINT('Ctrl Pts',(-0.244472862950292,0.0494828240606653,
-1.28173726095206));
#50197=CARTESIAN_POINT('Ctrl Pts',(-0.229836346380894,0.0992336302732099,
-1.28430727152533));
#50198=CARTESIAN_POINT('Ctrl Pts',(-0.201810743245362,0.139715073160739,
-1.2868772820986));
#50199=CARTESIAN_POINT('Ctrl Pts',(-0.155576784007822,0.206497485346041,
-1.29111703970559));
#50200=CARTESIAN_POINT('Ctrl Pts',(-0.0729040986815001,0.248053098858462,
-1.29535679731259));
#50201=CARTESIAN_POINT('Ctrl Pts',(0.00827454241877256,0.245314919832351,
-1.29959655491958));
#50202=CARTESIAN_POINT('Ctrl Pts',(0.0894531835190455,0.24257674080624,
-1.30383631252658));
#50203=CARTESIAN_POINT('Ctrl Pts',(0.16913778039327,0.195544769241596,-1.30807607013357));
#50204=CARTESIAN_POINT('Ctrl Pts',(0.210766596934376,0.125798721930996,
-1.31231582774057));
#50205=CARTESIAN_POINT('Ctrl Pts',(0.252395413475482,0.0560526746203967,
-1.31655558534757));
#50206=CARTESIAN_POINT('Ctrl Pts',(0.255968449683472,-0.0364074484361572,
-1.32079534295456));
#50207=CARTESIAN_POINT('Ctrl Pts',(0.219846277492275,-0.109158108861869,
-1.32503510056156));
#50208=CARTESIAN_POINT('Ctrl Pts',(0.183724105301078,-0.181908769287581,
-1.32927485816855));
#50209=CARTESIAN_POINT('Ctrl Pts',(0.107906724710694,-0.234949967082449,
-1.33351461577555));
#50210=CARTESIAN_POINT('Ctrl Pts',(0.0271814967732379,-0.243944758897442,
-1.33775437338254));
#50211=CARTESIAN_POINT('Ctrl Pts',(-0.0535437311642181,-0.252939550712434,
-1.34199413098954));
#50212=CARTESIAN_POINT('Ctrl Pts',(-0.139176806448746,-0.21788793654755,
-1.34623388859653));
#50213=CARTESIAN_POINT('Ctrl Pts',(-0.190426677209,-0.154872697333372,-1.35047364620353));
#50214=CARTESIAN_POINT('Ctrl Pts',(-0.225455888131193,-0.111801874461019,
-1.35337151426195));
#50215=CARTESIAN_POINT('Ctrl Pts',(-0.244422289497751,-0.0556672784509742,
-1.35626938232037));
#50216=CARTESIAN_POINT('Ctrl Pts',(-0.244854737116733,0.000201854273987251,
-1.35916725037879));
#50217=CARTESIAN_POINT('Ctrl Pts',(-0.244810640388203,0.000186482913498504,
-1.37073274962121));
#50218=CARTESIAN_POINT('Ctrl Pts',(-0.244428472433774,-0.0539105270476947,
-1.36792807513019));
#50219=CARTESIAN_POINT('Ctrl Pts',(-0.226760440538336,-0.108234224483701,
-1.36512340063918));
#50220=CARTESIAN_POINT('Ctrl Pts',(-0.193781152536664,-0.150654232462379,
-1.36231872614817));
#50221=CARTESIAN_POINT('Ctrl Pts',(-0.143927172109908,-0.214779517622103,
-1.35807896854117));
#50222=CARTESIAN_POINT('Ctrl Pts',(-0.0590844803015342,-0.251702935612399,
-1.35383921093418));
#50223=CARTESIAN_POINT('Ctrl Pts',(0.0218187473288031,-0.244482765576226,
-1.34959945332718));
#50224=CARTESIAN_POINT('Ctrl Pts',(0.10272197495914,-0.237262595540053,
-1.34535969572019));
#50225=CARTESIAN_POINT('Ctrl Pts',(0.179685738411441,-0.185898837477412,
-1.34111993811319));
#50226=CARTESIAN_POINT('Ctrl Pts',(0.217396563364921,-0.11395882571878,
-1.3368801805062));
#50227=CARTESIAN_POINT('Ctrl Pts',(0.2551073883184,-0.0420188139601475,
-1.3326404228992));
#50228=CARTESIAN_POINT('Ctrl Pts',(0.253565274773058,0.0504974514944755,
-1.32840066529221));
#50229=CARTESIAN_POINT('Ctrl Pts',(0.213477862795548,0.121140699626764,
-1.32416090768521));
#50230=CARTESIAN_POINT('Ctrl Pts',(0.173390450818038,0.191783947759052,
-1.31992115007821));
#50231=CARTESIAN_POINT('Ctrl Pts',(0.0947577404083598,0.240554178569004,
-1.31568139247122));
#50232=CARTESIAN_POINT('Ctrl Pts',(0.0136587974671215,0.245074094240732,
-1.31144163486423));
#50233=CARTESIAN_POINT('Ctrl Pts',(-0.0674401454741175,0.24959400991246,
-1.30720187725723));
#50234=CARTESIAN_POINT('Ctrl Pts',(-0.151005320946917,0.209863610445962,
-1.30296211965023));
#50235=CARTESIAN_POINT('Ctrl Pts',(-0.198694439746781,0.144112432926045,
-1.29872236204324));
#50236=CARTESIAN_POINT('Ctrl Pts',(-0.22865036421838,0.102810824566048,
-1.29605915790256));
#50237=CARTESIAN_POINT('Ctrl Pts',(-0.244450581848228,0.0512421316912588,
-1.29339595376188));
#50238=CARTESIAN_POINT('Ctrl Pts',(-0.244751695427407,-0.000157197744526027,
-1.29073274962121));
#50239=CARTESIAN_POINT('Origin',(0.,0.,-0.775));
#50240=CARTESIAN_POINT('',(-0.245346864912507,-0.000144723283361653,-1.1991672503788));
#50241=CARTESIAN_POINT('',(-0.245384515459765,-0.000118217032388335,-1.21073274962121));
#50242=CARTESIAN_POINT('',(-0.24505,-3.00099698131059E-17,-0.775));
#50243=CARTESIAN_POINT('Ctrl Pts',(-0.245346864912507,-0.000144723283361653,
-1.1991672503788));
#50244=CARTESIAN_POINT('Ctrl Pts',(-0.24483734676681,0.0727041776369625,
-1.20296538197676));
#50245=CARTESIAN_POINT('Ctrl Pts',(-0.210320245808661,0.145972253025746,
-1.20676351357472));
#50246=CARTESIAN_POINT('Ctrl Pts',(-0.153552896413428,0.191492521208896,
-1.21056164517268));
#50247=CARTESIAN_POINT('Ctrl Pts',(-0.0901849495111878,0.242305637691093,
-1.21480140277968));
#50248=CARTESIAN_POINT('Ctrl Pts',(0.000908338903704564,0.258543075920582,
-1.21904116038667));
#50249=CARTESIAN_POINT('Ctrl Pts',(0.0779305696397273,0.23275460038141,
-1.22328091799367));
#50250=CARTESIAN_POINT('Ctrl Pts',(0.15495280037575,0.206966124842239,-1.22752067560066));
#50251=CARTESIAN_POINT('Ctrl Pts',(0.217903973432903,0.139151735534406,
-1.23176043320766));
#50252=CARTESIAN_POINT('Ctrl Pts',(0.237900156835131,0.0604267576219127,
-1.23600019081465));
#50253=CARTESIAN_POINT('Ctrl Pts',(0.25789634023736,-0.0182982202905806,
-1.24023994842165));
#50254=CARTESIAN_POINT('Ctrl Pts',(0.234937533984665,-0.107933786807734,
-1.24447970602864));
#50255=CARTESIAN_POINT('Ctrl Pts',(0.179557943493476,-0.167352390514998,
-1.24871946363564));
#50256=CARTESIAN_POINT('Ctrl Pts',(0.124178353002287,-0.226770994222261,
-1.25295922124264));
#50257=CARTESIAN_POINT('Ctrl Pts',(0.0363779782726041,-0.255972635119634,
-1.25719897884963));
#50258=CARTESIAN_POINT('Ctrl Pts',(-0.0435576711461274,-0.241558703022307,
-1.26143873645663));
#50259=CARTESIAN_POINT('Ctrl Pts',(-0.123493320564858,-0.22714477092498,
-1.26567849406362));
#50260=CARTESIAN_POINT('Ctrl Pts',(-0.195564244672638,-0.169115265832955,
-1.26991825167062));
#50261=CARTESIAN_POINT('Ctrl Pts',(-0.226702090152149,-0.0940959078578519,
-1.27415800927761));
#50262=CARTESIAN_POINT('Ctrl Pts',(-0.238965132039332,-0.0645509757974888,
-1.27582775631134));
#50263=CARTESIAN_POINT('Ctrl Pts',(-0.244879343685111,-0.0323708720032655,
-1.27749750334507));
#50264=CARTESIAN_POINT('Ctrl Pts',(-0.244719259061378,-0.000134367261369422,
-1.27916725037879));
#50265=CARTESIAN_POINT('Ctrl Pts',(-0.244751695427407,-0.000157197744526027,
-1.29073274962121));
#50266=CARTESIAN_POINT('Ctrl Pts',(-0.244929947499698,-0.0305843774528814,
-1.28915619615489));
#50267=CARTESIAN_POINT('Ctrl Pts',(-0.2396767583184,-0.0609522061454329,
-1.28757964268857));
#50268=CARTESIAN_POINT('Ctrl Pts',(-0.228713440581758,-0.0890956461841305,
-1.28600308922225));
#50269=CARTESIAN_POINT('Ctrl Pts',(-0.199230260489943,-0.164780592201052,
-1.28176333161526));
#50270=CARTESIAN_POINT('Ctrl Pts',(-0.128450838179383,-0.224378528661559,
-1.27752357400826));
#50271=CARTESIAN_POINT('Ctrl Pts',(-0.0488509415881311,-0.240544088895643,
-1.27328381640127));
#50272=CARTESIAN_POINT('Ctrl Pts',(0.0307489550031208,-0.256709649129727,
-1.26904405879427));
#50273=CARTESIAN_POINT('Ctrl Pts',(0.119169325875064,-0.229442833137387,
-1.26480430118728));
#50274=CARTESIAN_POINT('Ctrl Pts',(0.175840185746171,-0.171254495081629,
-1.26056454358028));
#50275=CARTESIAN_POINT('Ctrl Pts',(0.232511045617277,-0.113066157025871,
-1.25632478597329));
#50276=CARTESIAN_POINT('Ctrl Pts',(0.257432394487546,-0.0239562969066957,
-1.25208502836629));
#50277=CARTESIAN_POINT('Ctrl Pts',(0.239169553386271,0.0551887446749379,
-1.2478452707593));
#50278=CARTESIAN_POINT('Ctrl Pts',(0.220906712284997,0.134333786256571,
-1.2436055131523));
#50279=CARTESIAN_POINT('Ctrl Pts',(0.159459681212178,0.203514009300662,
-1.2393657555453));
#50280=CARTESIAN_POINT('Ctrl Pts',(0.0830222449175702,0.230987401867944,
-1.23512599793831));
#50281=CARTESIAN_POINT('Ctrl Pts',(0.00658480862296257,0.258460794435227,
-1.23088624033131));
#50282=CARTESIAN_POINT('Ctrl Pts',(-0.0848430328934345,0.2442273565257,
-1.22664648272432));
#50283=CARTESIAN_POINT('Ctrl Pts',(-0.149311376844718,0.19481782690153,
-1.22240672511732));
#50284=CARTESIAN_POINT('Ctrl Pts',(-0.20848157298366,0.149468879188461,
-1.21851539995195));
#50285=CARTESIAN_POINT('Ctrl Pts',(-0.244941369133683,0.0744879581436564,
-1.21462407478658));
#50286=CARTESIAN_POINT('Ctrl Pts',(-0.245384515459765,-0.000118217032388335,
-1.21073274962121));
#50287=CARTESIAN_POINT('Origin',(0.,0.,-0.775));
#50288=CARTESIAN_POINT('',(-0.245167484065513,0.000212043117031907,-1.1191672503788));
#50289=CARTESIAN_POINT('',(-0.245113203773488,0.00022073262402164,-1.13073274962121));
#50290=CARTESIAN_POINT('',(-0.24505,-3.00099698131059E-17,-0.775));
#50291=CARTESIAN_POINT('Ctrl Pts',(-0.245167484065513,0.000212043117031907,
-1.1191672503788));
#50292=CARTESIAN_POINT('Ctrl Pts',(-0.245305444362438,0.0153259129849596,
-1.11995374539446));
#50293=CARTESIAN_POINT('Ctrl Pts',(-0.244028163778416,0.030416526229839,
-1.12074024041012));
#50294=CARTESIAN_POINT('Ctrl Pts',(-0.241251890522508,0.0452261317696372,
-1.12152673542578));
#50295=CARTESIAN_POINT('Ctrl Pts',(-0.226285838072791,0.125060252131,-1.12576649303278));
#50296=CARTESIAN_POINT('Ctrl Pts',(-0.167759610554573,0.196728392058633,
-1.13000625063977));
#50297=CARTESIAN_POINT('Ctrl Pts',(-0.0925268390960716,0.227347007287172,
-1.13424600824677));
#50298=CARTESIAN_POINT('Ctrl Pts',(-0.0172940676375692,0.257965622515711,
-1.13848576585376));
#50299=CARTESIAN_POINT('Ctrl Pts',(0.0746452477612181,0.247534713045156,
-1.14272552346076));
#50300=CARTESIAN_POINT('Ctrl Pts',(0.141106524790587,0.200840300580519,
-1.14696528106775));
#50301=CARTESIAN_POINT('Ctrl Pts',(0.207567801819956,0.154145888115883,
-1.15120503867475));
#50302=CARTESIAN_POINT('Ctrl Pts',(0.248551040479906,0.0711879726571643,
-1.15544479628174));
#50303=CARTESIAN_POINT('Ctrl Pts',(0.245251871857863,-0.00996980568939554,
-1.15968455388874));
#50304=CARTESIAN_POINT('Ctrl Pts',(0.241952703235821,-0.091127584035954,
-1.16392431149573));
#50305=CARTESIAN_POINT('Ctrl Pts',(0.194371127331788,-0.170485225270353,
-1.16816406910273));
#50306=CARTESIAN_POINT('Ctrl Pts',(0.124339032886921,-0.211631005706291,
-1.17240382670972));
#50307=CARTESIAN_POINT('Ctrl Pts',(0.0543069384420516,-0.25277678614223,
-1.17664358431672));
#50308=CARTESIAN_POINT('Ctrl Pts',(-0.0381756745436533,-0.255710705779704,
-1.18088334192371));
#50309=CARTESIAN_POINT('Ctrl Pts',(-0.110674942130753,-0.219086592152763,
-1.18512309953071));
#50310=CARTESIAN_POINT('Ctrl Pts',(-0.183174209717853,-0.182462478525821,
-1.18936285713771));
#50311=CARTESIAN_POINT('Ctrl Pts',(-0.235690131906348,-0.106280331634464,
-1.1936026147447));
#50312=CARTESIAN_POINT('Ctrl Pts',(-0.244126790305802,-0.0254948608213339,
-1.1978423723517));
#50313=CARTESIAN_POINT('Ctrl Pts',(-0.245005578228106,-0.0170800012066754,
-1.19828399836073));
#50314=CARTESIAN_POINT('Ctrl Pts',(-0.245406108901139,-0.00861519581599708,
-1.19872562436976));
#50315=CARTESIAN_POINT('Ctrl Pts',(-0.245346864912507,-0.000144723283361653,
-1.1991672503788));
#50316=CARTESIAN_POINT('Ctrl Pts',(-0.245384515459765,-0.000118217032388335,
-1.21073274962121));
#50317=CARTESIAN_POINT('Ctrl Pts',(-0.245424195144662,-0.0067985150470858,
-1.21038431717958));
#50318=CARTESIAN_POINT('Ctrl Pts',(-0.245175109242132,-0.0134758085149568,
-1.21003588473796));
#50319=CARTESIAN_POINT('Ctrl Pts',(-0.244627705212326,-0.020128555650413,
-1.20968745229634));
#50320=CARTESIAN_POINT('Ctrl Pts',(-0.237966843242477,-0.101079787239374,
-1.20544769468934));
#50321=CARTESIAN_POINT('Ctrl Pts',(-0.18713627291661,-0.178396629078483,
-1.20120793708235));
#50322=CARTESIAN_POINT('Ctrl Pts',(-0.115458621318355,-0.216603738881799,
-1.19696817947535));
#50323=CARTESIAN_POINT('Ctrl Pts',(-0.0437809697200995,-0.254810848685115,
-1.19272842186835));
#50324=CARTESIAN_POINT('Ctrl Pts',(0.0487437631505439,-0.253908226452637,
-1.18848866426136));
#50325=CARTESIAN_POINT('Ctrl Pts',(0.119662387405715,-0.214310023021451,
-1.18424890665437));
#50326=CARTESIAN_POINT('Ctrl Pts',(0.190581011660885,-0.174711819590264,
-1.18000914904737));
#50327=CARTESIAN_POINT('Ctrl Pts',(0.239893527300583,-0.096418034960368,
-1.17576939144037));
#50328=CARTESIAN_POINT('Ctrl Pts',(0.244973837284843,-0.015352262714056,
-1.17152963383338));
#50329=CARTESIAN_POINT('Ctrl Pts',(0.250054147269103,0.0657135095322565,
-1.16728987622638));
#50330=CARTESIAN_POINT('Ctrl Pts',(0.210902251597925,0.149551269394986,
-1.16305011861939));
#50331=CARTESIAN_POINT('Ctrl Pts',(0.145482242747102,0.197693677120017,
-1.15881036101239));
#50332=CARTESIAN_POINT('Ctrl Pts',(0.0800622338962787,0.245836084845048,
-1.1545706034054));
#50333=CARTESIAN_POINT('Ctrl Pts',(-0.0116258881341887,0.258283140432381,
-1.1503308457984));
#50334=CARTESIAN_POINT('Ctrl Pts',(-0.0875127962613097,0.229323752405274,
-1.14609108819141));
#50335=CARTESIAN_POINT('Ctrl Pts',(-0.163399704388431,0.200364364378166,
-1.14185133058441));
#50336=CARTESIAN_POINT('Ctrl Pts',(-0.223485398612205,0.129998532736619,
-1.13761157297742));
#50337=CARTESIAN_POINT('Ctrl Pts',(-0.240200716576505,0.050512262695319,
-1.13337181537042));
#50338=CARTESIAN_POINT('Ctrl Pts',(-0.243668904085937,0.0340200075364671,
-1.13249212678735));
#50339=CARTESIAN_POINT('Ctrl Pts',(-0.245269985293028,0.0171351150642011,
-1.13161243820428));
#50340=CARTESIAN_POINT('Ctrl Pts',(-0.245113203773488,0.00022073262402164,
-1.13073274962121));
#50341=CARTESIAN_POINT('Origin',(0.,0.,-0.775));
#50342=CARTESIAN_POINT('',(-0.244649653071174,3.34626584120729E-5,-1.03916725037879));
#50343=CARTESIAN_POINT('',(-0.244645538675098,3.85059038551794E-6,-1.05073274962121));
#50344=CARTESIAN_POINT('',(-0.24505,-3.00099698131059E-17,-0.775));
#50345=CARTESIAN_POINT('Ctrl Pts',(-0.244649653071174,3.34626584120729E-5,
-1.03916725037879));
#50346=CARTESIAN_POINT('Ctrl Pts',(-0.244696975754832,0.0389557362310942,
-1.04118186641915));
#50347=CARTESIAN_POINT('Ctrl Pts',(-0.235956892958235,0.0778579314244324,
-1.04319648245951));
#50348=CARTESIAN_POINT('Ctrl Pts',(-0.218316444296445,0.112186486821377,
-1.04521109849987));
#50349=CARTESIAN_POINT('Ctrl Pts',(-0.18119213628617,0.184430900131816,
-1.04945085610686));
#50350=CARTESIAN_POINT('Ctrl Pts',(-0.104648852062527,0.236419045208656,
-1.05369061371385));
#50351=CARTESIAN_POINT('Ctrl Pts',(-0.0238070018601966,0.244297163999081,
-1.05793037132085));
#50352=CARTESIAN_POINT('Ctrl Pts',(0.0570348483421337,0.252175282789506,
-1.06217012892784));
#50353=CARTESIAN_POINT('Ctrl Pts',(0.142175264523152,0.215943375293518,
-1.06640988653484));
#50354=CARTESIAN_POINT('Ctrl Pts',(0.192549208199601,0.152225753725436,
-1.07064964414184));
#50355=CARTESIAN_POINT('Ctrl Pts',(0.242923151876051,0.0885081321573535,
-1.07488940174883));
#50356=CARTESIAN_POINT('Ctrl Pts',(0.258530623047931,-0.00269520348282262,
-1.07912915935583));
#50357=CARTESIAN_POINT('Ctrl Pts',(0.232210434475385,-0.0795373610092435,
-1.08336891696282));
#50358=CARTESIAN_POINT('Ctrl Pts',(0.205890245902839,-0.156379518535664,
-1.08760867456982));
#50359=CARTESIAN_POINT('Ctrl Pts',(0.137642397585865,-0.21886049794833,
-1.09184843217681));
#50360=CARTESIAN_POINT('Ctrl Pts',(0.0587810989267877,-0.238312106458149,
-1.09608818978381));
#50361=CARTESIAN_POINT('Ctrl Pts',(-0.0200801997322901,-0.257763714967968,
-1.1003279473908));
#50362=CARTESIAN_POINT('Ctrl Pts',(-0.109554948733473,-0.234185952574941,
-1.1045677049978));
#50363=CARTESIAN_POINT('Ctrl Pts',(-0.168589384543456,-0.17839702098088,
-1.10880746260479));
#50364=CARTESIAN_POINT('Ctrl Pts',(-0.216672654314996,-0.132957199098996,
-1.11226072519613));
#50365=CARTESIAN_POINT('Ctrl Pts',(-0.244561741978186,-0.0661484046745886,
-1.11571398778746));
#50366=CARTESIAN_POINT('Ctrl Pts',(-0.245167484065513,0.000212043117031907,
-1.1191672503788));
#50367=CARTESIAN_POINT('Ctrl Pts',(-0.245113203773488,0.00022073262402164,
-1.13073274962121));
#50368=CARTESIAN_POINT('Ctrl Pts',(-0.244514359207961,-0.0643856446664852,
-1.12737268059728));
#50369=CARTESIAN_POINT('Ctrl Pts',(-0.218269289868647,-0.129422263940181,
-1.12401261157336));
#50370=CARTESIAN_POINT('Ctrl Pts',(-0.172465701285927,-0.174652382769037,
-1.12065254254943));
#50371=CARTESIAN_POINT('Ctrl Pts',(-0.114670426326225,-0.231724049751042,
-1.11641278494244));
#50372=CARTESIAN_POINT('Ctrl Pts',(-0.025734934701994,-0.257260675273999,
-1.11217302733544));
#50373=CARTESIAN_POINT('Ctrl Pts',(0.0535344379030858,-0.239545271055687,
-1.10793326972845));
#50374=CARTESIAN_POINT('Ctrl Pts',(0.132803810508166,-0.221829866837375,
-1.10369351212145));
#50375=CARTESIAN_POINT('Ctrl Pts',(0.202407064094095,-0.160862432877793,
-1.09945375451446));
#50376=CARTESIAN_POINT('Ctrl Pts',(0.230408087683255,-0.0846167008153363,
-1.09521399690746));
#50377=CARTESIAN_POINT('Ctrl Pts',(0.258409111272416,-0.00837096875287918,
-1.09097423930047));
#50378=CARTESIAN_POINT('Ctrl Pts',(0.244807904864808,0.0831530614124536,
-1.08673448169347));
#50379=CARTESIAN_POINT('Ctrl Pts',(0.195845119793085,0.147961352994708,
-1.08249472408648));
#50380=CARTESIAN_POINT('Ctrl Pts',(0.146882334721362,0.212769644576962,
-1.07825496647948));
#50381=CARTESIAN_POINT('Ctrl Pts',(0.0625579709855245,0.250862197576139,
-1.07401520887249));
#50382=CARTESIAN_POINT('Ctrl Pts',(-0.0184373628622437,0.24476097846153,
-1.06977545126549));
#50383=CARTESIAN_POINT('Ctrl Pts',(-0.0994326967100126,0.23865975934692,
-1.0655356936585));
#50384=CARTESIAN_POINT('Ctrl Pts',(-0.177099000669712,0.188364768118525,
-1.0612959360515));
#50385=CARTESIAN_POINT('Ctrl Pts',(-0.215800588552335,0.116952891829257,
-1.0570561784445));
#50386=CARTESIAN_POINT('Ctrl Pts',(-0.235041211799334,0.0814502398137821,
-1.05494836883674));
#50387=CARTESIAN_POINT('Ctrl Pts',(-0.244651260008812,0.040728308239459,
-1.05284055922897));
#50388=CARTESIAN_POINT('Ctrl Pts',(-0.244645568296149,3.85030838442385E-6,
-1.05073274962121));
#50389=CARTESIAN_POINT('Origin',(0.,0.,-0.775));
#50390=CARTESIAN_POINT('',(-0.245044321574299,-0.000225594368389231,-0.959167250378794));
#50391=CARTESIAN_POINT('',(-0.245099029133644,-0.000222287294248484,-0.970732749621207));
#50392=CARTESIAN_POINT('',(-0.24505,-3.00099698131059E-17,-0.775));
#50393=CARTESIAN_POINT('Ctrl Pts',(-0.245044321574299,-0.000225594368389231,
-0.959167250378794));
#50394=CARTESIAN_POINT('Ctrl Pts',(-0.244469510773935,0.0621696777858805,
-0.962409987443846));
#50395=CARTESIAN_POINT('Ctrl Pts',(-0.220208236993727,0.124962399432046,
-0.965652724508897));
#50396=CARTESIAN_POINT('Ctrl Pts',(-0.177227576931743,0.169818325425937,
-0.968895461573948));
#50397=CARTESIAN_POINT('Ctrl Pts',(-0.121031969086925,0.228465773441711,
-0.973135219180944));
#50398=CARTESIAN_POINT('Ctrl Pts',(-0.0328363455678891,0.256451012057126,
-0.977374976787939));
#50399=CARTESIAN_POINT('Ctrl Pts',(0.0468924321585544,0.240933554080418,
-0.981614734394934));
#50400=CARTESIAN_POINT('Ctrl Pts',(0.126621209884998,0.22541609610371,-0.98585449200193));
#50401=CARTESIAN_POINT('Ctrl Pts',(0.197883141818849,0.166395941534881,
-0.990094249608925));
#50402=CARTESIAN_POINT('Ctrl Pts',(0.227981064400714,0.0909533504071397,
-0.994334007215921));
#50403=CARTESIAN_POINT('Ctrl Pts',(0.258078986982579,0.0155107592793984,
-0.998573764822916));
#50404=CARTESIAN_POINT('Ctrl Pts',(0.24701290021246,-0.0763542684072548,
-1.00281352242991));
#50405=CARTESIAN_POINT('Ctrl Pts',(0.199860264654025,-0.142491235828697,
-1.00705328003691));
#50406=CARTESIAN_POINT('Ctrl Pts',(0.15270762909559,-0.208628203250139,
-1.0112930376439));
#50407=CARTESIAN_POINT('Ctrl Pts',(0.0694684447488411,-0.249037110406371,
-1.0155327952509));
#50408=CARTESIAN_POINT('Ctrl Pts',(-0.0116645934749716,-0.245177109320242,
-1.01977255285789));
#50409=CARTESIAN_POINT('Ctrl Pts',(-0.0927976316987844,-0.241317108234113,
-1.02401231046489));
#50410=CARTESIAN_POINT('Ctrl Pts',(-0.17182452379966,-0.193188198905624,
-1.02825206807188));
#50411=CARTESIAN_POINT('Ctrl Pts',(-0.212485303951644,-0.122873403469361,
-1.03249182567888));
#50412=CARTESIAN_POINT('Ctrl Pts',(-0.233825201284185,-0.0859702621631733,
-1.03471696724552));
#50413=CARTESIAN_POINT('Ctrl Pts',(-0.244597385210529,-0.0429561527619699,
-1.03694210881216));
#50414=CARTESIAN_POINT('Ctrl Pts',(-0.244649653071174,3.34626584120729E-5,
-1.03916725037879));
#50415=CARTESIAN_POINT('Ctrl Pts',(-0.244645568296149,3.85030838442385E-6,
-1.05073274962121));
#50416=CARTESIAN_POINT('Ctrl Pts',(-0.244639811402652,-0.0411869793974703,
-1.04860080162198));
#50417=CARTESIAN_POINT('Ctrl Pts',(-0.234796816845105,-0.082380393654487,
-1.04646885362275));
#50418=CARTESIAN_POINT('Ctrl Pts',(-0.215131935267918,-0.118178354002115,
-1.04433690562352));
#50419=CARTESIAN_POINT('Ctrl Pts',(-0.176024822295332,-0.189368962194075,
-1.04009714801652));
#50420=CARTESIAN_POINT('Ctrl Pts',(-0.0980737245446141,-0.239221417227855,
-1.03585739040953));
#50421=CARTESIAN_POINT('Ctrl Pts',(-0.0170450003451614,-0.244861881251446,
-1.03161763280253));
#50422=CARTESIAN_POINT('Ctrl Pts',(0.0639837238542925,-0.250502345275036,
-1.02737787519554));
#50423=CARTESIAN_POINT('Ctrl Pts',(0.148090074502482,-0.211930818288436,
-1.02313811758854));
#50424=CARTESIAN_POINT('Ctrl Pts',(0.196683474149454,-0.146845101802087,
-1.01889835998155));
#50425=CARTESIAN_POINT('Ctrl Pts',(0.245276873796425,-0.0817593853157384,
-1.01465860237455));
#50426=CARTESIAN_POINT('Ctrl Pts',(0.258357322442181,0.00984052067035691,
-1.01041884476756));
#50427=CARTESIAN_POINT('Ctrl Pts',(0.229923108412695,0.0859257653129111,
-1.00617908716056));
#50428=CARTESIAN_POINT('Ctrl Pts',(0.201488894383209,0.162011009955465,
-1.00193932955357));
#50429=CARTESIAN_POINT('Ctrl Pts',(0.131540017678481,0.222581593254477,
-0.99769957194657));
#50430=CARTESIAN_POINT('Ctrl Pts',(0.0521711717813305,0.23984587084569,
-0.993459814339575));
#50431=CARTESIAN_POINT('Ctrl Pts',(-0.0271976741158197,0.257110148436903,
-0.98922005673258));
#50432=CARTESIAN_POINT('Ctrl Pts',(-0.115986489205392,0.231068120320316,
-0.984980299125584));
#50433=CARTESIAN_POINT('Ctrl Pts',(-0.173456237504991,0.173668669014814,
-0.980740541518589));
#50434=CARTESIAN_POINT('Ctrl Pts',(-0.218674646565952,0.128505571110223,
-0.977404610886129));
#50435=CARTESIAN_POINT('Ctrl Pts',(-0.244503815935465,0.0639294875508147,
-0.974068680253668));
#50436=CARTESIAN_POINT('Ctrl Pts',(-0.245099029133644,-0.000222287294248484,
-0.970732749621207));
#50437=CARTESIAN_POINT('Origin',(0.,0.,-0.775));
#50438=CARTESIAN_POINT('',(-0.245422031604165,8.10237884523012E-5,-0.879167250378794));
#50439=CARTESIAN_POINT('',(-0.24539320090154,0.000110883525149794,-0.890732749621207));
#50440=CARTESIAN_POINT('',(-0.24505,-3.00099698131059E-17,-0.775));
#50441=CARTESIAN_POINT('Ctrl Pts',(-0.245422031604165,8.10237884523012E-5,
-0.879167250378794));
#50442=CARTESIAN_POINT('Ctrl Pts',(-0.245441074602344,0.00450998645013945,
-0.879398350861545));
#50443=CARTESIAN_POINT('Ctrl Pts',(-0.245331595776088,0.00893798850812526,
-0.879629451344296));
#50444=CARTESIAN_POINT('Ctrl Pts',(-0.245090635265792,0.013358824071627,
-0.879860551827046));
#50445=CARTESIAN_POINT('Ctrl Pts',(-0.240669986099019,0.0944632466437396,
-0.884100309434042));
#50446=CARTESIAN_POINT('Ctrl Pts',(-0.191996042349709,0.173155614686405,
-0.888340067041037));
#50447=CARTESIAN_POINT('Ctrl Pts',(-0.121401904688346,0.213329452288258,
-0.892579824648033));
#50448=CARTESIAN_POINT('Ctrl Pts',(-0.0508077670269831,0.253503289890111,
-0.896819582255028));
#50449=CARTESIAN_POINT('Ctrl Pts',(0.0417065645464325,0.255158597051152,
-0.901059339862023));
#50450=CARTESIAN_POINT('Ctrl Pts',(0.11369267263772,0.217535867994358,-0.905299097469018));
#50451=CARTESIAN_POINT('Ctrl Pts',(0.185678780729008,0.179913138937563,
-0.909538855076014));
#50452=CARTESIAN_POINT('Ctrl Pts',(0.237136665338167,0.103012373662934,
-0.913778612683009));
#50453=CARTESIAN_POINT('Ctrl Pts',(0.24445586820471,0.0221180056932788,
-0.918018370290005));
#50454=CARTESIAN_POINT('Ctrl Pts',(0.251775071071252,-0.058776362276376,
-0.922258127897));
#50455=CARTESIAN_POINT('Ctrl Pts',(0.214955592195177,-0.143664332941056,
-0.926497885503995));
#50456=CARTESIAN_POINT('Ctrl Pts',(0.150891339590376,-0.193596697575626,
-0.93073764311099));
#50457=CARTESIAN_POINT('Ctrl Pts',(0.0868270869855739,-0.243529062210196,
-0.934977400717986));
#50458=CARTESIAN_POINT('Ctrl Pts',(-0.0044819393479547,-0.258505820814656,
-0.939217158324981));
#50459=CARTESIAN_POINT('Ctrl Pts',(-0.0811403530874316,-0.231655176450718,
-0.943456915931977));
#50460=CARTESIAN_POINT('Ctrl Pts',(-0.157798766826908,-0.20480453208678,
-0.947696673538972));
#50461=CARTESIAN_POINT('Ctrl Pts',(-0.219806567972333,-0.136126484754444,
-0.951936431145967));
#50462=CARTESIAN_POINT('Ctrl Pts',(-0.238712672459747,-0.0571326323802092,
-0.956176188752962));
#50463=CARTESIAN_POINT('Ctrl Pts',(-0.243158628169807,-0.0385564540216952,
-0.957173209294906));
#50464=CARTESIAN_POINT('Ctrl Pts',(-0.245221054428119,-0.0194098102977235,
-0.95817022983685));
#50465=CARTESIAN_POINT('Ctrl Pts',(-0.245044321574299,-0.000225594368389231,
-0.959167250378794));
#50466=CARTESIAN_POINT('Ctrl Pts',(-0.245099029133644,-0.000222287294248484,
-0.970732749621207));
#50467=CARTESIAN_POINT('Ctrl Pts',(-0.245260294400637,-0.017603375499452,
-0.969828922646673));
#50468=CARTESIAN_POINT('Ctrl Pts',(-0.243569214490148,-0.0349533165394845,
-0.968925095672138));
#50469=CARTESIAN_POINT('Ctrl Pts',(-0.239909546000387,-0.0518775738123231,
-0.968021268697603));
#50470=CARTESIAN_POINT('Ctrl Pts',(-0.22274242468656,-0.131267490839541,
-0.963781511090608));
#50471=CARTESIAN_POINT('Ctrl Pts',(-0.162257500549283,-0.201290450399556,
-0.959541753483612));
#50472=CARTESIAN_POINT('Ctrl Pts',(-0.0862071148979349,-0.2298177675197,
-0.955301995876616));
#50473=CARTESIAN_POINT('Ctrl Pts',(-0.0101567292465875,-0.258345084639844,
-0.951062238269621));
#50474=CARTESIAN_POINT('Ctrl Pts',(0.0814591179188316,-0.245376759320117,
-0.946822480662627));
#50475=CARTESIAN_POINT('Ctrl Pts',(0.146604261452242,-0.196863057608093,
-0.942582723055632));
#50476=CARTESIAN_POINT('Ctrl Pts',(0.211749404985652,-0.14834935589607,
-0.938342965448636));
#50477=CARTESIAN_POINT('Ctrl Pts',(0.250423844887055,-0.0642902777917504,
-0.93410320784164));
#50478=CARTESIAN_POINT('Ctrl Pts',(0.244882560039177,0.016745289350255,
-0.929863450234645));
#50479=CARTESIAN_POINT('Ctrl Pts',(0.239341275191298,0.0977808564922616,
-0.925623692627649));
#50480=CARTESIAN_POINT('Ctrl Pts',(0.189584265594134,0.175792912671955,
-0.921383935020655));
#50481=CARTESIAN_POINT('Ctrl Pts',(0.118441575801277,0.214987129960086,
-0.91714417741366));
#50482=CARTESIAN_POINT('Ctrl Pts',(0.0472988860084194,0.254181347248218,
-0.912904419806664));
#50483=CARTESIAN_POINT('Ctrl Pts',(-0.0452294839801312,0.254557725644789,
-0.908664662199669));
#50484=CARTESIAN_POINT('Ctrl Pts',(-0.116688675514067,0.215943571178994,
-0.904424904592673));
#50485=CARTESIAN_POINT('Ctrl Pts',(-0.188147867048003,0.1773294167132,-0.900185146985678));
#50486=CARTESIAN_POINT('Ctrl Pts',(-0.238537880127323,0.0997247293850409,
-0.895945389378683));
#50487=CARTESIAN_POINT('Ctrl Pts',(-0.244738228754766,0.0187369237801842,
-0.891705631771688));
#50488=CARTESIAN_POINT('Ctrl Pts',(-0.245212486095677,0.0125422622151333,
-0.891381337721528));
#50489=CARTESIAN_POINT('Ctrl Pts',(-0.245428210065485,0.00632780758345109,
-0.891057043671367));
#50490=CARTESIAN_POINT('Ctrl Pts',(-0.24539320090154,0.000110883525149794,
-0.890732749621207));
#50491=CARTESIAN_POINT('Origin',(0.,0.,-0.775));
#50492=CARTESIAN_POINT('',(-0.244799711053798,0.000182046184206572,-0.799167250378795));
#50493=CARTESIAN_POINT('',(-0.244760945085023,0.000162685199137168,-0.810732749621207));
#50494=CARTESIAN_POINT('',(-0.24505,-3.00099698131059E-17,-0.775));
#50495=CARTESIAN_POINT('Ctrl Pts',(-0.244799711053798,0.000182046184206572,
-0.799167250378795));
#50496=CARTESIAN_POINT('Ctrl Pts',(-0.244993156130942,0.0283308761463506,
-0.80062647188624));
#50497=CARTESIAN_POINT('Ctrl Pts',(-0.240512320471579,0.0564200071496143,
-0.802085693393685));
#50498=CARTESIAN_POINT('Ctrl Pts',(-0.231088852819787,0.0827394692876446,
-0.803544914901131));
#50499=CARTESIAN_POINT('Ctrl Pts',(-0.203709035254664,0.159210477453564,
-0.807784672508126));
#50500=CARTESIAN_POINT('Ctrl Pts',(-0.134604069490859,0.22074213836936,
-0.812024430115121));
#50501=CARTESIAN_POINT('Ctrl Pts',(-0.0554814367462919,0.239101835735599,
-0.816264187722116));
#50502=CARTESIAN_POINT('Ctrl Pts',(0.023641195998275,0.257461533101838,
-0.820503945329112));
#50503=CARTESIAN_POINT('Ctrl Pts',(0.112781495723604,0.23264926691852,-0.824743702936108));
#50504=CARTESIAN_POINT('Ctrl Pts',(0.171039154498696,0.176049667150885,
-0.828983460543103));
#50505=CARTESIAN_POINT('Ctrl Pts',(0.229296813273789,0.119450067383251,
-0.833223218150098));
#50506=CARTESIAN_POINT('Ctrl Pts',(0.256671831098645,0.0310631340313012,
-0.837462975757093));
#50507=CARTESIAN_POINT('Ctrl Pts',(0.240603708826379,-0.0485564926097166,
-0.841702733364088));
#50508=CARTESIAN_POINT('Ctrl Pts',(0.224535586554113,-0.128176119250734,
-0.845942490971084));
#50509=CARTESIAN_POINT('Ctrl Pts',(0.165024324184724,-0.199028439180819,
-0.850182248578079));
#50510=CARTESIAN_POINT('Ctrl Pts',(0.0893755170973006,-0.228604231411312,
-0.854422006185075));
#50511=CARTESIAN_POINT('Ctrl Pts',(0.0137267100098771,-0.258180023641804,
-0.85866176379207));
#50512=CARTESIAN_POINT('Ctrl Pts',(-0.0780596417955818,-0.246479288172705,
-0.862901521399065));
#50513=CARTESIAN_POINT('Ctrl Pts',(-0.143869140406192,-0.198870681887375,
-0.867141279006061));
#50514=CARTESIAN_POINT('Ctrl Pts',(-0.206091498357299,-0.153857122988121,
-0.871149936130305));
#50515=CARTESIAN_POINT('Ctrl Pts',(-0.245091712734177,-0.0767435354485706,
-0.87515859325455));
#50516=CARTESIAN_POINT('Ctrl Pts',(-0.245422031604165,8.10237884523012E-5,
-0.879167250378794));
#50517=CARTESIAN_POINT('Ctrl Pts',(-0.24539320090154,0.000110883525149794,
-0.890732749621207));
#50518=CARTESIAN_POINT('Ctrl Pts',(-0.244970507036162,-0.0749510535466689,
-0.886817286064372));
#50519=CARTESIAN_POINT('Ctrl Pts',(-0.207996739432263,-0.150372975727332,
-0.882901822507536));
#50520=CARTESIAN_POINT('Ctrl Pts',(-0.148200946425008,-0.195663876087275,
-0.878986358950701));
#50521=CARTESIAN_POINT('Ctrl Pts',(-0.0834526312922395,-0.244705946468324,
-0.874746601343706));
#50522=CARTESIAN_POINT('Ctrl Pts',(0.00805468314886303,-0.258419163348866,
-0.870506843736711));
#50523=CARTESIAN_POINT('Ctrl Pts',(0.0843346299002956,-0.230511481549932,
-0.866267086129716));
#50524=CARTESIAN_POINT('Ctrl Pts',(0.160614576651729,-0.202603799750998,
-0.862027328522721));
#50525=CARTESIAN_POINT('Ctrl Pts',(0.221667155713491,-0.133075219272589,
-0.857787570915725));
#50526=CARTESIAN_POINT('Ctrl Pts',(0.23947956825832,-0.0538275887772554,
-0.853547813308729));
#50527=CARTESIAN_POINT('Ctrl Pts',(0.257291980803149,0.0254200417180767,
-0.849308055701734));
#50528=CARTESIAN_POINT('Ctrl Pts',(0.231864226831043,0.114386722230333,
-0.845068298094739));
#50529=CARTESIAN_POINT('Ctrl Pts',(0.174863341012712,0.172251806657105,
-0.840828540487743));
#50530=CARTESIAN_POINT('Ctrl Pts',(0.117862455194381,0.230116891083877,
-0.836588782880748));
#50531=CARTESIAN_POINT('Ctrl Pts',(0.029288437529827,0.256880379425167,
-0.832349025273753));
#50532=CARTESIAN_POINT('Ctrl Pts',(-0.0502182316557958,0.240262361047521,
-0.828109267666757));
#50533=CARTESIAN_POINT('Ctrl Pts',(-0.12972490084142,0.223644342669875,
-0.823869510059762));
#50534=CARTESIAN_POINT('Ctrl Pts',(-0.200164221548112,0.163644817573289,
-0.819629752452767));
#50535=CARTESIAN_POINT('Ctrl Pts',(-0.229216469518364,0.08779341107567,
-0.815389994845771));
#50536=CARTESIAN_POINT('Ctrl Pts',(-0.23985414079302,0.0600199207465147,
-0.813837579770917));
#50537=CARTESIAN_POINT('Ctrl Pts',(-0.244943021197934,0.0301211587088129,
-0.812285164696062));
#50538=CARTESIAN_POINT('Ctrl Pts',(-0.244760945085023,0.000162685199137168,
-0.810732749621207));
#50539=CARTESIAN_POINT('Origin',(0.,0.,-0.775));
#50540=CARTESIAN_POINT('',(-0.244760954731183,-0.000162685205530727,-0.719167250378794));
#50541=CARTESIAN_POINT('',(-0.244799701406111,-0.000182046177014158,-0.730732749621206));
#50542=CARTESIAN_POINT('',(-0.24505,-3.00099698131059E-17,-0.775));
#50543=CARTESIAN_POINT('Ctrl Pts',(-0.244760954731183,-0.000162685205530727,
-0.719167250378794));
#50544=CARTESIAN_POINT('Ctrl Pts',(-0.244445767826903,0.0516975965821623,
-0.721854592910934));
#50545=CARTESIAN_POINT('Ctrl Pts',(-0.2283355747708,0.103736810422125,-0.724541935443075));
#50546=CARTESIAN_POINT('Ctrl Pts',(-0.197871599550311,0.145240172703587,
-0.727229277975215));
#50547=CARTESIAN_POINT('Ctrl Pts',(-0.149809296685806,0.210719058943139,
-0.731469035582211));
#50548=CARTESIAN_POINT('Ctrl Pts',(-0.0660195162091051,0.249973539909514,
-0.735708793189205));
#50549=CARTESIAN_POINT('Ctrl Pts',(0.0150524165496374,0.244992453825791,
-0.739948550796201));
#50550=CARTESIAN_POINT('Ctrl Pts',(0.0961243493083799,0.240011367742068,
-0.744188308403196));
#50551=CARTESIAN_POINT('Ctrl Pts',(0.174478434349164,0.190794714608247,
-0.748428066010191));
#50552=CARTESIAN_POINT('Ctrl Pts',(0.214163410394044,0.119924606832621,
-0.752667823617187));
#50553=CARTESIAN_POINT('Ctrl Pts',(0.253848386438923,0.049054499056996,
-0.756907581224182));
#50554=CARTESIAN_POINT('Ctrl Pts',(0.2548642534879,-0.0434690633604349,
-0.761147338831177));
#50555=CARTESIAN_POINT('Ctrl Pts',(0.216744900531158,-0.11519342763068,
-0.765387096438173));
#50556=CARTESIAN_POINT('Ctrl Pts',(0.178625547574417,-0.186917791900926,
-0.769626854045168));
#50557=CARTESIAN_POINT('Ctrl Pts',(0.101370974611958,-0.237842958023986,
-0.773866611652163));
#50558=CARTESIAN_POINT('Ctrl Pts',(0.0204279530028463,-0.244602895346069,
-0.778106369259159));
#50559=CARTESIAN_POINT('Ctrl Pts',(-0.0605150686062649,-0.251362832668151,
-0.782346126866154));
#50560=CARTESIAN_POINT('Ctrl Pts',(-0.145146538862028,-0.213957541189255,
-0.786585884473149));
#50561=CARTESIAN_POINT('Ctrl Pts',(-0.194634939306689,-0.149549717741786,
-0.790825642080145));
#50562=CARTESIAN_POINT('Ctrl Pts',(-0.22709063529231,-0.107309501486582,
-0.793606178179695));
#50563=CARTESIAN_POINT('Ctrl Pts',(-0.244431102848988,-0.0534553470905533,
-0.796386714279245));
#50564=CARTESIAN_POINT('Ctrl Pts',(-0.244799711053798,0.000182046184206572,
-0.799167250378795));
#50565=CARTESIAN_POINT('Ctrl Pts',(-0.244760945085023,0.000162685199137168,
-0.810732749621207));
#50566=CARTESIAN_POINT('Ctrl Pts',(-0.244445758193169,-0.0516975945447203,
-0.808045407089066));
#50567=CARTESIAN_POINT('Ctrl Pts',(-0.228335565771977,-0.103736806333797,
-0.805358064556926));
#50568=CARTESIAN_POINT('Ctrl Pts',(-0.197871591752086,-0.145240166979595,
-0.802670722024785));
#50569=CARTESIAN_POINT('Ctrl Pts',(-0.149809290781742,-0.210719050638588,
-0.79843096441779));
#50570=CARTESIAN_POINT('Ctrl Pts',(-0.0660195136072412,-0.249973530057924,
-0.794191206810795));
#50571=CARTESIAN_POINT('Ctrl Pts',(0.0150524159564132,-0.244992444170509,
-0.7899514492038));
#50572=CARTESIAN_POINT('Ctrl Pts',(0.0961243455200677,-0.240011358283093,
-0.785711691596804));
#50573=CARTESIAN_POINT('Ctrl Pts',(0.174478427472875,-0.190794707088926,
-0.781471933989809));
#50574=CARTESIAN_POINT('Ctrl Pts',(0.21416340195375,-0.119924602106329,
-0.777232176382814));
#50575=CARTESIAN_POINT('Ctrl Pts',(0.253848376434623,-0.0490544971237331,
-0.772992418775818));
#50576=CARTESIAN_POINT('Ctrl Pts',(0.254864243443564,0.0434690616472924,
-0.768752661168824));
#50577=CARTESIAN_POINT('Ctrl Pts',(0.216744891989128,0.115193423090842,
-0.764512903561828));
#50578=CARTESIAN_POINT('Ctrl Pts',(0.178625540534692,0.186917784534393,
-0.760273145954833));
#50579=CARTESIAN_POINT('Ctrl Pts',(0.101370970616877,0.237842948650467,
-0.756033388347837));
#50580=CARTESIAN_POINT('Ctrl Pts',(0.0204279521977738,0.244602885706138,
-0.751793630740841));
#50581=CARTESIAN_POINT('Ctrl Pts',(-0.0605150662213308,0.251362822761809,
-0.747553873133846));
#50582=CARTESIAN_POINT('Ctrl Pts',(-0.145146533141725,0.213957532757076,
-0.743314115526851));
#50583=CARTESIAN_POINT('Ctrl Pts',(-0.194634931636022,0.149549711847952,
-0.739074357919856));
#50584=CARTESIAN_POINT('Ctrl Pts',(-0.227090626342544,0.107309497257462,
-0.736293821820306));
#50585=CARTESIAN_POINT('Ctrl Pts',(-0.244431093215825,0.0534553449838617,
-0.733513285720756));
#50586=CARTESIAN_POINT('Ctrl Pts',(-0.244799701406111,-0.000182046177014158,
-0.730732749621206));
#50587=CARTESIAN_POINT('Origin',(0.,0.,-0.775));
#50588=CARTESIAN_POINT('',(-0.245393210572617,-0.000110883529508943,-0.639167250378794));
#50589=CARTESIAN_POINT('',(-0.245422021931952,-8.10237852447184E-5,-0.650732749621206));
#50590=CARTESIAN_POINT('',(-0.24505,-3.00099698131059E-17,-0.775));
#50591=CARTESIAN_POINT('Ctrl Pts',(-0.245393210572617,-0.000110883529508943,
-0.639167250378794));
#50592=CARTESIAN_POINT('Ctrl Pts',(-0.244970516690577,0.0749510565005375,
-0.643082713935629));
#50593=CARTESIAN_POINT('Ctrl Pts',(-0.207996747629523,0.150372981653613,
-0.646998177492464));
#50594=CARTESIAN_POINT('Ctrl Pts',(-0.148200952265686,0.195663883798494,
-0.650913641049299));
#50595=CARTESIAN_POINT('Ctrl Pts',(-0.0834526345811506,0.244705956112317,
-0.655153398656294));
#50596=CARTESIAN_POINT('Ctrl Pts',(0.00805468346630517,0.258419173533304,
-0.659393156263289));
#50597=CARTESIAN_POINT('Ctrl Pts',(0.0843346332239721,0.230511490634511,
-0.663632913870285));
#50598=CARTESIAN_POINT('Ctrl Pts',(0.160614582981637,0.20260380773572,-0.66787267147728));
#50599=CARTESIAN_POINT('Ctrl Pts',(0.221667164449512,0.133075224517152,
-0.672112429084275));
#50600=CARTESIAN_POINT('Ctrl Pts',(0.239479577696338,0.053827590898629,
-0.676352186691271));
#50601=CARTESIAN_POINT('Ctrl Pts',(0.257291990943163,-0.0254200427198954,
-0.680591944298266));
#50602=CARTESIAN_POINT('Ctrl Pts',(0.231864235968934,-0.114386726738377,
-0.684831701905261));
#50603=CARTESIAN_POINT('Ctrl Pts',(0.174863347904167,-0.172251813445643,
-0.689071459512257));
#50604=CARTESIAN_POINT('Ctrl Pts',(0.117862459839398,-0.23011690015291,
-0.693311217119252));
#50605=CARTESIAN_POINT('Ctrl Pts',(0.0292884386840905,-0.256880389548962,
-0.697550974726248));
#50606=CARTESIAN_POINT('Ctrl Pts',(-0.0502182336349338,-0.240262370516387,
-0.701790732333243));
#50607=CARTESIAN_POINT('Ctrl Pts',(-0.129724905953956,-0.223644351483812,
-0.706030489940239));
#50608=CARTESIAN_POINT('Ctrl Pts',(-0.200164229436694,-0.163644824022614,
-0.710270247547233));
#50609=CARTESIAN_POINT('Ctrl Pts',(-0.229216478551909,-0.0877934145356514,
-0.714510005154228));
#50610=CARTESIAN_POINT('Ctrl Pts',(-0.239854150245803,-0.0600199231119234,
-0.716062420229084));
#50611=CARTESIAN_POINT('Ctrl Pts',(-0.244943030851271,-0.0301211598958906,
-0.717614835303939));
#50612=CARTESIAN_POINT('Ctrl Pts',(-0.244760954731183,-0.000162685205530727,
-0.719167250378794));
#50613=CARTESIAN_POINT('Ctrl Pts',(-0.244799701406111,-0.000182046177014158,
-0.730732749621206));
#50614=CARTESIAN_POINT('Ctrl Pts',(-0.244993146475634,-0.0283308750298025,
-0.729273528113761));
#50615=CARTESIAN_POINT('Ctrl Pts',(-0.240512310992863,-0.0564200049260635,
-0.727814306606315));
#50616=CARTESIAN_POINT('Ctrl Pts',(-0.231088843712454,-0.0827394660268344,
-0.726355085098869));
#50617=CARTESIAN_POINT('Ctrl Pts',(-0.203709027226386,-0.159210471178991,
-0.722115327491874));
#50618=CARTESIAN_POINT('Ctrl Pts',(-0.134604064186045,-0.220742129669793,
-0.717875569884879));
#50619=CARTESIAN_POINT('Ctrl Pts',(-0.0554814345597428,-0.239101826312468,
-0.713635812277884));
#50620=CARTESIAN_POINT('Ctrl Pts',(0.023641195066559,-0.257461522955143,
-0.709396054670889));
#50621=CARTESIAN_POINT('Ctrl Pts',(0.112781491278821,-0.23264925774969,
-0.705156297063893));
#50622=CARTESIAN_POINT('Ctrl Pts',(0.171039147757949,-0.176049660212677,
-0.700916539456897));
#50623=CARTESIAN_POINT('Ctrl Pts',(0.229296804237077,-0.119450062675664,
-0.696676781849902));
#50624=CARTESIAN_POINT('Ctrl Pts',(0.256671820983071,-0.0310631328070899,
-0.692437024242907));
#50625=CARTESIAN_POINT('Ctrl Pts',(0.24060369934406,0.0485564906960756,
-0.688197266635912));
#50626=CARTESIAN_POINT('Ctrl Pts',(0.224535577705048,0.128176114199242,
-0.683957509028917));
#50627=CARTESIAN_POINT('Ctrl Pts',(0.165024317681031,0.199028431337,-0.679717751421921));
#50628=CARTESIAN_POINT('Ctrl Pts',(0.0893755135749676,0.228604222401896,
-0.675477993814925));
#50629=CARTESIAN_POINT('Ctrl Pts',(0.013726709468904,0.258180013466792,
-0.67123823620793));
#50630=CARTESIAN_POINT('Ctrl Pts',(-0.0780596387192057,0.246479278458826,
-0.666998478600936));
#50631=CARTESIAN_POINT('Ctrl Pts',(-0.14386913473623,0.198870674049778,
-0.66275872099394));
#50632=CARTESIAN_POINT('Ctrl Pts',(-0.206091490235119,0.153857116924535,
-0.658750063869696));
#50633=CARTESIAN_POINT('Ctrl Pts',(-0.245091703074977,0.0767435324240782,
-0.654741406745451));
#50634=CARTESIAN_POINT('Ctrl Pts',(-0.245422021931952,-8.10237852447184E-5,
-0.650732749621206));
#50635=CARTESIAN_POINT('Origin',(0.,0.,-0.775));
#50636=CARTESIAN_POINT('',(-0.245099038793128,0.000222287303026779,-0.559167250378794));
#50637=CARTESIAN_POINT('',(-0.245044311916972,0.000225594359514621,-0.570732749621207));
#50638=CARTESIAN_POINT('',(-0.24505,-3.00099698131059E-17,-0.775));
#50639=CARTESIAN_POINT('Ctrl Pts',(-0.245099038793128,0.000222287303026779,
-0.559167250378794));
#50640=CARTESIAN_POINT('Ctrl Pts',(-0.245260304066475,0.0176033761932229,
-0.560071077353328));
#50641=CARTESIAN_POINT('Ctrl Pts',(-0.243569224089339,0.0349533179170207,
-0.560974904327863));
#50642=CARTESIAN_POINT('Ctrl Pts',(-0.239909555455349,0.0518775758568482,
-0.561878731302397));
#50643=CARTESIAN_POINT('Ctrl Pts',(-0.222742433464957,0.131267496012865,
-0.566118488909392));
#50644=CARTESIAN_POINT('Ctrl Pts',(-0.162257506943935,0.201290458332522,
-0.570358246516388));
#50645=CARTESIAN_POINT('Ctrl Pts',(-0.0862071182953996,0.229817776576942,
-0.574598004123383));
#50646=CARTESIAN_POINT('Ctrl Pts',(-0.0101567296468654,0.258345094821361,
-0.578837761730378));
#50647=CARTESIAN_POINT('Ctrl Pts',(0.0814591211291825,0.245376768990544,
-0.583077519337374));
#50648=CARTESIAN_POINT('Ctrl Pts',(0.146604267229997,0.196863065366569,
-0.587317276944369));
#50649=CARTESIAN_POINT('Ctrl Pts',(0.211749413330811,0.148349361742594,
-0.591557034551365));
#50650=CARTESIAN_POINT('Ctrl Pts',(0.250423854756394,0.0642902803254605,
-0.59579679215836));
#50651=CARTESIAN_POINT('Ctrl Pts',(0.244882569690129,-0.0167452900101996,
-0.600036549765355));
#50652=CARTESIAN_POINT('Ctrl Pts',(0.239341284623863,-0.097780860345862,
-0.60427630737235));
#50653=CARTESIAN_POINT('Ctrl Pts',(0.18958427306575,-0.175792919600049,
-0.608516064979345));
#50654=CARTESIAN_POINT('Ctrl Pts',(0.11844158046912,-0.214987138432845,
-0.612755822586341));
#50655=CARTESIAN_POINT('Ctrl Pts',(0.0472988878724918,-0.254181357265641,
-0.616995580193336));
#50656=CARTESIAN_POINT('Ctrl Pts',(-0.0452294857626519,-0.254557735677044,
-0.621235337800332));
#50657=CARTESIAN_POINT('Ctrl Pts',(-0.116688680112832,-0.215943579689445,
-0.625475095407327));
#50658=CARTESIAN_POINT('Ctrl Pts',(-0.188147874463012,-0.177329423701845,
-0.629714853014322));
#50659=CARTESIAN_POINT('Ctrl Pts',(-0.238537889528229,-0.099724733315242,
-0.633954610621317));
#50660=CARTESIAN_POINT('Ctrl Pts',(-0.244738238400031,-0.0187369245186125,
-0.638194368228313));
#50661=CARTESIAN_POINT('Ctrl Pts',(-0.245212495759632,-0.0125422627094244,
-0.638518662278473));
#50662=CARTESIAN_POINT('Ctrl Pts',(-0.245428219737942,-0.00632780783282481,
-0.638842956328634));
#50663=CARTESIAN_POINT('Ctrl Pts',(-0.245393210572617,-0.000110883529508943,
-0.639167250378794));
#50664=CARTESIAN_POINT('Ctrl Pts',(-0.245422021931952,-8.10237852447184E-5,
-0.650732749621206));
#50665=CARTESIAN_POINT('Ctrl Pts',(-0.245441064929381,-0.00450998627238757,
-0.650501649138455));
#50666=CARTESIAN_POINT('Ctrl Pts',(-0.24533158610744,-0.00893798815586689,
-0.650270548655704));
#50667=CARTESIAN_POINT('Ctrl Pts',(-0.24509062560664,-0.0133588235451446,
-0.650039448172953));
#50668=CARTESIAN_POINT('Ctrl Pts',(-0.240669976614088,-0.0944632429208891,
-0.645799690565958));
#50669=CARTESIAN_POINT('Ctrl Pts',(-0.191996034783046,-0.173155607862247,
-0.641559932958963));
#50670=CARTESIAN_POINT('Ctrl Pts',(-0.121401899903836,-0.213329443880829,
-0.637320175351968));
#50671=CARTESIAN_POINT('Ctrl Pts',(-0.0508077650246259,-0.253503279899411,
-0.633080417744973));
#50672=CARTESIAN_POINT('Ctrl Pts',(0.0417065629027502,-0.255158586995217,
-0.628840660137977));
#50673=CARTESIAN_POINT('Ctrl Pts',(0.113692668157028,-0.217535859421155,
-0.624600902530982));
#50674=CARTESIAN_POINT('Ctrl Pts',(0.185678773411305,-0.179913131847094,
-0.620361144923986));
#50675=CARTESIAN_POINT('Ctrl Pts',(0.237136655992484,-0.103012369603164,
-0.616121387316991));
#50676=CARTESIAN_POINT('Ctrl Pts',(0.244455858570574,-0.0221180048216005,
-0.611881629709996));
#50677=CARTESIAN_POINT('Ctrl Pts',(0.251775061148664,0.0587763599599641,
-0.607641872103));
#50678=CARTESIAN_POINT('Ctrl Pts',(0.214955583723666,0.143664327279164,
-0.603402114496005));
#50679=CARTESIAN_POINT('Ctrl Pts',(0.150891333643671,0.193596689945875,
-0.59916235688901));
#50680=CARTESIAN_POINT('Ctrl Pts',(0.0868270835636758,0.243529052612585,
-0.594922599282015));
#50681=CARTESIAN_POINT('Ctrl Pts',(-0.00448193917131465,0.258505810626804,
-0.590682841675019));
#50682=CARTESIAN_POINT('Ctrl Pts',(-0.0811403498896434,0.231655167321066,
-0.586443084068023));
#50683=CARTESIAN_POINT('Ctrl Pts',(-0.157798760607972,0.204804524015327,
-0.582203326461028));
#50684=CARTESIAN_POINT('Ctrl Pts',(-0.219806559309638,0.13612647938963,
-0.577963568854034));
#50685=CARTESIAN_POINT('Ctrl Pts',(-0.238712663051953,0.057132630128584,
-0.573723811247038));
#50686=CARTESIAN_POINT('Ctrl Pts',(-0.243158618586795,0.0385564525021716,
-0.572726790705094));
#50687=CARTESIAN_POINT('Ctrl Pts',(-0.245221044763826,0.0194098095327841,
-0.571729770163151));
#50688=CARTESIAN_POINT('Ctrl Pts',(-0.245044311916972,0.000225594359514621,
-0.570732749621207));
#50689=CARTESIAN_POINT('Origin',(0.,0.,-0.775));
#50690=CARTESIAN_POINT('',(-0.24464554858441,-3.8505879792117E-6,-0.479167250378794));
#50691=CARTESIAN_POINT('',(-0.244649643429401,-3.34626570719463E-5,-0.490732749621207));
#50692=CARTESIAN_POINT('',(-0.24505,-3.00099698131059E-17,-0.775));
#50693=CARTESIAN_POINT('Ctrl Pts',(-0.244645577937762,-3.85030852002866E-6,
-0.479167250378794));
#50694=CARTESIAN_POINT('Ctrl Pts',(-0.244639821044035,0.0411869810206832,
-0.481299198378023));
#50695=CARTESIAN_POINT('Ctrl Pts',(-0.23479682609857,0.0823803969011494,
-0.483431146377252));
#50696=CARTESIAN_POINT('Ctrl Pts',(-0.21513194374638,0.11817835865959,-0.485563094376481));
#50697=CARTESIAN_POINT('Ctrl Pts',(-0.176024829232561,0.18936896965721,
-0.489802851983476));
#50698=CARTESIAN_POINT('Ctrl Pts',(-0.0980737284097471,0.239221426655701,
-0.494042609590472));
#50699=CARTESIAN_POINT('Ctrl Pts',(-0.0170450010169084,0.244861890901583,
-0.498282367197467));
#50700=CARTESIAN_POINT('Ctrl Pts',(0.0639837263759303,0.250502355147466,
-0.502522124804463));
#50701=CARTESIAN_POINT('Ctrl Pts',(0.148090080338794,0.21193082664074,-0.506761882411458));
#50702=CARTESIAN_POINT('Ctrl Pts',(0.196683481900857,0.146845107589328,
-0.511001640018453));
#50703=CARTESIAN_POINT('Ctrl Pts',(0.245276883462918,0.0817593885379164,
-0.515241397625448));
#50704=CARTESIAN_POINT('Ctrl Pts',(0.25835733262418,-0.00984052105818028,
-0.519481155232444));
#50705=CARTESIAN_POINT('Ctrl Pts',(0.229923117474086,-0.0859257686992934,
-0.523720912839439));
#50706=CARTESIAN_POINT('Ctrl Pts',(0.201488902323992,-0.162011016340406,
-0.527960670446434));
#50707=CARTESIAN_POINT('Ctrl Pts',(0.131540022862543,-0.222581602026536,
-0.53220042805343));
#50708=CARTESIAN_POINT('Ctrl Pts',(0.0521711738374254,-0.239845880298143,
-0.536440185660425));
#50709=CARTESIAN_POINT('Ctrl Pts',(-0.0271976751876943,-0.257110158569751,
-0.54067994326742));
#50710=CARTESIAN_POINT('Ctrl Pts',(-0.115986493776483,-0.231068129426834,
-0.544919700874415));
#50711=CARTESIAN_POINT('Ctrl Pts',(-0.173456244340995,-0.173668675859187,
-0.549159458481411));
#50712=CARTESIAN_POINT('Ctrl Pts',(-0.218674655184041,-0.128505576174691,
-0.552495389113872));
#50713=CARTESIAN_POINT('Ctrl Pts',(-0.244503825571495,-0.0639294900702973,
-0.555831319746333));
#50714=CARTESIAN_POINT('Ctrl Pts',(-0.245099038793128,0.000222287303026779,
-0.559167250378794));
#50715=CARTESIAN_POINT('Ctrl Pts',(-0.245044311916972,0.000225594359514621,
-0.570732749621207));
#50716=CARTESIAN_POINT('Ctrl Pts',(-0.244469501139266,-0.0621696753357292,
-0.567490012556155));
#50717=CARTESIAN_POINT('Ctrl Pts',(-0.220208228315207,-0.124962394507208,
-0.564247275491103));
#50718=CARTESIAN_POINT('Ctrl Pts',(-0.17722756994711,-0.169818318733306,
-0.561004538426051));
#50719=CARTESIAN_POINT('Ctrl Pts',(-0.121031964316992,-0.228465764437753,
-0.556764780819056));
#50720=CARTESIAN_POINT('Ctrl Pts',(-0.0328363442737951,-0.256451001950254,
-0.552525023212061));
#50721=CARTESIAN_POINT('Ctrl Pts',(0.0468924303104948,-0.240933544585099,
-0.548285265605066));
#50722=CARTESIAN_POINT('Ctrl Pts',(0.126621204894785,-0.225416087219944,
-0.544045507998071));
#50723=CARTESIAN_POINT('Ctrl Pts',(0.197883134020166,-0.166395934977131,
-0.539805750391075));
#50724=CARTESIAN_POINT('Ctrl Pts',(0.227981055415858,-0.0909533468226233,
-0.535565992784079));
#50725=CARTESIAN_POINT('Ctrl Pts',(0.258078976811549,-0.0155107586681155,
-0.531326235177084));
#50726=CARTESIAN_POINT('Ctrl Pts',(0.247012890477551,0.0763542653980887,
-0.527086477570089));
#50727=CARTESIAN_POINT('Ctrl Pts',(0.199860256777428,0.142491230213038,
-0.522846719963094));
#50728=CARTESIAN_POINT('Ctrl Pts',(0.152707623077304,0.208628195027989,
-0.518606962356099));
#50729=CARTESIAN_POINT('Ctrl Pts',(0.0694684420110575,0.249037100591685,
-0.514367204749104));
#50730=CARTESIAN_POINT('Ctrl Pts',(-0.0116645930152598,0.245177099657682,
-0.510127447142108));
#50731=CARTESIAN_POINT('Ctrl Pts',(-0.092797628041576,0.241317098723679,
-0.505887689535113));
#50732=CARTESIAN_POINT('Ctrl Pts',(-0.171824517027962,0.193188191291977,
-0.501647931928117));
#50733=CARTESIAN_POINT('Ctrl Pts',(-0.212485295577484,0.122873398626858,
-0.497408174321122));
#50734=CARTESIAN_POINT('Ctrl Pts',(-0.233825192069005,0.0859702587750484,
-0.495183032754483));
#50735=CARTESIAN_POINT('Ctrl Pts',(-0.244597375570812,0.0429561510690604,
-0.492957891187845));
#50736=CARTESIAN_POINT('Ctrl Pts',(-0.244649643429401,-3.34626570719463E-5,
-0.490732749621207));
#50737=CARTESIAN_POINT('Origin',(0.,0.,-0.775));
#50738=CARTESIAN_POINT('',(-0.245113213433533,-0.000220732632699366,-0.399167250378794));
#50739=CARTESIAN_POINT('',(-0.245167474403332,-0.000212043108657725,-0.410732749621206));
#50740=CARTESIAN_POINT('',(-0.24505,-3.00099698131059E-17,-0.775));
#50741=CARTESIAN_POINT('Ctrl Pts',(-0.245113213433533,-0.000220732632699366,
-0.399167250378794));
#50742=CARTESIAN_POINT('Ctrl Pts',(-0.2445143688444,0.0643856472039739,
-0.402527319402718));
#50743=CARTESIAN_POINT('Ctrl Pts',(-0.21826929847075,0.129422269040789,
-0.405887388426641));
#50744=CARTESIAN_POINT('Ctrl Pts',(-0.172465708082888,0.174652389652183,
-0.409247457450565));
#50745=CARTESIAN_POINT('Ctrl Pts',(-0.114670430845441,0.23172405888341,
-0.41348721505756));
#50746=CARTESIAN_POINT('Ctrl Pts',(-0.0257349357162201,0.257260685412779,
-0.417726972664556));
#50747=CARTESIAN_POINT('Ctrl Pts',(0.0535344400129061,0.239545280496294,
-0.421966730271551));
#50748=CARTESIAN_POINT('Ctrl Pts',(0.132803815742034,0.221829875579809,
-0.426206487878547));
#50749=CARTESIAN_POINT('Ctrl Pts',(0.202407072071065,0.160862439217467,
-0.430446245485542));
#50750=CARTESIAN_POINT('Ctrl Pts',(0.230408096763762,0.0846167041501249,
-0.434686003092537));
#50751=CARTESIAN_POINT('Ctrl Pts',(0.258409121456458,0.00837096908278148,
-0.438925760699532));
#50752=CARTESIAN_POINT('Ctrl Pts',(0.244807914512817,-0.0831530646895631,
-0.443165518306528));
#50753=CARTESIAN_POINT('Ctrl Pts',(0.195845127511443,-0.147961358825947,
-0.447405275913524));
#50754=CARTESIAN_POINT('Ctrl Pts',(0.14688234051007,-0.212769652962328,
-0.451645033520519));
#50755=CARTESIAN_POINT('Ctrl Pts',(0.0625579734509672,-0.250862207462751,
-0.455884791127514));
#50756=CARTESIAN_POINT('Ctrl Pts',(-0.0184373635888685,-0.24476098810769,
-0.460124548734509));
#50757=CARTESIAN_POINT('Ctrl Pts',(-0.0994327006287077,-0.238659768752629,
-0.464364306341504));
#50758=CARTESIAN_POINT('Ctrl Pts',(-0.177099007649279,-0.18836477554208,
-0.4686040639485));
#50759=CARTESIAN_POINT('Ctrl Pts',(-0.215800597057152,-0.116952896438431,
-0.472843821555495));
#50760=CARTESIAN_POINT('Ctrl Pts',(-0.235041221062436,-0.0814502430237733,
-0.474951631163261));
#50761=CARTESIAN_POINT('Ctrl Pts',(-0.244651269650652,-0.0407283098445718,
-0.477059440771028));
#50762=CARTESIAN_POINT('Ctrl Pts',(-0.244645577937762,-3.85030852002866E-6,
-0.479167250378794));
#50763=CARTESIAN_POINT('Ctrl Pts',(-0.244649643429401,-3.34626570719463E-5,
-0.490732749621207));
#50764=CARTESIAN_POINT('Ctrl Pts',(-0.244696966111197,-0.038955734695813,
-0.48871813358085));
#50765=CARTESIAN_POINT('Ctrl Pts',(-0.235956883659052,-0.0778579283560022,
-0.486703517540493));
#50766=CARTESIAN_POINT('Ctrl Pts',(-0.218316435692479,-0.112186482400046,
-0.484688901500136));
#50767=CARTESIAN_POINT('Ctrl Pts',(-0.181192129145293,-0.184430892863294,
-0.480449143893141));
#50768=CARTESIAN_POINT('Ctrl Pts',(-0.104648847938264,-0.236419035891254,
-0.476209386286145));
#50769=CARTESIAN_POINT('Ctrl Pts',(-0.023807000921954,-0.2442971543712,
-0.47196962867915));
#50770=CARTESIAN_POINT('Ctrl Pts',(0.0570348460943559,-0.252175272851145,
-0.467729871072154));
#50771=CARTESIAN_POINT('Ctrl Pts',(0.142175258919946,-0.215943366783077,
-0.463490113465159));
#50772=CARTESIAN_POINT('Ctrl Pts',(0.192549200611132,-0.152225747726141,
-0.459250355858164));
#50773=CARTESIAN_POINT('Ctrl Pts',(0.242923142302319,-0.0885081286692047,
-0.455010598251169));
#50774=CARTESIAN_POINT('Ctrl Pts',(0.258530612859102,0.00269520337659913,
-0.450770840644173));
#50775=CARTESIAN_POINT('Ctrl Pts',(0.232210425323849,0.0795373578746301,
-0.446531083037178));
#50776=CARTESIAN_POINT('Ctrl Pts',(0.205890237788597,0.156379512372661,
-0.442291325430183));
#50777=CARTESIAN_POINT('Ctrl Pts',(0.137642392161309,0.218860489322919,
-0.438051567823187));
#50778=CARTESIAN_POINT('Ctrl Pts',(0.0587810966101972,0.238312097066141,
-0.433811810216192));
#50779=CARTESIAN_POINT('Ctrl Pts',(-0.0200801989409146,0.257763704809364,
-0.429572052609197));
#50780=CARTESIAN_POINT('Ctrl Pts',(-0.10955494441585,0.23418594334555,-0.425332295002201));
#50781=CARTESIAN_POINT('Ctrl Pts',(-0.168589377899256,0.178397013950162,
-0.421092537395206));
#50782=CARTESIAN_POINT('Ctrl Pts',(-0.216672645775806,0.132957193859089,
-0.417639274803873));
#50783=CARTESIAN_POINT('Ctrl Pts',(-0.244561732339873,0.0661484020676576,
-0.414186012212539));
#50784=CARTESIAN_POINT('Ctrl Pts',(-0.245167474403332,-0.000212043108657725,
-0.410732749621206));
#50785=CARTESIAN_POINT('Origin',(0.,0.,-0.775));
#50786=CARTESIAN_POINT('',(-0.245384525130581,0.000118217037109843,-0.319167250378794));
#50787=CARTESIAN_POINT('',(-0.245346855243246,0.000144723277665203,-0.330732749621206));
#50788=CARTESIAN_POINT('',(-0.24505,-3.00099698131059E-17,-0.775));
#50789=CARTESIAN_POINT('Ctrl Pts',(-0.245384525130581,0.000118217037109843,
-0.319167250378794));
#50790=CARTESIAN_POINT('Ctrl Pts',(-0.245424204817052,0.00679851531508335,
-0.319515682820417));
#50791=CARTESIAN_POINT('Ctrl Pts',(-0.245175118904715,0.013475809046111,
-0.31986411526204));
#50792=CARTESIAN_POINT('Ctrl Pts',(-0.244627714853342,0.0201285564437554,
-0.320212547703663));
#50793=CARTESIAN_POINT('Ctrl Pts',(-0.237966852621071,0.1010797912231,-0.324452305310658));
#50794=CARTESIAN_POINT('Ctrl Pts',(-0.18713628029174,0.17839663610918,-0.328692062917654));
#50795=CARTESIAN_POINT('Ctrl Pts',(-0.115458625868584,0.21660374741823,
-0.332931820524649));
#50796=CARTESIAN_POINT('Ctrl Pts',(-0.0437809714454274,0.254810858727282,
-0.337171578131644));
#50797=CARTESIAN_POINT('Ctrl Pts',(0.0487437650715545,0.2539082364593,-0.34141133573864));
#50798=CARTESIAN_POINT('Ctrl Pts',(0.119662392121641,0.214310031467542,
-0.345651093345635));
#50799=CARTESIAN_POINT('Ctrl Pts',(0.190581019171727,0.174711826475785,
-0.349890850952631));
#50800=CARTESIAN_POINT('Ctrl Pts',(0.239893536754919,0.0964180387602521,
-0.354130608559626));
#50801=CARTESIAN_POINT('Ctrl Pts',(0.24497384693941,0.0153522633190858,
-0.358370366166621));
#50802=CARTESIAN_POINT('Ctrl Pts',(0.250054157123901,-0.0657135121220805,
-0.362610123773617));
#50803=CARTESIAN_POINT('Ctrl Pts',(0.210902259909693,-0.14955127528888,
-0.366849881380612));
#50804=CARTESIAN_POINT('Ctrl Pts',(0.145482248480625,-0.197693684911225,
-0.371089638987607));
#50805=CARTESIAN_POINT('Ctrl Pts',(0.0800622370515574,-0.245836094533568,
-0.375329396594603));
#50806=CARTESIAN_POINT('Ctrl Pts',(-0.0116258885923681,-0.258283150611457,
-0.379569154201598));
#50807=CARTESIAN_POINT('Ctrl Pts',(-0.0875127997102276,-0.229323761443049,
-0.383808911808593));
#50808=CARTESIAN_POINT('Ctrl Pts',(-0.163399710828089,-0.20036437227464,
-0.388048669415588));
#50809=CARTESIAN_POINT('Ctrl Pts',(-0.223485407419884,-0.129998537859931,
-0.392288427022584));
#50810=CARTESIAN_POINT('Ctrl Pts',(-0.240200726042946,-0.0505122646860321,
-0.396528184629579));
#50811=CARTESIAN_POINT('Ctrl Pts',(-0.243668913689063,-0.0340200088772053,
-0.397407873212651));
#50812=CARTESIAN_POINT('Ctrl Pts',(-0.245269994959254,-0.01713511573949,
-0.398287561795722));
#50813=CARTESIAN_POINT('Ctrl Pts',(-0.245113213433533,-0.000220732632699366,
-0.399167250378794));
#50814=CARTESIAN_POINT('Ctrl Pts',(-0.245167474403332,-0.000212043108657725,
-0.410732749621206));
#50815=CARTESIAN_POINT('Ctrl Pts',(-0.24530543469482,-0.0153259123809456,
-0.409946254605544));
#50816=CARTESIAN_POINT('Ctrl Pts',(-0.244028154161137,-0.0304165250311018,
-0.409159759589882));
#50817=CARTESIAN_POINT('Ctrl Pts',(-0.241251881014642,-0.0452261299872512,
-0.40837326457422));
#50818=CARTESIAN_POINT('Ctrl Pts',(-0.226285829154746,-0.125060247202309,
-0.404133506967224));
#50819=CARTESIAN_POINT('Ctrl Pts',(-0.167759603943079,-0.196728384305462,
-0.399893749360229));
#50820=CARTESIAN_POINT('Ctrl Pts',(-0.092526835449539,-0.227346998327305,
-0.395653991753234));
#50821=CARTESIAN_POINT('Ctrl Pts',(-0.0172940669560004,-0.257965612349148,
-0.391414234146239));
#50822=CARTESIAN_POINT('Ctrl Pts',(0.0746452448194102,-0.247534703289683,
-0.387174476539243));
#50823=CARTESIAN_POINT('Ctrl Pts',(0.141106519229503,-0.200840292665299,
-0.382934718932248));
#50824=CARTESIAN_POINT('Ctrl Pts',(0.207567793639597,-0.154145882040914,
-0.378694961325253));
#50825=CARTESIAN_POINT('Ctrl Pts',(0.248551030684372,-0.0711879698516079,
-0.374455203718257));
#50826=CARTESIAN_POINT('Ctrl Pts',(0.245251862192355,0.00996980529647849,
-0.370215446111262));
#50827=CARTESIAN_POINT('Ctrl Pts',(0.241952693700338,0.0911275804445649,
-0.365975688504267));
#50828=CARTESIAN_POINT('Ctrl Pts',(0.194371119671528,0.170485218551432,
-0.361735930897271));
#50829=CARTESIAN_POINT('Ctrl Pts',(0.124339027986658,0.211630997365796,
-0.357496173290276));
#50830=CARTESIAN_POINT('Ctrl Pts',(0.054306936301789,0.25277677618016,-0.353256415683281));
#50831=CARTESIAN_POINT('Ctrl Pts',(-0.0381756730391405,0.255710695702023,
-0.349016658076286));
#50832=CARTESIAN_POINT('Ctrl Pts',(-0.110674937768999,0.219086583518454,
-0.34477690046929));
#50833=CARTESIAN_POINT('Ctrl Pts',(-0.183174202498859,0.182462471334884,
-0.340537142862295));
#50834=CARTESIAN_POINT('Ctrl Pts',(-0.235690122617646,0.106280327445879,
-0.3362973852553));
#50835=CARTESIAN_POINT('Ctrl Pts',(-0.244126780684619,0.0254948598165568,
-0.332057627648304));
#50836=CARTESIAN_POINT('Ctrl Pts',(-0.245005568572291,0.0170800005335381,
-0.331616001639271));
#50837=CARTESIAN_POINT('Ctrl Pts',(-0.245406099229541,0.00861519547646839,
-0.331174375630239));
#50838=CARTESIAN_POINT('Ctrl Pts',(-0.245346855243246,0.000144723277665203,
-0.330732749621206));
#50839=CARTESIAN_POINT('Origin',(0.,0.,-0.775));
#50840=CARTESIAN_POINT('',(-0.244751705071012,0.000157197749167753,-0.239167250378794));
#50841=CARTESIAN_POINT('',(-0.244719249417263,0.000134367256465015,-0.250732749621206));
#50842=CARTESIAN_POINT('',(-0.24505,-3.00099698131059E-17,-0.775));
#50843=CARTESIAN_POINT('Ctrl Pts',(-0.244751705071012,0.000157197749167753,
-0.239167250378794));
#50844=CARTESIAN_POINT('Ctrl Pts',(-0.244929957152803,0.030584378658343,
-0.240743803845112));
#50845=CARTESIAN_POINT('Ctrl Pts',(-0.239676767767007,0.0609522085494251,
-0.242320357311429));
#50846=CARTESIAN_POINT('Ctrl Pts',(-0.228713449599398,0.0890956496980255,
-0.243896910777747));
#50847=CARTESIAN_POINT('Ctrl Pts',(-0.199230268348596,0.164780598699778,
-0.248136668384742));
#50848=CARTESIAN_POINT('Ctrl Pts',(-0.128450843241183,0.224378537504145,
-0.252376425991738));
#50849=CARTESIAN_POINT('Ctrl Pts',(-0.0488509435112058,0.240544098374202,
-0.256616183598733));
#50850=CARTESIAN_POINT('Ctrl Pts',(0.0307489562187699,0.25670965924426,
-0.260855941205729));
#50851=CARTESIAN_POINT('Ctrl Pts',(0.119169330571309,0.229442842180009,
-0.265095698812724));
#50852=CARTESIAN_POINT('Ctrl Pts',(0.175840192674927,0.171254501831632,
-0.269335456419719));
#50853=CARTESIAN_POINT('Ctrl Pts',(0.232511054778548,0.113066161483252,
-0.273575214026715));
#50854=CARTESIAN_POINT('Ctrl Pts',(0.257432404633245,0.0239562978507422,
-0.27781497163371));
#50855=CARTESIAN_POINT('Ctrl Pts',(0.239169562812728,-0.0551887468503754,
-0.282054729240705));
#50856=CARTESIAN_POINT('Ctrl Pts',(0.220906720992213,-0.134333791551488,
-0.286294486847701));
#50857=CARTESIAN_POINT('Ctrl Pts',(0.15945968749649,-0.203514017321211,
-0.290534244454696));
#50858=CARTESIAN_POINT('Ctrl Pts',(0.0830222481891644,-0.230987410971053,
-0.294774002061691));
#50859=CARTESIAN_POINT('Ctrl Pts',(0.00658480888183648,-0.258460804620896,
-0.299013759668687));
#50860=CARTESIAN_POINT('Ctrl Pts',(-0.0848430362370954,-0.244227366150856,
-0.303253517275682));
#50861=CARTESIAN_POINT('Ctrl Pts',(-0.149311382728958,-0.19481783457953,
-0.307493274882677));
#50862=CARTESIAN_POINT('Ctrl Pts',(-0.208481581199691,-0.149468885079323,
-0.311384600048049));
#50863=CARTESIAN_POINT('Ctrl Pts',(-0.244941378786922,-0.074487961079283,
-0.315275925213421));
#50864=CARTESIAN_POINT('Ctrl Pts',(-0.245384525130581,0.000118217037109843,
-0.319167250378794));
#50865=CARTESIAN_POINT('Ctrl Pts',(-0.245346855243246,0.000144723277665203,
-0.330732749621206));
#50866=CARTESIAN_POINT('Ctrl Pts',(-0.244837337117652,-0.072704174771635,
-0.326934618023243));
#50867=CARTESIAN_POINT('Ctrl Pts',(-0.210320237519882,-0.145972247272856,
-0.323136486425281));
#50868=CARTESIAN_POINT('Ctrl Pts',(-0.153552890361856,-0.191492513662049,
-0.319338354827318));
#50869=CARTESIAN_POINT('Ctrl Pts',(-0.0901849459569572,-0.242305628141694,
-0.315098597220323));
#50870=CARTESIAN_POINT('Ctrl Pts',(0.000908338867999472,-0.258543065731344,
-0.310858839613328));
#50871=CARTESIAN_POINT('Ctrl Pts',(0.0779305665684941,-0.232754591208473,
-0.306619082006332));
#50872=CARTESIAN_POINT('Ctrl Pts',(0.154952794268988,-0.206966116685603,
-0.302379324399337));
#50873=CARTESIAN_POINT('Ctrl Pts',(0.21790396484502,-0.139151730050211,
-0.298139566792341));
#50874=CARTESIAN_POINT('Ctrl Pts',(0.237900147459264,-0.0604267552403789,
-0.293899809185346));
#50875=CARTESIAN_POINT('Ctrl Pts',(0.257896330073507,0.0182982195694519,
-0.289660051578351));
#50876=CARTESIAN_POINT('Ctrl Pts',(0.234937524725965,0.107933782553724,
-0.285420293971356));
#50877=CARTESIAN_POINT('Ctrl Pts',(0.179557936417182,0.167352383919392,
-0.281180536364361));
#50878=CARTESIAN_POINT('Ctrl Pts',(0.124178348108397,0.226770985285061,
-0.276940778757365));
#50879=CARTESIAN_POINT('Ctrl Pts',(0.0363779768383712,0.255972625032124,
-0.27270102115037));
#50880=CARTESIAN_POINT('Ctrl Pts',(-0.0435576694298078,0.241558693502635,
-0.268461263543374));
#50881=CARTESIAN_POINT('Ctrl Pts',(-0.123493315697988,0.227144761973145,
-0.264221505936379));
#50882=CARTESIAN_POINT('Ctrl Pts',(-0.19556423696432,0.169115259167102,
-0.259981748329384));
#50883=CARTESIAN_POINT('Ctrl Pts',(-0.226702081217119,0.0940959041489634,
-0.255741990722389));
#50884=CARTESIAN_POINT('Ctrl Pts',(-0.238965122621183,0.0645509732531478,
-0.254072243688661));
#50885=CARTESIAN_POINT('Ctrl Pts',(-0.244879334034295,0.0323708707275442,
-0.252402496654933));
#50886=CARTESIAN_POINT('Ctrl Pts',(-0.244719249417263,0.000134367256465015,
-0.250732749621206));
#50887=CARTESIAN_POINT('Origin',(0.,0.,-0.775));
#50888=CARTESIAN_POINT('',(-0.244810649818844,-0.000186483096579593,-0.159167250378794));
#50889=CARTESIAN_POINT('',(-0.244854727503173,-0.000201854228764521,-0.170732749621206));
#50890=CARTESIAN_POINT('',(-0.24505,-3.00099698131059E-17,-0.775));
#50891=CARTESIAN_POINT('Ctrl Pts',(-0.244810649818844,-0.000186483096579593,
-0.159167250378794));
#50892=CARTESIAN_POINT('Ctrl Pts',(-0.244428481934693,0.0539105290607768,
-0.161971924869806));
#50893=CARTESIAN_POINT('Ctrl Pts',(-0.226760449543787,0.108234228796465,
-0.164776599360819));
#50894=CARTESIAN_POINT('Ctrl Pts',(-0.193781160300922,0.150654238495037,
-0.167581273851832));
#50895=CARTESIAN_POINT('Ctrl Pts',(-0.143927177997881,0.214779526254686,
-0.171821031458827));
#50896=CARTESIAN_POINT('Ctrl Pts',(-0.0590844826091137,0.251702945519997,
-0.176060789065822));
#50897=CARTESIAN_POINT('Ctrl Pts',(0.0218187482607599,0.244482775158905,
-0.180300546672818));
#50898=CARTESIAN_POINT('Ctrl Pts',(0.102721979130632,0.237262604797812,
-0.184540304279813));
#50899=CARTESIAN_POINT('Ctrl Pts',(0.179685745481613,0.185898844810319,
-0.188780061886808));
#50900=CARTESIAN_POINT('Ctrl Pts',(0.217396571892036,0.113958830238838,
-0.193019819493804));
#50901=CARTESIAN_POINT('Ctrl Pts',(0.25510739830246,0.0420188156673544,
-0.197259577100799));
#50902=CARTESIAN_POINT('Ctrl Pts',(0.253565284772325,-0.050497453488115,
-0.201499334707794));
#50903=CARTESIAN_POINT('Ctrl Pts',(0.213477871231587,-0.121140704416826,
-0.20573909231479));
#50904=CARTESIAN_POINT('Ctrl Pts',(0.17339045769085,-0.191783955345535,
-0.209978849921785));
#50905=CARTESIAN_POINT('Ctrl Pts',(0.0947577441395111,-0.240554188047485,
-0.21421860752878));
#50906=CARTESIAN_POINT('Ctrl Pts',(0.0136587979927169,-0.245074103890555,
-0.218458365135775));
#50907=CARTESIAN_POINT('Ctrl Pts',(-0.0674401481540807,-0.249594019733626,
-0.222698122742771));
#50908=CARTESIAN_POINT('Ctrl Pts',(-0.151005326896335,-0.209863618717812,
-0.226937880349766));
#50909=CARTESIAN_POINT('Ctrl Pts',(-0.198694447570365,-0.144112438610335,
-0.231177637956762));
#50910=CARTESIAN_POINT('Ctrl Pts',(-0.228650373219223,-0.102810828624959,
-0.233840842097439));
#50911=CARTESIAN_POINT('Ctrl Pts',(-0.244450591475787,-0.051242133715127,
-0.236504046238116));
#50912=CARTESIAN_POINT('Ctrl Pts',(-0.244751705071012,0.000157197749167753,
-0.239167250378794));
#50913=CARTESIAN_POINT('Ctrl Pts',(-0.244719249417263,0.000134367256465015,
-0.250732749621206));
#50914=CARTESIAN_POINT('Ctrl Pts',(-0.244472853316488,-0.0494828221095842,
-0.248162739047938));
#50915=CARTESIAN_POINT('Ctrl Pts',(-0.229836337324464,-0.0992336263609378,
-0.24559272847467));
#50916=CARTESIAN_POINT('Ctrl Pts',(-0.201810735292949,-0.139715067653531,
-0.243022717901403));
#50917=CARTESIAN_POINT('Ctrl Pts',(-0.155576777876713,-0.20649747720766,
-0.238782960294407));
#50918=CARTESIAN_POINT('Ctrl Pts',(-0.0729040958049717,-0.248053089085685,
-0.234543202687412));
#50919=CARTESIAN_POINT('Ctrl Pts',(0.00827454209456518,-0.245314910166111,
-0.230303445080417));
#50920=CARTESIAN_POINT('Ctrl Pts',(0.0894531799941032,-0.242576731246538,
-0.226063687473421));
#50921=CARTESIAN_POINT('Ctrl Pts',(0.169137773721435,-0.195544761529366,
-0.221823929866426));
#50922=CARTESIAN_POINT('Ctrl Pts',(0.210766588624511,-0.125798716970005,
-0.217584172259431));
#50923=CARTESIAN_POINT('Ctrl Pts',(0.252395403527586,-0.0560526724106442,
-0.213344414652435));
#50924=CARTESIAN_POINT('Ctrl Pts',(0.255968439606403,0.0364074469909048,
-0.20910465704544));
#50925=CARTESIAN_POINT('Ctrl Pts',(0.219846268834206,0.109158104554032,
-0.204864899438444));
#50926=CARTESIAN_POINT('Ctrl Pts',(0.183724098062009,0.181908762117159,
-0.200625141831449));
#50927=CARTESIAN_POINT('Ctrl Pts',(0.107906720438797,0.234949957841866,
-0.196385384224454));
#50928=CARTESIAN_POINT('Ctrl Pts',(0.0271814956909134,0.243944749294114,
-0.192145626617459));
#50929=CARTESIAN_POINT('Ctrl Pts',(-0.0535437290569703,0.252939540746362,
-0.187905869010463));
#50930=CARTESIAN_POINT('Ctrl Pts',(-0.139176800929527,0.217887927926151,
-0.183666111403468));
#50931=CARTESIAN_POINT('Ctrl Pts',(-0.19042666968436,0.154872691210361,
-0.179426353796473));
#50932=CARTESIAN_POINT('Ctrl Pts',(-0.225455879235849,0.111801870045655,
-0.17652848573805));
#50933=CARTESIAN_POINT('Ctrl Pts',(-0.244422279888803,0.0556672762822381,
-0.173630617679628));
#50934=CARTESIAN_POINT('Ctrl Pts',(-0.244854727503173,-0.000201854228764521,
-0.170732749621206));
#50935=CARTESIAN_POINT('Origin',(0.,0.,-0.775));
#50936=CARTESIAN_POINT('',(-0.245435813781494,-6.93175206961383E-5,-0.0791672503787938));
#50937=CARTESIAN_POINT('',(-0.24544712988196,-4.00287140078511E-5,-0.0907327496212059));
#50938=CARTESIAN_POINT('',(-0.24505,-3.00099698131059E-17,-0.775));
#50939=CARTESIAN_POINT('Ctrl Pts',(-0.245435813781494,-6.93175206961383E-5,
-0.0791672503787938));
#50940=CARTESIAN_POINT('Ctrl Pts',(-0.245137074140361,0.0772146059016804,
-0.0832000458945011));
#50941=CARTESIAN_POINT('Ctrl Pts',(-0.205588735409901,0.154757573364138,
-0.0872328414102084));
#50942=CARTESIAN_POINT('Ctrl Pts',(-0.142732132519899,0.199683998895668,
-0.0912656369259157));
#50943=CARTESIAN_POINT('Ctrl Pts',(-0.0766497439597067,0.246916037728415,
-0.095505394532911));
#50944=CARTESIAN_POINT('Ctrl Pts',(0.0151946451133084,0.258097885770481,
-0.0997451521399064));
#50945=CARTESIAN_POINT('Ctrl Pts',(0.0906723482987466,0.22809311535553,
-0.103984909746902));
#50946=CARTESIAN_POINT('Ctrl Pts',(0.166150051484185,0.198088344940579,
-0.108224667353897));
#50947=CARTESIAN_POINT('Ctrl Pts',(0.225261068782046,0.126896956068611,
-0.112464424960892));
#50948=CARTESIAN_POINT('Ctrl Pts',(0.240876975049947,0.0471868152081749,
-0.116704182567888));
#50949=CARTESIAN_POINT('Ctrl Pts',(0.256492881317849,-0.0325233256522602,
-0.120943940174883));
#50950=CARTESIAN_POINT('Ctrl Pts',(0.228613676555791,-0.120752218501163,
-0.125183697781878));
#50951=CARTESIAN_POINT('Ctrl Pts',(0.170034593344665,-0.17701934772879,
-0.129423455388874));
#50952=CARTESIAN_POINT('Ctrl Pts',(0.111455510133537,-0.233286476956419,
-0.133663212995869));
#50953=CARTESIAN_POINT('Ctrl Pts',(0.0221765484733384,-0.25759184256277,
-0.137902970602864));
#50954=CARTESIAN_POINT('Ctrl Pts',(-0.0568401436653837,-0.238782550966523,
-0.14214272820986));
#50955=CARTESIAN_POINT('Ctrl Pts',(-0.135856835804105,-0.219973259370277,
-0.146382485816855));
#50956=CARTESIAN_POINT('Ctrl Pts',(-0.20461125842135,-0.158049310571434,
-0.15062224342385));
#50957=CARTESIAN_POINT('Ctrl Pts',(-0.231555835121315,-0.0814237580450181,
-0.154862001030846));
#50958=CARTESIAN_POINT('Ctrl Pts',(-0.240676098748089,-0.0554873609967367,
-0.156297084146828));
#50959=CARTESIAN_POINT('Ctrl Pts',(-0.245006195747533,-0.0278665967856731,
-0.157732167262811));
#50960=CARTESIAN_POINT('Ctrl Pts',(-0.244810649818844,-0.000186483096579593,
-0.159167250378794));
#50961=CARTESIAN_POINT('Ctrl Pts',(-0.244854727503173,-0.000201854228764521,
-0.170732749621206));
#50962=CARTESIAN_POINT('Ctrl Pts',(-0.245054977108168,-0.0260726671191914,
-0.169390860072633));
#50963=CARTESIAN_POINT('Ctrl Pts',(-0.241281075540797,-0.0518865579329514,
-0.16804897052406));
#50964=CARTESIAN_POINT('Ctrl Pts',(-0.233287657827869,-0.0763200394868092,
-0.166707080975487));
#50965=CARTESIAN_POINT('Ctrl Pts',(-0.208032111579436,-0.15351867285682,
-0.162467323368491));
#50966=CARTESIAN_POINT('Ctrl Pts',(-0.140654353445459,-0.216937078985472,
-0.158227565761496));
#50967=CARTESIAN_POINT('Ctrl Pts',(-0.0620694914948961,-0.237476859134449,
-0.153987808154501));
#50968=CARTESIAN_POINT('Ctrl Pts',(0.0165153704556672,-0.258016639283427,
-0.149748050547505));
#50969=CARTESIAN_POINT('Ctrl Pts',(0.106307336222817,-0.235677793452729,
-0.14550829294051));
#50970=CARTESIAN_POINT('Ctrl Pts',(0.166107327439438,-0.180710233822531,
-0.141268535333515));
#50971=CARTESIAN_POINT('Ctrl Pts',(0.225907318656059,-0.125742674192334,
-0.137028777726519));
#50972=CARTESIAN_POINT('Ctrl Pts',(0.25571533532215,-0.038146400762637,
-0.132789020119524));
#50973=CARTESIAN_POINT('Ctrl Pts',(0.241854097822414,0.0418870367285358,
-0.128549262512529));
#50974=CARTESIAN_POINT('Ctrl Pts',(0.227992860322678,0.121920474219708,
-0.124309504905533));
#50975=CARTESIAN_POINT('Ctrl Pts',(0.170462368657113,0.194391075772358,
-0.120069747298538));
#50976=CARTESIAN_POINT('Ctrl Pts',(0.0956602294151765,0.226046509466257,
-0.115829989691543));
#50977=CARTESIAN_POINT('Ctrl Pts',(0.0208580901732384,0.257701943160157,
-0.111590232084547));
#50978=CARTESIAN_POINT('Ctrl Pts',(-0.0712156966450689,0.248542208995308,
-0.107350474477552));
#50979=CARTESIAN_POINT('Ctrl Pts',(-0.138316468287019,0.202771205622553,
-0.103110716870557));
#50980=CARTESIAN_POINT('Ctrl Pts',(-0.2036166757344,0.158228409136335,-0.0989847277874397));
#50981=CARTESIAN_POINT('Ctrl Pts',(-0.245266124651116,0.0790128155760584,
-0.0948587387043228));
#50982=CARTESIAN_POINT('Ctrl Pts',(-0.24544712988196,-4.00287140078511E-5,
-0.0907327496212059));
#50983=CARTESIAN_POINT('Origin',(0.,0.,-1.69285451186048));
#50984=CARTESIAN_POINT('',(-0.19978905918818,-5.64256782074264E-5,-0.052854511860476));
#50985=CARTESIAN_POINT('',(-0.199405777330601,0.000173947029632089,-0.0370454881395214));
#50986=CARTESIAN_POINT('',(-0.199475,-2.40257419738789E-14,-1.69285451186048));
#50987=CARTESIAN_POINT('',(0.197117919843508,-0.0326679626569813,-0.0149499999999996));
#50988=CARTESIAN_POINT('Ctrl Pts',(-0.19978905918818,-5.64256782074292E-5,
-0.0528545118604759));
#50989=CARTESIAN_POINT('Ctrl Pts',(-0.199801539091601,-0.0032849757852362,
-0.0526475497691882));
#50990=CARTESIAN_POINT('Ctrl Pts',(-0.198261725162247,-0.0726406134626104,
-0.0482008300709051));
#50991=CARTESIAN_POINT('Ctrl Pts',(-0.117789880017489,-0.204361235882386,
-0.0395143527656268));
#50992=CARTESIAN_POINT('Ctrl Pts',(0.102816622150766,-0.209511115609609,
-0.0270864775700892));
#50993=CARTESIAN_POINT('Ctrl Pts',(0.186733138685136,-0.0934018186338016,
-0.0188983599815467));
#50994=CARTESIAN_POINT('Ctrl Pts',(0.197120359334095,-0.0326678654691807,
-0.0149499999999996));
#50995=CARTESIAN_POINT('',(0.0326814423280684,-0.196779569448551,-0.01495));
#50996=CARTESIAN_POINT('Origin',(0.,0.,-0.0149499999999998));
#50997=CARTESIAN_POINT('Ctrl Pts',(-0.199405777330601,0.000173947029632086,
-0.0370454881395214));
#50998=CARTESIAN_POINT('Ctrl Pts',(-0.198920212120655,-0.0488485699620836,
-0.0339200830333429));
#50999=CARTESIAN_POINT('Ctrl Pts',(-0.155869131157208,-0.165069700487324,
-0.0265549203201691));
#51000=CARTESIAN_POINT('Ctrl Pts',(-0.0328441439546209,-0.207662155862942,
-0.0191897576069953));
#51001=CARTESIAN_POINT('Ctrl Pts',(0.0326814423280684,-0.196779569448551,
-0.01495));
#51002=CARTESIAN_POINT('Origin',(0.,0.,-1.69285451186048));
#51003=CARTESIAN_POINT('',(-0.199280164752556,-0.000151800512929585,-0.132854511860476));
#51004=CARTESIAN_POINT('',(-0.199798270692528,-3.2584075625286E-5,-0.117045488139522));
#51005=CARTESIAN_POINT('',(-0.199475,-2.40257419738789E-14,-1.69285451186048));
#51006=CARTESIAN_POINT('Ctrl Pts',(-0.199280164752556,-0.000151800512929595,
-0.132854511860476));
#51007=CARTESIAN_POINT('Ctrl Pts',(-0.199439342569838,-0.0226838987709636,
-0.131419428744494));
#51008=CARTESIAN_POINT('Ctrl Pts',(-0.185501100147388,-0.111592971135028,
-0.125744588021516));
#51009=CARTESIAN_POINT('Ctrl Pts',(-0.0546225418096208,-0.229469274023813,
-0.115829989691543));
#51010=CARTESIAN_POINT('Ctrl Pts',(0.16340138241606,-0.170114291722319,
-0.103110716870557));
#51011=CARTESIAN_POINT('Ctrl Pts',(0.231483868070962,0.0453453091881316,
-0.0903914440495704));
#51012=CARTESIAN_POINT('Ctrl Pts',(0.0871316520886174,0.219198428493199,
-0.0776721712285846));
#51013=CARTESIAN_POINT('Ctrl Pts',(-0.133507657360752,0.192336088231908,
-0.0651598604988864));
#51014=CARTESIAN_POINT('Ctrl Pts',(-0.199545879878187,0.0628540441225657,
-0.0568873073761835));
#51015=CARTESIAN_POINT('Ctrl Pts',(-0.19978905918818,-5.64256782074292E-5,
-0.0528545118604759));
#51016=CARTESIAN_POINT('Ctrl Pts',(-0.199798270692528,-3.25840756252845E-5,
-0.117045488139522));
#51017=CARTESIAN_POINT('Ctrl Pts',(-0.199802333431698,-0.00180695869165221,
-0.116931719615644));
#51018=CARTESIAN_POINT('Ctrl Pts',(-0.198975693736128,-0.0697022559227335,
-0.112578193484771));
#51019=CARTESIAN_POINT('Ctrl Pts',(-0.122283640616722,-0.201709157150624,
-0.103984909746902));
#51020=CARTESIAN_POINT('Ctrl Pts',(0.10342756844873,-0.21198412740384,-0.091265636925916));
#51021=CARTESIAN_POINT('Ctrl Pts',(0.234263184552909,-0.0277545195405686,
-0.0785463641049296));
#51022=CARTESIAN_POINT('Ctrl Pts',(0.150056069810251,0.181992167351128,
-0.0658270912839439));
#51023=CARTESIAN_POINT('Ctrl Pts',(-0.0717210418700825,0.224640263091484,
-0.0531078184629578));
#51024=CARTESIAN_POINT('Ctrl Pts',(-0.189548818024464,0.101452165564304,
-0.0435139507481504));
#51025=CARTESIAN_POINT('Ctrl Pts',(-0.199578903945434,0.0176527577918152,
-0.0381598406403383));
#51026=CARTESIAN_POINT('Ctrl Pts',(-0.199405777330601,0.000173947029632086,
-0.0370454881395214));
#51027=CARTESIAN_POINT('Origin',(0.,0.,-1.69285451186048));
#51028=CARTESIAN_POINT('',(-0.199232182693492,0.000127961726227482,-0.212854511860476));
#51029=CARTESIAN_POINT('',(-0.19931604476105,-0.000164312884269185,-0.197045488139522));
#51030=CARTESIAN_POINT('',(-0.199475,-2.40257419738789E-14,-1.69285451186048));
#51031=CARTESIAN_POINT('Ctrl Pts',(-0.199232182693492,0.000127961726227475,
-0.212854511860476));
#51032=CARTESIAN_POINT('Ctrl Pts',(-0.198987070943203,-0.0417119960123555,
-0.210191307719799));
#51033=CARTESIAN_POINT('Ctrl Pts',(-0.165649967516347,-0.15051751299201,
-0.203288345972126));
#51034=CARTESIAN_POINT('Ctrl Pts',(0.0131260578517699,-0.235515155392752,
-0.192145626617459));
#51035=CARTESIAN_POINT('Ctrl Pts',(0.205151283752445,-0.116415679756492,
-0.179426353796472));
#51036=CARTESIAN_POINT('Ctrl Pts',(0.208917206173459,0.109513919792018,
-0.166707080975487));
#51037=CARTESIAN_POINT('Ctrl Pts',(0.0209676371933062,0.234946925588856,
-0.1539878081545));
#51038=CARTESIAN_POINT('Ctrl Pts',(-0.162845934874777,0.154951522837623,
-0.142703618449497));
#51039=CARTESIAN_POINT('Ctrl Pts',(-0.198969073388792,0.0438841166471984,
-0.135659186351489));
#51040=CARTESIAN_POINT('Ctrl Pts',(-0.199280164752556,-0.000151800512929595,
-0.132854511860476));
#51041=CARTESIAN_POINT('Ctrl Pts',(-0.19931604476105,-0.000164312884269184,
-0.197045488139521));
#51042=CARTESIAN_POINT('Ctrl Pts',(-0.199479051453381,-0.0212236085435869,
-0.195703598590949));
#51043=CARTESIAN_POINT('Ctrl Pts',(-0.186700843720701,-0.10862791766991,
-0.190121951435381));
#51044=CARTESIAN_POINT('Ctrl Pts',(-0.0596484344001499,-0.228214284403755,
-0.180300546672818));
#51045=CARTESIAN_POINT('Ctrl Pts',(0.159628272860435,-0.173661646916563,
-0.167581273851832));
#51046=CARTESIAN_POINT('Ctrl Pts',(0.232421018722115,0.0402530640696309,
-0.154862001030846));
#51047=CARTESIAN_POINT('Ctrl Pts',(0.0919285295363725,0.217230088081641,
-0.14214272820986));
#51048=CARTESIAN_POINT('Ctrl Pts',(-0.130909325195414,0.195061612321686,
-0.129537223912752));
#51049=CARTESIAN_POINT('Ctrl Pts',(-0.19965092925845,0.0643178183514808,
-0.121171477222639));
#51050=CARTESIAN_POINT('Ctrl Pts',(-0.199798270692528,-3.25840756252845E-5,
-0.117045488139522));
#51051=CARTESIAN_POINT('Origin',(0.,0.,-1.69285451186048));
#51052=CARTESIAN_POINT('',(-0.199747309326353,9.62307426035103E-5,-0.292854511860476));
#51053=CARTESIAN_POINT('',(-0.199205763221826,0.000109377304542274,-0.277045488139522));
#51054=CARTESIAN_POINT('',(-0.199475,-2.40257419738789E-14,-1.69285451186048));
#51055=CARTESIAN_POINT('Ctrl Pts',(-0.199747309326353,9.62307426035014E-5,
-0.292854511860476));
#51056=CARTESIAN_POINT('Ctrl Pts',(-0.199386580426527,-0.0606345073915193,
-0.288963186695104));
#51057=CARTESIAN_POINT('Ctrl Pts',(-0.137371276050314,-0.188171277532572,
-0.280832103922736));
#51058=CARTESIAN_POINT('Ctrl Pts',(0.0797840202277238,-0.221977898961698,
-0.268461263543375));
#51059=CARTESIAN_POINT('Ctrl Pts',(0.229840910738551,-0.0530361458245903,
-0.255741990722388));
#51060=CARTESIAN_POINT('Ctrl Pts',(0.168981662475758,0.164574832115758,
-0.243022717901402));
#51061=CARTESIAN_POINT('Ctrl Pts',(-0.0469455463466026,0.231161834775108,
-0.230303445080416));
#51062=CARTESIAN_POINT('Ctrl Pts',(-0.18360132481013,0.116094458771798,
-0.220247376400108));
#51063=CARTESIAN_POINT('Ctrl Pts',(-0.199377283015938,0.024896220905409,
-0.214431065326794));
#51064=CARTESIAN_POINT('Ctrl Pts',(-0.199232182693492,0.000127961726227475,
-0.212854511860476));
#51065=CARTESIAN_POINT('Ctrl Pts',(-0.199205763221826,0.000109377304542285,
-0.277045488139522));
#51066=CARTESIAN_POINT('Ctrl Pts',(-0.199005192472171,-0.0402798854940347,
-0.274475477566255));
#51067=CARTESIAN_POINT('Ctrl Pts',(-0.167435605774816,-0.147587685310038,
-0.267665709385992));
#51068=CARTESIAN_POINT('Ctrl Pts',(0.00795180063483016,-0.23574656447556,
-0.256616183598734));
#51069=CARTESIAN_POINT('Ctrl Pts',(0.202545773298689,-0.12089201855432,
-0.243896910777748));
#51070=CARTESIAN_POINT('Ctrl Pts',(0.211271315496057,0.10490046033926,-0.231177637956761));
#51071=CARTESIAN_POINT('Ctrl Pts',(0.0261212881376767,0.234429852510476,
-0.218458365135776));
#51072=CARTESIAN_POINT('Ctrl Pts',(-0.160936868752923,0.157862587704772,
-0.207080981863362));
#51073=CARTESIAN_POINT('Ctrl Pts',(-0.198964024814612,0.0453141397118719,
-0.199943356197944));
#51074=CARTESIAN_POINT('Ctrl Pts',(-0.19931604476105,-0.000164312884269184,
-0.197045488139521));
#51075=CARTESIAN_POINT('Origin',(0.,0.,-1.69285451186048));
#51076=CARTESIAN_POINT('',(-0.19952645684413,-0.000179680236322701,-0.372854511860476));
#51077=CARTESIAN_POINT('',(-0.199716645377052,0.000117807287515384,-0.357045488139522));
#51078=CARTESIAN_POINT('',(-0.199475,-2.40257419738789E-14,-1.69285451186048));
#51079=CARTESIAN_POINT('Ctrl Pts',(-0.19952645684413,-0.000179680236322737,
-0.372854511860476));
#51080=CARTESIAN_POINT('Ctrl Pts',(-0.19965407975718,-0.0139482848893583,
-0.371974823277405));
#51081=CARTESIAN_POINT('Ctrl Pts',(-0.192069331498236,-0.0939365192239043,
-0.366855377087338));
#51082=CARTESIAN_POINT('Ctrl Pts',(-0.0840994204847348,-0.220379138866998,
-0.357496173290276));
#51083=CARTESIAN_POINT('Ctrl Pts',(0.139807809013192,-0.189982772682906,
-0.344776900469291));
#51084=CARTESIAN_POINT('Ctrl Pts',(0.235418803056905,0.014753458384602,
-0.332057627648304));
#51085=CARTESIAN_POINT('Ctrl Pts',(0.11499503919352,0.205951009552392,-0.319338354827319));
#51086=CARTESIAN_POINT('Ctrl Pts',(-0.110955238097539,0.208155260646928,
-0.306619082006331));
#51087=CARTESIAN_POINT('Ctrl Pts',(-0.19710964318935,0.0771084030278873,
-0.297791134350718));
#51088=CARTESIAN_POINT('Ctrl Pts',(-0.199779609287417,0.00553411076300435,
-0.2932029443021));
#51089=CARTESIAN_POINT('Ctrl Pts',(-0.199747309326353,9.62307426035014E-5,
-0.292854511860476));
#51090=CARTESIAN_POINT('Ctrl Pts',(-0.199716645377052,0.000117807287515386,
-0.357045488139522));
#51091=CARTESIAN_POINT('Ctrl Pts',(-0.199301888682071,-0.0591824740362239,
-0.353247356541559));
#51092=CARTESIAN_POINT('Ctrl Pts',(-0.139839812362773,-0.185400255066588,
-0.345209467336602));
#51093=CARTESIAN_POINT('Ctrl Pts',(0.0748909360789789,-0.223676151397489,
-0.332931820524649));
#51094=CARTESIAN_POINT('Ctrl Pts',(0.228621008521177,-0.0580698493273639,
-0.320212547703664));
#51095=CARTESIAN_POINT('Ctrl Pts',(0.172554397257742,0.160824914104033,
-0.307493274882677));
#51096=CARTESIAN_POINT('Ctrl Pts',(-0.0418587313987176,0.232136855608358,
-0.294774002061692));
#51097=CARTESIAN_POINT('Ctrl Pts',(-0.182297588611502,0.119059390862335,
-0.284624739813973));
#51098=CARTESIAN_POINT('Ctrl Pts',(-0.199336074909168,0.0263504567980952,
-0.27871523517325));
#51099=CARTESIAN_POINT('Ctrl Pts',(-0.199205763221826,0.000109377304542285,
-0.277045488139522));
#51100=CARTESIAN_POINT('Origin',(0.,0.,-1.69285451186048));
#51101=CARTESIAN_POINT('',(-0.199145764441746,-3.13449387460375E-6,-0.452854511860477));
#51102=CARTESIAN_POINT('',(-0.199570626225687,-0.000172606811285253,-0.437045488139522));
#51103=CARTESIAN_POINT('',(-0.199475,-2.40257419738789E-14,-1.69285451186048));
#51104=CARTESIAN_POINT('Ctrl Pts',(-0.199145793344766,-3.13421870281119E-6,
-0.452854511860477));
#51105=CARTESIAN_POINT('Ctrl Pts',(-0.199150426498933,-0.0331535588910306,
-0.450746702252711));
#51106=CARTESIAN_POINT('Ctrl Pts',(-0.175592596745264,-0.132978274684061,
-0.444399135037949));
#51107=CARTESIAN_POINT('Ctrl Pts',(-0.0177182263414914,-0.235214246654171,
-0.433811810216192));
#51108=CARTESIAN_POINT('Ctrl Pts',(0.188206317046981,-0.142190223283767,
-0.421092537395206));
#51109=CARTESIAN_POINT('Ctrl Pts',(0.221421180402404,0.081316285225576,
-0.40837326457422));
#51110=CARTESIAN_POINT('Ctrl Pts',(0.051446364370158,0.230201974289577,
-0.395653991753234));
#51111=CARTESIAN_POINT('Ctrl Pts',(-0.150717866526423,0.17215324521349,
-0.383814407515319));
#51112=CARTESIAN_POINT('Ctrl Pts',(-0.19903898684039,0.0524110466272596,
-0.3762145808844));
#51113=CARTESIAN_POINT('Ctrl Pts',(-0.19952645684413,-0.000179680236322737,
-0.372854511860476));
#51114=CARTESIAN_POINT('Ctrl Pts',(-0.199570626225687,-0.000172606811285283,
-0.437045488139522));
#51115=CARTESIAN_POINT('Ctrl Pts',(-0.199682928323807,-0.0124755616086236,
-0.43625899312386));
#51116=CARTESIAN_POINT('Ctrl Pts',(-0.193038335109565,-0.0909790538091767,
-0.431232740501203));
#51117=CARTESIAN_POINT('Ctrl Pts',(-0.0889178870534499,-0.21847947809828,
-0.421966730271551));
#51118=CARTESIAN_POINT('Ctrl Pts',(0.135602752200584,-0.193006649067832,
-0.409247457450565));
#51119=CARTESIAN_POINT('Ctrl Pts',(0.235685974516513,0.00958093959523976,
-0.396528184629579));
#51120=CARTESIAN_POINT('Ctrl Pts',(0.119489265933811,0.20337646942222,-0.383808911808593));
#51121=CARTESIAN_POINT('Ctrl Pts',(-0.106358134575664,0.210541255342925,
-0.371089638987607));
#51122=CARTESIAN_POINT('Ctrl Pts',(-0.196308748593597,0.0800545266610567,
-0.362168497764583));
#51123=CARTESIAN_POINT('Ctrl Pts',(-0.199764871021477,0.00701292029244546,
-0.357487114148555));
#51124=CARTESIAN_POINT('Ctrl Pts',(-0.199716645377052,0.000117807287515386,
-0.357045488139522));
#51125=CARTESIAN_POINT('Origin',(0.,0.,-1.69285451186048));
#51126=CARTESIAN_POINT('',(-0.199514918438111,0.000180945765229524,-0.532854511860476));
#51127=CARTESIAN_POINT('',(-0.1991491027263,-2.72391900677377E-5,-0.517045488139522));
#51128=CARTESIAN_POINT('',(-0.199475,-2.40257419738789E-14,-1.69285451186048));
#51129=CARTESIAN_POINT('Ctrl Pts',(-0.199514918438111,0.000180945765229527,
-0.532854511860476));
#51130=CARTESIAN_POINT('Ctrl Pts',(-0.199030404431233,-0.0520397267160747,
-0.529518581228016));
#51131=CARTESIAN_POINT('Ctrl Pts',(-0.15128305072811,-0.171413952745693,
-0.521942892988561));
#51132=CARTESIAN_POINT('Ctrl Pts',(0.0501362714953425,-0.230490849393937,
-0.510127447142107));
#51133=CARTESIAN_POINT('Ctrl Pts',(0.220955117411352,-0.0825742905723761,
-0.497408174321123));
#51134=CARTESIAN_POINT('Ctrl Pts',(0.189011971974381,0.141117510692855,
-0.484688901500136));
#51135=CARTESIAN_POINT('Ctrl Pts',(-0.0163801719563586,0.235311213800938,
-0.47196962867915));
#51136=CARTESIAN_POINT('Ctrl Pts',(-0.175194713167085,0.133743756730128,
-0.46135816546593));
#51137=CARTESIAN_POINT('Ctrl Pts',(-0.199141107132255,0.0335269252768801,
-0.454986459859706));
#51138=CARTESIAN_POINT('Ctrl Pts',(-0.199145793344766,-3.13421870281119E-6,
-0.452854511860477));
#51139=CARTESIAN_POINT('Ctrl Pts',(-0.1991491027263,-2.72391900677377E-5,
-0.517045488139522));
#51140=CARTESIAN_POINT('Ctrl Pts',(-0.19918762421967,-0.0317106516158013,
-0.515030872099166));
#51141=CARTESIAN_POINT('Ctrl Pts',(-0.177100415645962,-0.130021035991661,
-0.508776498451814));
#51142=CARTESIAN_POINT('Ctrl Pts',(-0.0228784244999453,-0.234768504447706,
-0.498282367197467));
#51143=CARTESIAN_POINT('Ctrl Pts',(0.185038945608821,-0.146288282497961,
-0.485563094376481));
#51144=CARTESIAN_POINT('Ctrl Pts',(0.223153210321907,0.0764350555126916,
-0.472843821555495));
#51145=CARTESIAN_POINT('Ctrl Pts',(0.0564883785752809,0.229016890368669,
-0.46012454873451));
#51146=CARTESIAN_POINT('Ctrl Pts',(-0.148502607420017,0.174999094124885,
-0.448191770929184));
#51147=CARTESIAN_POINT('Ctrl Pts',(-0.199077541556816,0.0538459600181255,
-0.440498750730856));
#51148=CARTESIAN_POINT('Ctrl Pts',(-0.199570626225687,-0.000172606811285283,
-0.437045488139522));
#51149=CARTESIAN_POINT('Origin',(0.,0.,-1.69285451186048));
#51150=CARTESIAN_POINT('',(-0.199754379428577,-9.02611387494427E-5,-0.612854511860476));
#51151=CARTESIAN_POINT('',(-0.199470369800604,0.000183637767226734,-0.597045488139522));
#51152=CARTESIAN_POINT('',(-0.199475,-2.40257419738789E-14,-1.69285451186048));
#51153=CARTESIAN_POINT('Ctrl Pts',(-0.199754379428577,-9.02611387494983E-5,
-0.612854511860476));
#51154=CARTESIAN_POINT('Ctrl Pts',(-0.199782877503472,-0.00515094661274952,
-0.612530217810316));
#51155=CARTESIAN_POINT('Ctrl Pts',(-0.197311473429714,-0.0763457633342411,
-0.60796616615316));
#51156=CARTESIAN_POINT('Ctrl Pts',(-0.112137314847476,-0.207520842308891,
-0.599162356889011));
#51157=CARTESIAN_POINT('Ctrl Pts',(0.113821844477603,-0.206601706414806,
-0.586443084068023));
#51158=CARTESIAN_POINT('Ctrl Pts',(0.235331086026933,-0.0160921509804536,
-0.573723811247038));
#51159=CARTESIAN_POINT('Ctrl Pts',(0.140886064153414,0.189184550905072,
-0.561004538426052));
#51160=CARTESIAN_POINT('Ctrl Pts',(-0.0828446663124362,0.22085388526665,
-0.548285265605067));
#51161=CARTESIAN_POINT('Ctrl Pts',(-0.191812282577816,0.0947028634056557,
-0.53890192341654));
#51162=CARTESIAN_POINT('Ctrl Pts',(-0.199646191200409,0.0143294571154524,
-0.533758338835011));
#51163=CARTESIAN_POINT('Ctrl Pts',(-0.199514918438111,0.000180945765229527,
-0.532854511860476));
#51164=CARTESIAN_POINT('Ctrl Pts',(-0.199470369800604,0.000183637767226717,
-0.597045488139522));
#51165=CARTESIAN_POINT('Ctrl Pts',(-0.199002463741088,-0.0506072066419029,
-0.593802751074471));
#51166=CARTESIAN_POINT('Ctrl Pts',(-0.15343214889695,-0.168551718593714,
-0.586320256402424));
#51167=CARTESIAN_POINT('Ctrl Pts',(0.0450634218898312,-0.231536090050329,
-0.574598004123383));
#51168=CARTESIAN_POINT('Ctrl Pts',(0.219088804207135,-0.0874057713157602,
-0.561878731302397));
#51169=CARTESIAN_POINT('Ctrl Pts',(0.192064838835073,0.136933453441709,
-0.54915945848141));
#51170=CARTESIAN_POINT('Ctrl Pts',(-0.0112096232321388,0.235614128046703,
-0.536440185660426));
#51171=CARTESIAN_POINT('Ctrl Pts',(-0.173629946925928,0.136697002188027,
-0.525735528879795));
#51172=CARTESIAN_POINT('Ctrl Pts',(-0.199106555772246,0.0349670607406491,
-0.519270629706161));
#51173=CARTESIAN_POINT('Ctrl Pts',(-0.1991491027263,-2.72391900677377E-5,
-0.517045488139522));
#51174=CARTESIAN_POINT('Origin',(0.,0.,-1.69285451186048));
#51175=CARTESIAN_POINT('',(-0.199239712079179,-0.000132428612020959,-0.692854511860477));
#51176=CARTESIAN_POINT('',(-0.199777832380642,-6.59547829733875E-5,-0.677045488139522));
#51177=CARTESIAN_POINT('',(-0.199475,-2.40257419738789E-14,-1.69285451186048));
#51178=CARTESIAN_POINT('Ctrl Pts',(-0.199239712079179,-0.000132428612020962,
-0.692854511860477));
#51179=CARTESIAN_POINT('Ctrl Pts',(-0.199387925235899,-0.0245191527044881,
-0.691302096785622));
#51180=CARTESIAN_POINT('Ctrl Pts',(-0.183932189689554,-0.11532642708485,
-0.685509924103772));
#51181=CARTESIAN_POINT('Ctrl Pts',(-0.0482595044417223,-0.23089109468499,
-0.675477993814925));
#51182=CARTESIAN_POINT('Ctrl Pts',(0.168042917961313,-0.165533244687709,
-0.662758720993941));
#51183=CARTESIAN_POINT('Ctrl Pts',(0.230138834184335,0.0517280810978802,
-0.650039448172953));
#51184=CARTESIAN_POINT('Ctrl Pts',(0.0810452162903746,0.221520541463405,
-0.637320175351968));
#51185=CARTESIAN_POINT('Ctrl Pts',(-0.136722929391739,0.188885971979512,
-0.624925196581142));
#51186=CARTESIAN_POINT('Ctrl Pts',(-0.199410299191403,0.0610114751905463,
-0.616769975417311));
#51187=CARTESIAN_POINT('Ctrl Pts',(-0.199754379428577,-9.02611387494983E-5,
-0.612854511860476));
#51188=CARTESIAN_POINT('Ctrl Pts',(-0.199777832380642,-6.59547829734257E-5,
-0.677045488139522));
#51189=CARTESIAN_POINT('Ctrl Pts',(-0.199793333714704,-0.0036712079644515,
-0.676814387656772));
#51190=CARTESIAN_POINT('Ctrl Pts',(-0.198069267605619,-0.0734031236255173,
-0.672343529567026));
#51191=CARTESIAN_POINT('Ctrl Pts',(-0.116666698598652,-0.205008669149152,
-0.663632913870284));
#51192=CARTESIAN_POINT('Ctrl Pts',(0.109258160368663,-0.209051016216307,
-0.650913641049299));
#51193=CARTESIAN_POINT('Ctrl Pts',(0.234921018494109,-0.0212553065822581,
-0.638194368228312));
#51194=CARTESIAN_POINT('Ctrl Pts',(0.145005916359623,0.186045578310588,
-0.625475095407328));
#51195=CARTESIAN_POINT('Ctrl Pts',(-0.0779755238778273,0.222619609792564,
-0.612755822586341));
#51196=CARTESIAN_POINT('Ctrl Pts',(-0.19079618970027,0.0976627030116315,
-0.603279286830406));
#51197=CARTESIAN_POINT('Ctrl Pts',(-0.199614233439153,0.015799925552125,
-0.598042508681467));
#51198=CARTESIAN_POINT('Ctrl Pts',(-0.199470369800604,0.000183637767226717,
-0.597045488139522));
#51199=CARTESIAN_POINT('Origin',(0.,0.,-1.69285451186048));
#51200=CARTESIAN_POINT('',(-0.199271260405861,0.000148188788378376,-0.772854511860477));
#51201=CARTESIAN_POINT('',(-0.199271252552475,-0.00014818878255532,-0.757045488139522));
#51202=CARTESIAN_POINT('',(-0.199475,-2.40257419738789E-14,-1.69285451186048));
#51203=CARTESIAN_POINT('Ctrl Pts',(-0.199271260405861,0.000148188788378367,
-0.772854511860477));
#51204=CARTESIAN_POINT('Ctrl Pts',(-0.198971206859014,-0.0435135905361769,
-0.770073975760927));
#51205=CARTESIAN_POINT('Ctrl Pts',(-0.163332551127985,-0.154196284756057,
-0.763053682054382));
#51206=CARTESIAN_POINT('Ctrl Pts',(0.0196311741237908,-0.235062320196826,
-0.751793630740842));
#51207=CARTESIAN_POINT('Ctrl Pts',(0.208290908157902,-0.110700383705523,
-0.739074357919856));
#51208=CARTESIAN_POINT('Ctrl Pts',(0.205810107346701,0.115247026372627,
-0.726355085098869));
#51209=CARTESIAN_POINT('Ctrl Pts',(0.0144653069364513,0.235436684204114,
-0.713635812277884));
#51210=CARTESIAN_POINT('Ctrl Pts',(-0.16517954457325,0.151275282131266,
-0.702468954531752));
#51211=CARTESIAN_POINT('Ctrl Pts',(-0.198983144408374,0.0420827507783096,
-0.695541854392617));
#51212=CARTESIAN_POINT('Ctrl Pts',(-0.199239712079179,-0.000132428612020962,
-0.692854511860477));
#51213=CARTESIAN_POINT('Ctrl Pts',(-0.199271252552475,-0.000148188782555318,
-0.757045488139522));
#51214=CARTESIAN_POINT('Ctrl Pts',(-0.19942872023353,-0.0230618294085849,
-0.755586266632077));
#51215=CARTESIAN_POINT('Ctrl Pts',(-0.185183518334068,-0.112361096942695,
-0.749887287517637));
#51216=CARTESIAN_POINT('Ctrl Pts',(-0.0533174176740989,-0.229775816744889,
-0.739948550796201));
#51217=CARTESIAN_POINT('Ctrl Pts',(0.164367878228055,-0.169182958938016,
-0.727229277975214));
#51218=CARTESIAN_POINT('Ctrl Pts',(0.231219110206101,0.0466625766939018,
-0.714510005154229));
#51219=CARTESIAN_POINT('Ctrl Pts',(0.085889480416779,0.219687664974506,
-0.701790732333243));
#51220=CARTESIAN_POINT('Ctrl Pts',(-0.134185014399097,0.191633020719834,
-0.689302559995007));
#51221=CARTESIAN_POINT('Ctrl Pts',(-0.199508947034822,0.0624705820456586,
-0.681054145263767));
#51222=CARTESIAN_POINT('Ctrl Pts',(-0.199777832380642,-6.59547829734257E-5,
-0.677045488139522));
#51223=CARTESIAN_POINT('Origin',(0.,0.,-1.69285451186048));
#51224=CARTESIAN_POINT('',(-0.199777840253992,6.59547855500507E-5,-0.852854511860477));
#51225=CARTESIAN_POINT('',(-0.199239704227035,0.000132428606779117,-0.837045488139522));
#51226=CARTESIAN_POINT('',(-0.199475,-2.40257419738789E-14,-1.69285451186048));
#51227=CARTESIAN_POINT('Ctrl Pts',(-0.199777840253992,6.59547855500525E-5,
-0.852854511860478));
#51228=CARTESIAN_POINT('Ctrl Pts',(-0.199508954897568,-0.0624705845076746,
-0.848845854736233));
#51229=CARTESIAN_POINT('Ctrl Pts',(-0.134185019687388,-0.191633028272198,
-0.840597440004992));
#51230=CARTESIAN_POINT('Ctrl Pts',(0.0858894838017356,-0.219687673632512,
-0.828109267666759));
#51231=CARTESIAN_POINT('Ctrl Pts',(0.23121911931857,-0.0466625785328924,
-0.81538999484577));
#51232=CARTESIAN_POINT('Ctrl Pts',(0.164367884705876,0.169182965605612,
-0.802670722024787));
#51233=CARTESIAN_POINT('Ctrl Pts',(-0.0533174197753734,0.229775825800475,
-0.789951449203798));
#51234=CARTESIAN_POINT('Ctrl Pts',(-0.185183525632255,0.112361101370898,
-0.780012712482364));
#51235=CARTESIAN_POINT('Ctrl Pts',(-0.199428728093124,0.0230618303174506,
-0.774313733367923));
#51236=CARTESIAN_POINT('Ctrl Pts',(-0.199271260405861,0.000148188788378367,
-0.772854511860477));
#51237=CARTESIAN_POINT('Ctrl Pts',(-0.199239704227035,0.000132428606779098,
-0.837045488139522));
#51238=CARTESIAN_POINT('Ctrl Pts',(-0.198983136566337,-0.0420827491198241,
-0.834358145607383));
#51239=CARTESIAN_POINT('Ctrl Pts',(-0.165179538063425,-0.151275276169436,
-0.827431045468248));
#51240=CARTESIAN_POINT('Ctrl Pts',(0.0144653063663763,-0.235436674925429,
-0.816264187722117));
#51241=CARTESIAN_POINT('Ctrl Pts',(0.205810099235619,-0.115247021830672,
-0.80354491490113));
#51242=CARTESIAN_POINT('Ctrl Pts',(0.208290899949043,0.110700379342769,
-0.790825642080145));
#51243=CARTESIAN_POINT('Ctrl Pts',(0.019631173350109,0.235062310932895,
-0.778106369259159));
#51244=CARTESIAN_POINT('Ctrl Pts',(-0.16333254469097,0.154196278679093,
-0.766846317945618));
#51245=CARTESIAN_POINT('Ctrl Pts',(-0.198971199017457,0.0435135888212697,
-0.759826024239072));
#51246=CARTESIAN_POINT('Ctrl Pts',(-0.199271252552475,-0.000148188782555318,
-0.757045488139522));
#51247=CARTESIAN_POINT('Origin',(0.,0.,-1.69285451186048));
#51248=CARTESIAN_POINT('',(-0.199470377661838,-0.000183637774485374,-0.932854511860477));
#51249=CARTESIAN_POINT('',(-0.199754371556151,9.02611351696198E-5,-0.917045488139523));
#51250=CARTESIAN_POINT('',(-0.199475,-2.40257419738789E-14,-1.69285451186048));
#51251=CARTESIAN_POINT('Ctrl Pts',(-0.199470377661838,-0.000183637774485384,
-0.932854511860477));
#51252=CARTESIAN_POINT('Ctrl Pts',(-0.199614241306055,-0.0157999261748247,
-0.931857491318533));
#51253=CARTESIAN_POINT('Ctrl Pts',(-0.190796197219643,-0.0976627068605806,
-0.926620713169594));
#51254=CARTESIAN_POINT('Ctrl Pts',(-0.0779755269508779,-0.222619618566124,
-0.917144177413659));
#51255=CARTESIAN_POINT('Ctrl Pts',(0.145005922074389,-0.186045585642739,
-0.904424904592673));
#51256=CARTESIAN_POINT('Ctrl Pts',(0.234921027752471,0.0212553074199478,
-0.891705631771688));
#51257=CARTESIAN_POINT('Ctrl Pts',(0.109258164674579,0.209051024455123,
-0.878986358950702));
#51258=CARTESIAN_POINT('Ctrl Pts',(-0.116666703196555,0.20500867722865,
-0.866267086129715));
#51259=CARTESIAN_POINT('Ctrl Pts',(-0.19806927541164,0.0734031265183624,
-0.857556470432975));
#51260=CARTESIAN_POINT('Ctrl Pts',(-0.199793341588666,0.00367120810911873,
-0.853085612343228));
#51261=CARTESIAN_POINT('Ctrl Pts',(-0.199777840253992,6.59547855500525E-5,
-0.852854511860478));
#51262=CARTESIAN_POINT('Ctrl Pts',(-0.199754371556151,9.02611351696076E-5,
-0.917045488139523));
#51263=CARTESIAN_POINT('Ctrl Pts',(-0.19941029133253,-0.0610114727860687,
-0.913130024582688));
#51264=CARTESIAN_POINT('Ctrl Pts',(-0.136722924003404,-0.188885964535421,
-0.904974803418858));
#51265=CARTESIAN_POINT('Ctrl Pts',(0.0810452130963459,-0.22152053273316,
-0.892579824648032));
#51266=CARTESIAN_POINT('Ctrl Pts',(0.230138825114443,-0.0517280790592424,
-0.879860551827046));
#51267=CARTESIAN_POINT('Ctrl Pts',(0.168042911338648,0.165533238163961,
-0.86714127900606));
#51268=CARTESIAN_POINT('Ctrl Pts',(-0.0482595025397965,0.230891085585448,
-0.854422006185075));
#51269=CARTESIAN_POINT('Ctrl Pts',(-0.183932182440697,0.115326422539765,
-0.844390075896228));
#51270=CARTESIAN_POINT('Ctrl Pts',(-0.199387917377917,0.0245191517381582,
-0.838597903214378));
#51271=CARTESIAN_POINT('Ctrl Pts',(-0.199239704227035,0.000132428606779098,
-0.837045488139522));
#51272=CARTESIAN_POINT('Origin',(0.,0.,-1.69285451186048));
#51273=CARTESIAN_POINT('',(-0.199149110574872,2.7239191122689E-5,-1.01285451186048));
#51274=CARTESIAN_POINT('',(-0.199514910575122,-0.000180945758118223,-0.997045488139523));
#51275=CARTESIAN_POINT('',(-0.199475,-2.40257419738789E-14,-1.69285451186048));
#51276=CARTESIAN_POINT('Ctrl Pts',(-0.199149110574872,2.72391911226855E-5,
-1.01285451186048));
#51277=CARTESIAN_POINT('Ctrl Pts',(-0.199106563619138,-0.0349670621187339,
-1.01062937029384));
#51278=CARTESIAN_POINT('Ctrl Pts',(-0.173629953768769,-0.136697007575336,
-1.0041644711202));
#51279=CARTESIAN_POINT('Ctrl Pts',(-0.011209623673909,-0.235614137332382,
-0.993459814339576));
#51280=CARTESIAN_POINT('Ctrl Pts',(0.192064846404454,-0.136933458838324,
-0.980740541518589));
#51281=CARTESIAN_POINT('Ctrl Pts',(0.219088812841539,0.0874057747604746,
-0.968021268697603));
#51282=CARTESIAN_POINT('Ctrl Pts',(0.045063423665798,0.231536099175291,
-0.955301995876618));
#51283=CARTESIAN_POINT('Ctrl Pts',(-0.153432154943803,0.168551725236421,
-0.943579743597575));
#51284=CARTESIAN_POINT('Ctrl Pts',(-0.199002471583887,0.0506072086363436,
-0.936097248925528));
#51285=CARTESIAN_POINT('Ctrl Pts',(-0.199470377661838,-0.000183637774485384,
-0.932854511860477));
#51286=CARTESIAN_POINT('Ctrl Pts',(-0.199514910575122,-0.000180945758118245,
-0.997045488139523));
#51287=CARTESIAN_POINT('Ctrl Pts',(-0.199646183332245,-0.0143294565507365,
-0.996141661164988));
#51288=CARTESIAN_POINT('Ctrl Pts',(-0.191812275018386,-0.094702859673376,
-0.990998076583459));
#51289=CARTESIAN_POINT('Ctrl Pts',(-0.0828446630474759,-0.220853876562684,
-0.981614734394935));
#51290=CARTESIAN_POINT('Ctrl Pts',(0.140886058601026,-0.189184543449203,
-0.968895461573948));
#51291=CARTESIAN_POINT('Ctrl Pts',(0.23533107675241,0.0160921503462616,
-0.956176188752962));
#51292=CARTESIAN_POINT('Ctrl Pts',(0.113821839991816,0.206601698272528,
-0.943456915931977));
#51293=CARTESIAN_POINT('Ctrl Pts',(-0.112137310428092,0.20752083413038,
-0.93073764311099));
#51294=CARTESIAN_POINT('Ctrl Pts',(-0.19731146565357,0.0763457603254025,
-0.921933833846839));
#51295=CARTESIAN_POINT('Ctrl Pts',(-0.199782869629924,0.00515094640973097,
-0.917369782189683));
#51296=CARTESIAN_POINT('Ctrl Pts',(-0.199754371556151,9.02611351696076E-5,
-0.917045488139523));
#51297=CARTESIAN_POINT('Origin',(0.,0.,-1.69285451186048));
#51298=CARTESIAN_POINT('',(-0.199570634090872,0.000172606818067552,-1.09285451186048));
#51299=CARTESIAN_POINT('',(-0.199145756921865,3.13449059798551E-6,-1.07704548813952));
#51300=CARTESIAN_POINT('',(-0.199475,-2.40257419738789E-14,-1.69285451186048));
#51301=CARTESIAN_POINT('Ctrl Pts',(-0.199570634090872,0.000172606818067534,
-1.09285451186048));
#51302=CARTESIAN_POINT('Ctrl Pts',(-0.199077549402563,-0.0538459621402391,
-1.08940124926914));
#51303=CARTESIAN_POINT('Ctrl Pts',(-0.148502613272573,-0.174999101021697,
-1.08170822907082));
#51304=CARTESIAN_POINT('Ctrl Pts',(0.0564883808015244,-0.229016899394345,
-1.06977545126549));
#51305=CARTESIAN_POINT('Ctrl Pts',(0.223153219116496,-0.0764350585250314,
-1.0570561784445));
#51306=CARTESIAN_POINT('Ctrl Pts',(0.1850389529013,0.146288288263266,-1.04433690562352));
#51307=CARTESIAN_POINT('Ctrl Pts',(-0.022878425401603,0.234768513700057,
-1.03161763280253));
#51308=CARTESIAN_POINT('Ctrl Pts',(-0.177100422625592,0.130021041115852,
-1.02112350154819));
#51309=CARTESIAN_POINT('Ctrl Pts',(-0.199187632069763,0.0317106528655207,
-1.01486912790083));
#51310=CARTESIAN_POINT('Ctrl Pts',(-0.199149110574872,2.72391911226855E-5,
-1.01285451186048));
#51311=CARTESIAN_POINT('Ctrl Pts',(-0.199145785496325,3.13421856075122E-6,
-1.07704548813952));
#51312=CARTESIAN_POINT('Ctrl Pts',(-0.199141099283995,-0.0335269239555814,
-1.07491354014029));
#51313=CARTESIAN_POINT('Ctrl Pts',(-0.175194706262559,-0.133743751459225,
-1.06854183453407));
#51314=CARTESIAN_POINT('Ctrl Pts',(-0.0163801713107981,-0.235311204527198,
-1.05793037132085));
#51315=CARTESIAN_POINT('Ctrl Pts',(0.189011964525323,-0.141117505131332,
-1.04521109849986));
#51316=CARTESIAN_POINT('Ctrl Pts',(0.22095510870339,0.0825742873180875,
-1.03249182567888));
#51317=CARTESIAN_POINT('Ctrl Pts',(0.0501362695194371,0.230490840310171,
-1.01977255285789));
#51318=CARTESIAN_POINT('Ctrl Pts',(-0.151283044765976,0.171413945990171,
-1.00795710701144));
#51319=CARTESIAN_POINT('Ctrl Pts',(-0.199030396587344,0.0520397246651457,
-1.00038141877198));
#51320=CARTESIAN_POINT('Ctrl Pts',(-0.199514910575122,-0.000180945758118245,
-0.997045488139523));
#51321=CARTESIAN_POINT('Origin',(0.,0.,-1.69285451186048));
#51322=CARTESIAN_POINT('',(-0.199716653248,-0.000117807292186744,-1.17285451186048));
#51323=CARTESIAN_POINT('',(-0.199526448980684,0.000179680229220276,-1.15704548813952));
#51324=CARTESIAN_POINT('',(-0.199475,-2.40257419738789E-14,-1.69285451186048));
#51325=CARTESIAN_POINT('Ctrl Pts',(-0.199716653248,-0.000117807292186758,
-1.17285451186048));
#51326=CARTESIAN_POINT('Ctrl Pts',(-0.199764878894326,-0.00701292056885365,
-1.17241288585144));
#51327=CARTESIAN_POINT('Ctrl Pts',(-0.196308756330249,-0.0800545298160815,
-1.16773150223542));
#51328=CARTESIAN_POINT('Ctrl Pts',(-0.106358138767262,-0.21054126364045,
-1.15881036101239));
#51329=CARTESIAN_POINT('Ctrl Pts',(0.11948927064294,-0.203376477437402,
-1.14609108819141));
#51330=CARTESIAN_POINT('Ctrl Pts',(0.23568598380503,-0.00958093997281493,
-1.13337181537042));
#51331=CARTESIAN_POINT('Ctrl Pts',(0.13560275754475,0.193006656674328,-1.12065254254944));
#51332=CARTESIAN_POINT('Ctrl Pts',(-0.0889178905577564,0.218479486708672,
-1.10793326972845));
#51333=CARTESIAN_POINT('Ctrl Pts',(-0.193038342717315,0.0909790573946992,
-1.0986672594988));
#51334=CARTESIAN_POINT('Ctrl Pts',(-0.199682936193419,0.0124755621002766,
-1.09364100687614));
#51335=CARTESIAN_POINT('Ctrl Pts',(-0.199570634090872,0.000172606818067534,
-1.09285451186048));
#51336=CARTESIAN_POINT('Ctrl Pts',(-0.199526448980684,0.000179680229220268,
-1.15704548813952));
#51337=CARTESIAN_POINT('Ctrl Pts',(-0.199038978996149,-0.0524110445617291,
-1.1536854191156));
#51338=CARTESIAN_POINT('Ctrl Pts',(-0.150717860586543,-0.172153238428849,
-1.14608559248468));
#51339=CARTESIAN_POINT('Ctrl Pts',(0.051446362342642,-0.230201965217191,
-1.13424600824677));
#51340=CARTESIAN_POINT('Ctrl Pts',(0.221421171676079,-0.0813162820208495,
-1.12152673542578));
#51341=CARTESIAN_POINT('Ctrl Pts',(0.188206309629664,0.142190217679984,
-1.10880746260479));
#51342=CARTESIAN_POINT('Ctrl Pts',(-0.0177182256432174,0.235214237384252,
-1.09608818978381));
#51343=CARTESIAN_POINT('Ctrl Pts',(-0.175592589825075,0.132978269443307,
-1.08550086496205));
#51344=CARTESIAN_POINT('Ctrl Pts',(-0.199150418650312,0.0331535575844161,
-1.07915329774729));
#51345=CARTESIAN_POINT('Ctrl Pts',(-0.199145785496325,3.13421856075122E-6,
-1.07704548813952));
#51346=CARTESIAN_POINT('Origin',(0.,0.,-1.69285451186048));
#51347=CARTESIAN_POINT('',(-0.199205771072305,-0.000109377308561953,-1.25285451186048));
#51348=CARTESIAN_POINT('',(-0.199747301454138,-9.62307387931682E-5,-1.23704548813952));
#51349=CARTESIAN_POINT('',(-0.199475,-2.40257419738789E-14,-1.69285451186048));
#51350=CARTESIAN_POINT('Ctrl Pts',(-0.199205771072305,-0.000109377308561975,
-1.25285451186048));
#51351=CARTESIAN_POINT('Ctrl Pts',(-0.199336082765098,-0.0263504578365746,
-1.25118476482675));
#51352=CARTESIAN_POINT('Ctrl Pts',(-0.182297595797127,-0.119059395555614,
-1.24527526018603));
#51353=CARTESIAN_POINT('Ctrl Pts',(-0.0418587330474375,-0.232136864756142,
-1.23512599793831));
#51354=CARTESIAN_POINT('Ctrl Pts',(0.172554404057684,-0.16082492044269,
-1.22240672511732));
#51355=CARTESIAN_POINT('Ctrl Pts',(0.228621017531538,0.0580698516161886,
-1.20968745229634));
#51356=CARTESIAN_POINT('Ctrl Pts',(0.0748909390303039,0.223676160212552,
-1.19696817947535));
#51357=CARTESIAN_POINT('Ctrl Pts',(-0.13983981787387,0.185400262373372,
-1.1846905326634));
#51358=CARTESIAN_POINT('Ctrl Pts',(-0.199301896536666,0.0591824763686249,
-1.17665264345844));
#51359=CARTESIAN_POINT('Ctrl Pts',(-0.199716653248,-0.000117807292186758,
-1.17285451186048));
#51360=CARTESIAN_POINT('Ctrl Pts',(-0.199747301454138,-9.62307387932064E-5,
-1.23704548813952));
#51361=CARTESIAN_POINT('Ctrl Pts',(-0.199779601413921,-0.00553411054487472,
-1.2366970556979));
#51362=CARTESIAN_POINT('Ctrl Pts',(-0.197109635420976,-0.0771083999889113,
-1.23210886564928));
#51363=CARTESIAN_POINT('Ctrl Pts',(-0.110955233724902,-0.208155252443532,
-1.22328091799367));
#51364=CARTESIAN_POINT('Ctrl Pts',(0.11499503466161,-0.20595100143569,-1.21056164517268));
#51365=CARTESIAN_POINT('Ctrl Pts',(0.235418793778872,-0.0147534578031819,
-1.19784237235169));
#51366=CARTESIAN_POINT('Ctrl Pts',(0.139807803503312,0.189982765195607,
-1.18512309953071));
#51367=CARTESIAN_POINT('Ctrl Pts',(-0.0840994171703575,0.220379130181726,
-1.17240382670972));
#51368=CARTESIAN_POINT('Ctrl Pts',(-0.192069323928686,0.0939365155218052,
-1.16304462291266));
#51369=CARTESIAN_POINT('Ctrl Pts',(-0.199654071888705,0.0139482843396326,
-1.15792517672259));
#51370=CARTESIAN_POINT('Ctrl Pts',(-0.199526448980684,0.000179680229220268,
-1.15704548813952));
#51371=CARTESIAN_POINT('Origin',(0.,0.,-1.69285451186048));
#51372=CARTESIAN_POINT('',(-0.199316052586657,0.000164312921044613,-1.33285451186048));
#51373=CARTESIAN_POINT('',(-0.199232174843428,-0.0001279617224864,-1.31704548813952));
#51374=CARTESIAN_POINT('',(-0.199475,-2.40257419738789E-14,-1.69285451186048));
#51375=CARTESIAN_POINT('Ctrl Pts',(-0.199316052586657,0.000164312921044612,
-1.33285451186048));
#51376=CARTESIAN_POINT('Ctrl Pts',(-0.198964032636456,-0.0453141414772884,
-1.32995664380206));
#51377=CARTESIAN_POINT('Ctrl Pts',(-0.160936875144002,-0.157862593974603,
-1.32281901813664));
#51378=CARTESIAN_POINT('Ctrl Pts',(0.0261212891997552,-0.23442986171762,
-1.31144163486423));
#51379=CARTESIAN_POINT('Ctrl Pts',(0.211271323804121,-0.104900464490951,
-1.29872236204324));
#51380=CARTESIAN_POINT('Ctrl Pts',(0.202545781291298,0.120892023328345,
-1.28600308922225));
#51381=CARTESIAN_POINT('Ctrl Pts',(0.00795180094256099,0.2357465737612,
-1.27328381640127));
#51382=CARTESIAN_POINT('Ctrl Pts',(-0.167435612371573,0.147587691128348,
-1.26223429061401));
#51383=CARTESIAN_POINT('Ctrl Pts',(-0.199005200314261,0.0402798870822277,
-1.25542452243375));
#51384=CARTESIAN_POINT('Ctrl Pts',(-0.199205771072305,-0.000109377308561975,
-1.25285451186048));
#51385=CARTESIAN_POINT('Ctrl Pts',(-0.199232174843428,-0.000127961722486429,
-1.31704548813952));
#51386=CARTESIAN_POINT('Ctrl Pts',(-0.199377275158137,-0.0248962199241702,
-1.31546893467321));
#51387=CARTESIAN_POINT('Ctrl Pts',(-0.183601317566453,-0.116094454191202,
-1.30965262359989));
#51388=CARTESIAN_POINT('Ctrl Pts',(-0.0469455445028857,-0.231161825669147,
-1.29959655491958));
#51389=CARTESIAN_POINT('Ctrl Pts',(0.168981655819671,-0.164574825627453,
-1.2868772820986));
#51390=CARTESIAN_POINT('Ctrl Pts',(0.229840901678433,0.0530361437331597,
-1.27415800927761));
#51391=CARTESIAN_POINT('Ctrl Pts',(0.0797840170844622,0.22197789021412,
-1.26143873645663));
#51392=CARTESIAN_POINT('Ctrl Pts',(-0.137371270637,0.188171270116292,-1.24906789607726));
#51393=CARTESIAN_POINT('Ctrl Pts',(-0.199386572568632,0.0606345050018434,
-1.24093681330489));
#51394=CARTESIAN_POINT('Ctrl Pts',(-0.199747301454138,-9.62307387932064E-5,
-1.23704548813952));
#51395=CARTESIAN_POINT('Origin',(0.,0.,-1.69285451186048));
#51396=CARTESIAN_POINT('',(-0.199798277749891,3.2585087406417E-5,-1.41285451186048));
#51397=CARTESIAN_POINT('',(-0.199280157075849,0.000151800363860324,-1.39704548813952));
#51398=CARTESIAN_POINT('',(-0.199475,-2.40257419738789E-14,-1.69285451186048));
#51399=CARTESIAN_POINT('Ctrl Pts',(-0.199798277749891,3.25850874064147E-5,
-1.41285451186048));
#51400=CARTESIAN_POINT('Ctrl Pts',(-0.199650935957592,-0.0643178193354115,
-1.40872852277736));
#51401=CARTESIAN_POINT('Ctrl Pts',(-0.13090933192774,-0.195061621925552,
-1.40036277608725));
#51402=CARTESIAN_POINT('Ctrl Pts',(0.0919285341003431,-0.217230095550597,
-1.38775727179014));
#51403=CARTESIAN_POINT('Ctrl Pts',(0.232421027333792,-0.0402530662671006,
-1.37503799896916));
#51404=CARTESIAN_POINT('Ctrl Pts',(0.159628279467637,0.173661654101238,
-1.36231872614817));
#51405=CARTESIAN_POINT('Ctrl Pts',(-0.059648436931805,0.228214293208638,
-1.34959945332718));
#51406=CARTESIAN_POINT('Ctrl Pts',(-0.186700851040545,0.108627921988768,
-1.33977804856462));
#51407=CARTESIAN_POINT('Ctrl Pts',(-0.199479059280731,0.0212236094148981,
-1.33419640140905));
#51408=CARTESIAN_POINT('Ctrl Pts',(-0.199316052586657,0.000164312921044612,
-1.33285451186048));
#51409=CARTESIAN_POINT('Ctrl Pts',(-0.199280157075849,0.000151800363860317,
-1.39704548813952));
#51410=CARTESIAN_POINT('Ctrl Pts',(-0.198969065654869,-0.0438841150085429,
-1.39424081364851));
#51411=CARTESIAN_POINT('Ctrl Pts',(-0.162845928153855,-0.154951516497137,
-1.3871963815505));
#51412=CARTESIAN_POINT('Ctrl Pts',(0.0209676361572253,-0.234946916486012,
-1.3759121918455));
#51413=CARTESIAN_POINT('Ctrl Pts',(0.208917198058643,-0.109513915389758,
-1.36319291902451));
#51414=CARTESIAN_POINT('Ctrl Pts',(0.205151275600481,0.116415675121088,
-1.35047364620353));
#51415=CARTESIAN_POINT('Ctrl Pts',(0.0131260573719064,0.235515146136983,
-1.33775437338254));
#51416=CARTESIAN_POINT('Ctrl Pts',(-0.165649961001676,0.150517507050773,
-1.32661165402787));
#51417=CARTESIAN_POINT('Ctrl Pts',(-0.198987063106209,0.0417119943648623,
-1.3197086922802));
#51418=CARTESIAN_POINT('Ctrl Pts',(-0.199232174843428,-0.000127961722486429,
-1.31704548813952));
#51419=CARTESIAN_POINT('Origin',(0.,0.,-1.69285451186048));
#51420=CARTESIAN_POINT('',(-0.199405781844198,-0.000173944371801526,-1.49285451186048));
#51421=CARTESIAN_POINT('',(-0.199789055725603,5.64207037231385E-5,-1.47704548813952));
#51422=CARTESIAN_POINT('',(-0.199475,-2.40257419738789E-14,-1.69285451186048));
#51423=CARTESIAN_POINT('Ctrl Pts',(-0.199405781844198,-0.000173944371801573,
-1.49285451186048));
#51424=CARTESIAN_POINT('Ctrl Pts',(-0.19957890617447,-0.0176527449068341,
-1.49174015935966));
#51425=CARTESIAN_POINT('Ctrl Pts',(-0.189548811499923,-0.101452112831176,
-1.48638604925185));
#51426=CARTESIAN_POINT('Ctrl Pts',(-0.0717210652972735,-0.224640326086787,
-1.47679218153704));
#51427=CARTESIAN_POINT('Ctrl Pts',(0.150056091147136,-0.181992142895108,
-1.46407290871606));
#51428=CARTESIAN_POINT('Ctrl Pts',(0.234263183139456,0.0277545022598852,
-1.45135363589507));
#51429=CARTESIAN_POINT('Ctrl Pts',(0.103427579470953,0.211984146348435,
-1.43863436307408));
#51430=CARTESIAN_POINT('Ctrl Pts',(-0.122283649797262,0.201709159043015,
-1.4259150902531));
#51431=CARTESIAN_POINT('Ctrl Pts',(-0.198975701192239,0.069702259029704,
-1.41732180651523));
#51432=CARTESIAN_POINT('Ctrl Pts',(-0.199802340498938,0.00180695975846793,
-1.41296828038436));
#51433=CARTESIAN_POINT('Ctrl Pts',(-0.199798277749891,3.25850874064147E-5,
-1.41285451186048));
#51434=CARTESIAN_POINT('Ctrl Pts',(-0.199789055725603,5.64207037231446E-5,
-1.47704548813952));
#51435=CARTESIAN_POINT('Ctrl Pts',(-0.199545877469372,-0.0628540486324878,
-1.47301269262382));
#51436=CARTESIAN_POINT('Ctrl Pts',(-0.133507643719009,-0.192336071597138,
-1.46474013950111));
#51437=CARTESIAN_POINT('Ctrl Pts',(0.0871316433491625,-0.219198425104216,
-1.45222782877142));
#51438=CARTESIAN_POINT('Ctrl Pts',(0.231483862146741,-0.0453453044496629,
-1.43950855595043));
#51439=CARTESIAN_POINT('Ctrl Pts',(0.163401374080225,0.170114283366123,
-1.42678928312944));
#51440=CARTESIAN_POINT('Ctrl Pts',(-0.0546225385477825,0.229469265901282,
-1.41407001030846));
#51441=CARTESIAN_POINT('Ctrl Pts',(-0.185501093092507,0.1115929665413,-1.40415541197848));
#51442=CARTESIAN_POINT('Ctrl Pts',(-0.199439334922407,0.0226838977071687,
-1.39848057125551));
#51443=CARTESIAN_POINT('Ctrl Pts',(-0.199280157075849,0.000151800363860317,
-1.39704548813952));
#51444=CARTESIAN_POINT('Origin',(5.69858952725515E-17,8.58067791224701E-18,
-0.0149499999999998));
#51445=CARTESIAN_POINT('',(-0.0796899944392906,0.231730462577249,-0.0149499999999998));
#51446=CARTESIAN_POINT('Ctrl Pts',(0.197120359334095,-0.0326678654691807,
-0.0149499999999996));
#51447=CARTESIAN_POINT('Ctrl Pts',(0.198391584513283,-0.0282478211509381,
-0.0149499999999996));
#51448=CARTESIAN_POINT('Ctrl Pts',(0.199497230955055,-0.0237887632912905,
-0.0149499999999994));
#51449=CARTESIAN_POINT('Ctrl Pts',(0.200432280241851,-0.0192980722140279,
-0.0149499999999992));
#51450=CARTESIAN_POINT('Ctrl Pts',(0.202577210314895,-0.00899677743053964,
-0.014949999999999));
#51451=CARTESIAN_POINT('Ctrl Pts',(0.203826056148701,0.00147035978450179,
-0.014949999999999));
#51452=CARTESIAN_POINT('Ctrl Pts',(0.204234176055474,0.012009143396064,
-0.014949999999999));
#51453=CARTESIAN_POINT('Ctrl Pts',(0.204460723116552,0.0178592144534165,
-0.014949999999999));
#51454=CARTESIAN_POINT('Ctrl Pts',(0.20442720843244,0.0237345702014736,
-0.0149499999999995));
#51455=CARTESIAN_POINT('Ctrl Pts',(0.204142818256796,0.02959475413324,-0.0149499999999996));
#51456=CARTESIAN_POINT('Ctrl Pts',(0.203701771739557,0.03868302065875,-0.0149499999999997));
#51457=CARTESIAN_POINT('Ctrl Pts',(0.202658984688022,0.0477465139947516,
-0.0149499999999992));
#51458=CARTESIAN_POINT('Ctrl Pts',(0.201046156693127,0.0567277105127938,
-0.014949999999999));
#51459=CARTESIAN_POINT('Ctrl Pts',(0.200183599069131,0.061530950259233,
-0.0149499999999989));
#51460=CARTESIAN_POINT('Ctrl Pts',(0.199157809647221,0.0663107083864419,
-0.0149499999999991));
#51461=CARTESIAN_POINT('Ctrl Pts',(0.19797238261792,0.0710583673294022,
-0.0149499999999992));
#51462=CARTESIAN_POINT('Ctrl Pts',(0.196938500061177,0.0751990876311717,
-0.0149499999999992));
#51463=CARTESIAN_POINT('Ctrl Pts',(0.195783593393406,0.079312838501636,
-0.014949999999999));
#51464=CARTESIAN_POINT('Ctrl Pts',(0.194513872543076,0.0833835575473151,
-0.0149499999999991));
#51465=CARTESIAN_POINT('Ctrl Pts',(0.190330656324442,0.0967949289751111,
-0.0149499999999993));
#51466=CARTESIAN_POINT('Ctrl Pts',(0.184897520196834,0.109771278820074,
-0.0149499999999998));
#51467=CARTESIAN_POINT('Ctrl Pts',(0.178311313802482,0.12211617811317,-0.0149499999999997));
#51468=CARTESIAN_POINT('Ctrl Pts',(0.173661048230523,0.130832433987144,
-0.0149499999999997));
#51469=CARTESIAN_POINT('Ctrl Pts',(0.168434777087133,0.139234261100576,
-0.0149499999999995));
#51470=CARTESIAN_POINT('Ctrl Pts',(0.16265144281701,0.147249217570727,-0.0149499999999996));
#51471=CARTESIAN_POINT('Ctrl Pts',(0.160514169925959,0.150211202541075,
-0.0149499999999997));
#51472=CARTESIAN_POINT('Ctrl Pts',(0.158302456051775,0.153117610750161,
-0.0149499999999994));
#51473=CARTESIAN_POINT('Ctrl Pts',(0.156022862593314,0.155958527256897,
-0.0149499999999994));
#51474=CARTESIAN_POINT('Ctrl Pts',(0.150502215199784,0.162838569068711,
-0.0149499999999995));
#51475=CARTESIAN_POINT('Ctrl Pts',(0.144575729488352,0.169346199310948,
-0.0149499999999991));
#51476=CARTESIAN_POINT('Ctrl Pts',(0.138263937757876,0.175434414556545,
-0.0149499999999992));
#51477=CARTESIAN_POINT('Ctrl Pts',(0.131281545757466,0.182169476048256,
-0.0149499999999993));
#51478=CARTESIAN_POINT('Ctrl Pts',(0.123827770680868,0.188391667069538,
-0.0149499999999997));
#51479=CARTESIAN_POINT('Ctrl Pts',(0.115968513453136,0.194097818772095,
-0.0149499999999997));
#51480=CARTESIAN_POINT('Ctrl Pts',(0.111698380331938,0.197198115234424,
-0.0149499999999997));
#51481=CARTESIAN_POINT('Ctrl Pts',(0.107308365134894,0.200145943520289,
-0.0149499999999997));
#51482=CARTESIAN_POINT('Ctrl Pts',(0.102807943122472,0.202939758658773,
-0.0149499999999997));
#51483=CARTESIAN_POINT('Ctrl Pts',(0.0986065241053424,0.20554795585023,
-0.0149499999999998));
#51484=CARTESIAN_POINT('Ctrl Pts',(0.0943067130227581,0.208022653727126,
-0.0149500000000002));
#51485=CARTESIAN_POINT('Ctrl Pts',(0.0899371597296005,0.210351797381489,
-0.0149500000000001));
#51486=CARTESIAN_POINT('Ctrl Pts',(0.0771241543606563,0.217181632869509,
-0.0149499999999997));
#51487=CARTESIAN_POINT('Ctrl Pts',(0.063678628286122,0.222786554309641,
-0.0149499999999996));
#51488=CARTESIAN_POINT('Ctrl Pts',(0.0498091452572496,0.227155755310556,
-0.0149499999999995));
#51489=CARTESIAN_POINT('Ctrl Pts',(0.0425067586415354,0.229456172337205,
-0.0149499999999994));
#51490=CARTESIAN_POINT('Ctrl Pts',(0.0350861724152127,0.231413431882226,
-0.0149499999999995));
#51491=CARTESIAN_POINT('Ctrl Pts',(0.0275745532422898,0.233021449591895,
-0.0149499999999995));
#51492=CARTESIAN_POINT('Ctrl Pts',(0.0230174457248419,0.233996992870145,
-0.0149499999999994));
#51493=CARTESIAN_POINT('Ctrl Pts',(0.0184267979876164,0.234843932724277,
-0.0149499999999994));
#51494=CARTESIAN_POINT('Ctrl Pts',(0.0138084601729489,0.235560277476396,
-0.0149499999999995));
#51495=CARTESIAN_POINT('Ctrl Pts',(0.00959333086335831,0.236214081048503,
-0.0149499999999995));
#51496=CARTESIAN_POINT('Ctrl Pts',(0.00536398260013057,0.23675765141323,
-0.01495));
#51497=CARTESIAN_POINT('Ctrl Pts',(0.00112883840488462,0.237190302563417,
-0.01495));
#51498=CARTESIAN_POINT('Ctrl Pts',(-0.0140084017468552,0.238736683054937,
-0.01495));
#51499=CARTESIAN_POINT('Ctrl Pts',(-0.0292325594370678,0.238871969867428,
-0.0149499999999999));
#51500=CARTESIAN_POINT('Ctrl Pts',(-0.0443347582390812,0.237560856560192,
-0.0149499999999998));
#51501=CARTESIAN_POINT('Ctrl Pts',(-0.0562275002790541,0.236528375624631,
-0.0149499999999998));
#51502=CARTESIAN_POINT('Ctrl Pts',(-0.0680455254831802,0.234598199446658,
-0.0149499999999998));
#51503=CARTESIAN_POINT('Ctrl Pts',(-0.0796899944392906,0.231730462577249,
-0.0149499999999998));
#51504=CARTESIAN_POINT('',(-0.24505,-3.00099698131059E-17,-0.01495));
#51505=CARTESIAN_POINT('Origin',(0.,0.,-0.0149499999999999));
#51506=CARTESIAN_POINT('',(-0.231938272394163,0.0797165085725884,-0.0149499999999999));
#51507=CARTESIAN_POINT('Origin',(0.,0.,-0.0149499999999999));
#51508=CARTESIAN_POINT('Ctrl Pts',(-0.232146082211074,0.0797430227058928,
-0.0149499999999999));
#51509=CARTESIAN_POINT('Ctrl Pts',(-0.23350718091485,0.0743161424960959,
-0.0149499999999999));
#51510=CARTESIAN_POINT('Ctrl Pts',(-0.234667147495365,0.0688472522854195,
-0.01495));
#51511=CARTESIAN_POINT('Ctrl Pts',(-0.235618162261078,0.0633433287759428,
-0.01495));
#51512=CARTESIAN_POINT('Ctrl Pts',(-0.237412919095364,0.0529563140941966,
-0.01495));
#51513=CARTESIAN_POINT('Ctrl Pts',(-0.238464189863105,0.0424443716233503,
-0.0149500000000004));
#51514=CARTESIAN_POINT('Ctrl Pts',(-0.238796729904135,0.0318787064057965,
-0.0149500000000006));
#51515=CARTESIAN_POINT('Ctrl Pts',(-0.238949765616349,0.0270163623206224,
-0.0149500000000007));
#51516=CARTESIAN_POINT('Ctrl Pts',(-0.23895041575299,0.0221426647714983,
-0.0149500000000005));
#51517=CARTESIAN_POINT('Ctrl Pts',(-0.238800283436524,0.0172647976316243,
-0.0149500000000006));
#51518=CARTESIAN_POINT('Ctrl Pts',(-0.238643002975604,0.0121546840322981,
-0.0149500000000006));
#51519=CARTESIAN_POINT('Ctrl Pts',(-0.23832047459253,0.00704905816868219,
-0.0149500000000003));
#51520=CARTESIAN_POINT('Ctrl Pts',(-0.237836102473065,0.00195870824191732,
-0.0149500000000004));
#51521=CARTESIAN_POINT('Ctrl Pts',(-0.236971800239444,-0.00712439261134424,
-0.0149500000000004));
#51522=CARTESIAN_POINT('Ctrl Pts',(-0.235592455321206,-0.0161618930984169,
-0.0149500000000005));
#51523=CARTESIAN_POINT('Ctrl Pts',(-0.233711732266915,-0.0251065474147256,
-0.0149500000000005));
#51524=CARTESIAN_POINT('Ctrl Pts',(-0.232387572468453,-0.0314042059826735,
-0.0149500000000005));
#51525=CARTESIAN_POINT('Ctrl Pts',(-0.23081472952064,-0.0376558054885507,
-0.0149500000000003));
#51526=CARTESIAN_POINT('Ctrl Pts',(-0.228996206985243,-0.0438437591894054,
-0.0149500000000002));
#51527=CARTESIAN_POINT('Ctrl Pts',(-0.227643304056364,-0.0484473318824611,
-0.0149500000000002));
#51528=CARTESIAN_POINT('Ctrl Pts',(-0.226156739718812,-0.053007313491729,
-0.0149500000000003));
#51529=CARTESIAN_POINT('Ctrl Pts',(-0.22454077011411,-0.0575117245253547,
-0.0149500000000003));
#51530=CARTESIAN_POINT('Ctrl Pts',(-0.219610988257616,-0.0712531734505997,
-0.0149500000000004));
#51531=CARTESIAN_POINT('Ctrl Pts',(-0.213475163641887,-0.0844959724585875,
-0.0149500000000002));
#51532=CARTESIAN_POINT('Ctrl Pts',(-0.206180419574474,-0.0970381019544846,
-0.0149500000000001));
#51533=CARTESIAN_POINT('Ctrl Pts',(-0.202999702259208,-0.102506829587592,
-0.0149500000000001));
#51534=CARTESIAN_POINT('Ctrl Pts',(-0.1995981365692,-0.107841939337988,
-0.0149500000000007));
#51535=CARTESIAN_POINT('Ctrl Pts',(-0.195977488873056,-0.113024301602003,
-0.0149500000000007));
#51536=CARTESIAN_POINT('Ctrl Pts',(-0.193573372357027,-0.116465399371397,
-0.0149500000000008));
#51537=CARTESIAN_POINT('Ctrl Pts',(-0.191072637928957,-0.119839117844746,
-0.0149500000000006));
#51538=CARTESIAN_POINT('Ctrl Pts',(-0.188475540395292,-0.123139391550832,
-0.0149500000000006));
#51539=CARTESIAN_POINT('Ctrl Pts',(-0.185966800671422,-0.126327384161342,
-0.0149500000000005));
#51540=CARTESIAN_POINT('Ctrl Pts',(-0.183373622103193,-0.129439792556405,
-0.0149500000000006));
#51541=CARTESIAN_POINT('Ctrl Pts',(-0.180698977833861,-0.132470011526652,
-0.0149500000000007));
#51542=CARTESIAN_POINT('Ctrl Pts',(-0.175543672442891,-0.138310677656444,
-0.0149500000000007));
#51543=CARTESIAN_POINT('Ctrl Pts',(-0.170083732537213,-0.143849024363428,
-0.0149500000000004));
#51544=CARTESIAN_POINT('Ctrl Pts',(-0.164325057077125,-0.149051164015221,
-0.0149500000000004));
#51545=CARTESIAN_POINT('Ctrl Pts',(-0.153833964139055,-0.158528366011066,
-0.0149500000000006));
#51546=CARTESIAN_POINT('Ctrl Pts',(-0.142351798966231,-0.166892708688512,
-0.0149500000000005));
#51547=CARTESIAN_POINT('Ctrl Pts',(-0.130079353982082,-0.174080052076584,
-0.0149500000000005));
#51548=CARTESIAN_POINT('Ctrl Pts',(-0.125535338402389,-0.176741249610913,
-0.0149500000000005));
#51549=CARTESIAN_POINT('Ctrl Pts',(-0.120878764860052,-0.179242193486494,
-0.0149500000000003));
#51550=CARTESIAN_POINT('Ctrl Pts',(-0.116145470012991,-0.181566385959855,
-0.0149500000000003));
#51551=CARTESIAN_POINT('Ctrl Pts',(-0.104698292289123,-0.18718730017853,
-0.0149500000000001));
#51552=CARTESIAN_POINT('Ctrl Pts',(-0.0927779473770901,-0.191793807979919,
-0.0149500000000003));
#51553=CARTESIAN_POINT('Ctrl Pts',(-0.0805361235299436,-0.19534629546693,
-0.0149500000000004));
#51554=CARTESIAN_POINT('Ctrl Pts',(-0.0695096581407387,-0.198546094844067,
-0.0149500000000005));
#51555=CARTESIAN_POINT('Ctrl Pts',(-0.0582215533463788,-0.200890382869549,
-0.0149500000000003));
#51556=CARTESIAN_POINT('Ctrl Pts',(-0.0467843692613105,-0.202323848970006,
-0.0149500000000003));
#51557=CARTESIAN_POINT('Ctrl Pts',(-0.0426471414161356,-0.202842383586728,
-0.0149500000000003));
#51558=CARTESIAN_POINT('Ctrl Pts',(-0.0384978609908941,-0.203240430888916,
-0.0149500000000004));
#51559=CARTESIAN_POINT('Ctrl Pts',(-0.0343490018043639,-0.203515797544261,
-0.0149500000000004));
#51560=CARTESIAN_POINT('Ctrl Pts',(-0.0213910422852966,-0.204375838777875,
-0.0149500000000003));
#51561=CARTESIAN_POINT('Ctrl Pts',(-0.00841434859516882,-0.204045491679898,
-0.0149500000000002));
#51562=CARTESIAN_POINT('Ctrl Pts',(0.00441495196016681,-0.202455457095622,
-0.0149500000000002));
#51563=CARTESIAN_POINT('Ctrl Pts',(0.013943768462285,-0.201274477063217,
-0.0149500000000001));
#51564=CARTESIAN_POINT('Ctrl Pts',(0.0233913298848719,-0.199397633716378,
-0.0149500000000001));
#51565=CARTESIAN_POINT('Ctrl Pts',(0.0326814423280684,-0.196779569448551,
-0.01495));
#51566=CARTESIAN_POINT('Ctrl Pts',(-0.0648690538289174,-0.188632662814108,
-1.54126273851832));
#51567=CARTESIAN_POINT('Ctrl Pts',(-0.00205630422489446,-0.210233395022512,
-1.53702298091132));
#51568=CARTESIAN_POINT('Ctrl Pts',(0.14575417320045,-0.185369963268203,
-1.52854346569733));
#51569=CARTESIAN_POINT('Ctrl Pts',(0.234947663922723,0.022663611902651,
-1.51582419287635));
#51570=CARTESIAN_POINT('Ctrl Pts',(0.107989171190762,0.209631807114936,
-1.50310492005536));
#51571=CARTESIAN_POINT('Ctrl Pts',(-0.117789854919609,0.204361256460409,
-1.49038564723437));
#51572=CARTESIAN_POINT('Ctrl Pts',(-0.235621695359832,0.01148780516709,
-1.47766637441339));
#51573=CARTESIAN_POINT('Ctrl Pts',(-0.137157166917276,-0.191891750082203,
-1.4649471015924));
#51574=CARTESIAN_POINT('Ctrl Pts',(0.0871316433491625,-0.219198425104216,
-1.45222782877142));
#51575=CARTESIAN_POINT('Ctrl Pts',(0.231483862146741,-0.0453453044496629,
-1.43950855595043));
#51576=CARTESIAN_POINT('Ctrl Pts',(0.163401374080225,0.170114283366123,
-1.42678928312944));
#51577=CARTESIAN_POINT('Ctrl Pts',(-0.0546225385477825,0.229469265901282,
-1.41407001030846));
#51578=CARTESIAN_POINT('Ctrl Pts',(-0.222524453105232,0.0782477276413624,
-1.40135073748747));
#51579=CARTESIAN_POINT('Ctrl Pts',(-0.186222683554777,-0.144777986019408,
-1.38863146466649));
#51580=CARTESIAN_POINT('Ctrl Pts',(0.0209676361572253,-0.234946916486012,
-1.3759121918455));
#51581=CARTESIAN_POINT('Ctrl Pts',(0.208917198058643,-0.109513915389758,
-1.36319291902451));
#51582=CARTESIAN_POINT('Ctrl Pts',(0.205151275600481,0.116415675121088,
-1.35047364620353));
#51583=CARTESIAN_POINT('Ctrl Pts',(0.0131260573719064,0.235515146136983,
-1.33775437338254));
#51584=CARTESIAN_POINT('Ctrl Pts',(-0.190944500197199,0.138491419139472,
-1.32503510056156));
#51585=CARTESIAN_POINT('Ctrl Pts',(-0.219792619778126,-0.0856205274590762,
-1.31231582774057));
#51586=CARTESIAN_POINT('Ctrl Pts',(-0.0469455445028857,-0.231161825669147,
-1.29959655491958));
#51587=CARTESIAN_POINT('Ctrl Pts',(0.168981655819671,-0.164574825627453,
-1.2868772820986));
#51588=CARTESIAN_POINT('Ctrl Pts',(0.229840901678433,0.0530361437331597,
-1.27415800927761));
#51589=CARTESIAN_POINT('Ctrl Pts',(0.0797840170844622,0.22197789021412,
-1.26143873645663));
#51590=CARTESIAN_POINT('Ctrl Pts',(-0.143487584872076,0.187219085557888,
-1.24871946363564));
#51591=CARTESIAN_POINT('Ctrl Pts',(-0.235086162299716,-0.019343454534662,
-1.23600019081465));
#51592=CARTESIAN_POINT('Ctrl Pts',(-0.110955233724902,-0.208155252443532,
-1.22328091799367));
#51593=CARTESIAN_POINT('Ctrl Pts',(0.11499503466161,-0.20595100143569,-1.21056164517268));
#51594=CARTESIAN_POINT('Ctrl Pts',(0.235418793778872,-0.0147534578031819,
-1.19784237235169));
#51595=CARTESIAN_POINT('Ctrl Pts',(0.139807803503312,0.189982765195607,
-1.18512309953071));
#51596=CARTESIAN_POINT('Ctrl Pts',(-0.0840994171703575,0.220379130181726,
-1.17240382670972));
#51597=CARTESIAN_POINT('Ctrl Pts',(-0.230831845515026,0.0485420650925855,
-1.15968455388874));
#51598=CARTESIAN_POINT('Ctrl Pts',(-0.165738789974153,-0.167840181382976,
-1.14696528106775));
#51599=CARTESIAN_POINT('Ctrl Pts',(0.051446362342642,-0.230201965217191,
-1.13424600824677));
#51600=CARTESIAN_POINT('Ctrl Pts',(0.221421171676079,-0.0813162820208495,
-1.12152673542578));
#51601=CARTESIAN_POINT('Ctrl Pts',(0.188206309629664,0.142190217679984,
-1.10880746260479));
#51602=CARTESIAN_POINT('Ctrl Pts',(-0.0177182256432174,0.235214237384252,
-1.09608818978381));
#51603=CARTESIAN_POINT('Ctrl Pts',(-0.207383428447063,0.112391221159588,
-1.08336891696282));
#51604=CARTESIAN_POINT('Ctrl Pts',(-0.206740855544523,-0.113568884985925,
-1.07064964414184));
#51605=CARTESIAN_POINT('Ctrl Pts',(-0.0163801713107981,-0.235311204527198,
-1.05793037132085));
#51606=CARTESIAN_POINT('Ctrl Pts',(0.189011964525323,-0.141117505131332,
-1.04521109849986));
#51607=CARTESIAN_POINT('Ctrl Pts',(0.22095510870339,0.0825742873180875,
-1.03249182567888));
#51608=CARTESIAN_POINT('Ctrl Pts',(0.0501362695194371,0.230490840310171,
-1.01977255285789));
#51609=CARTESIAN_POINT('Ctrl Pts',(-0.166690690978327,0.16689483673674,
-1.00705328003691));
#51610=CARTESIAN_POINT('Ctrl Pts',(-0.230552031857313,-0.0498541231462333,
-0.99433400721592));
#51611=CARTESIAN_POINT('Ctrl Pts',(-0.0828446630474759,-0.220853876562684,
-0.981614734394935));
#51612=CARTESIAN_POINT('Ctrl Pts',(0.140886058601026,-0.189184543449203,
-0.968895461573948));
#51613=CARTESIAN_POINT('Ctrl Pts',(0.23533107675241,0.0160921503462616,
-0.956176188752962));
#51614=CARTESIAN_POINT('Ctrl Pts',(0.113821839991816,0.206601698272528,
-0.943456915931977));
#51615=CARTESIAN_POINT('Ctrl Pts',(-0.112137310428092,0.20752083413038,
-0.93073764311099));
#51616=CARTESIAN_POINT('Ctrl Pts',(-0.235192375014876,0.0180061023843909,
-0.918018370290004));
#51617=CARTESIAN_POINT('Ctrl Pts',(-0.142420465925963,-0.188032135215358,
-0.905299097469019));
#51618=CARTESIAN_POINT('Ctrl Pts',(0.0810452130963459,-0.22152053273316,
-0.892579824648032));
#51619=CARTESIAN_POINT('Ctrl Pts',(0.230138825114443,-0.0517280790592424,
-0.879860551827046));
#51620=CARTESIAN_POINT('Ctrl Pts',(0.168042911338648,0.165533238163961,
-0.86714127900606));
#51621=CARTESIAN_POINT('Ctrl Pts',(-0.0482595025397965,0.230891085585448,
-0.854422006185075));
#51622=CARTESIAN_POINT('Ctrl Pts',(-0.220276031794642,0.0843690867855101,
-0.841702733364088));
#51623=CARTESIAN_POINT('Ctrl Pts',(-0.190153740381844,-0.139575169736631,
-0.828983460543103));
#51624=CARTESIAN_POINT('Ctrl Pts',(0.0144653063663763,-0.235436674925429,
-0.816264187722117));
#51625=CARTESIAN_POINT('Ctrl Pts',(0.205810099235619,-0.115247021830672,
-0.80354491490113));
#51626=CARTESIAN_POINT('Ctrl Pts',(0.208290899949043,0.110700379342769,
-0.790825642080145));
#51627=CARTESIAN_POINT('Ctrl Pts',(0.019631173350109,0.235062310932895,
-0.778106369259159));
#51628=CARTESIAN_POINT('Ctrl Pts',(-0.187043324066072,0.143716623640167,
-0.765387096438172));
#51629=CARTESIAN_POINT('Ctrl Pts',(-0.222075375264048,-0.0795122675412271,
-0.752667823617187));
#51630=CARTESIAN_POINT('Ctrl Pts',(-0.0533174176740989,-0.229775816744889,
-0.739948550796201));
#51631=CARTESIAN_POINT('Ctrl Pts',(0.164367878228055,-0.169182958938016,
-0.727229277975214));
#51632=CARTESIAN_POINT('Ctrl Pts',(0.231219110206101,0.0466625766939018,
-0.714510005154229));
#51633=CARTESIAN_POINT('Ctrl Pts',(0.085889480416779,0.219687664974506,
-0.701790732333243));
#51634=CARTESIAN_POINT('Ctrl Pts',(-0.138257613704705,0.191113854131237,
-0.689071459512257));
#51635=CARTESIAN_POINT('Ctrl Pts',(-0.235531026859181,-0.0128377714138675,
-0.676352186691271));
#51636=CARTESIAN_POINT('Ctrl Pts',(-0.116666698598652,-0.205008669149152,
-0.663632913870284));
#51637=CARTESIAN_POINT('Ctrl Pts',(0.109258160368663,-0.209051016216307,
-0.650913641049299));
#51638=CARTESIAN_POINT('Ctrl Pts',(0.234921018494109,-0.0212553065822581,
-0.638194368228312));
#51639=CARTESIAN_POINT('Ctrl Pts',(0.145005916359623,0.186045578310588,
-0.625475095407328));
#51640=CARTESIAN_POINT('Ctrl Pts',(-0.0779755238778273,0.222619609792564,
-0.612755822586341));
#51641=CARTESIAN_POINT('Ctrl Pts',(-0.229401832541543,0.0549042094451505,
-0.600036549765355));
#51642=CARTESIAN_POINT('Ctrl Pts',(-0.17031492507753,-0.163194666837034,
-0.587317276944369));
#51643=CARTESIAN_POINT('Ctrl Pts',(0.0450634218898312,-0.231536090050329,
-0.574598004123383));
#51644=CARTESIAN_POINT('Ctrl Pts',(0.219088804207135,-0.0874057713157602,
-0.561878731302397));
#51645=CARTESIAN_POINT('Ctrl Pts',(0.192064838835073,0.136933453441709,
-0.54915945848141));
#51646=CARTESIAN_POINT('Ctrl Pts',(-0.0112096232321388,0.235614128046703,
-0.536440185660426));
#51647=CARTESIAN_POINT('Ctrl Pts',(-0.204197446295501,0.118080802481237,
-0.523720912839439));
#51648=CARTESIAN_POINT('Ctrl Pts',(-0.209801146623257,-0.10781072239708,
-0.511001640018453));
#51649=CARTESIAN_POINT('Ctrl Pts',(-0.0228784244999453,-0.234768504447706,
-0.498282367197467));
#51650=CARTESIAN_POINT('Ctrl Pts',(0.185038945608821,-0.146288282497961,
-0.485563094376481));
#51651=CARTESIAN_POINT('Ctrl Pts',(0.223153210321907,0.0764350555126916,
-0.472843821555495));
#51652=CARTESIAN_POINT('Ctrl Pts',(0.0564883785752809,0.229016890368669,
-0.46012454873451));
#51653=CARTESIAN_POINT('Ctrl Pts',(-0.162013660032506,0.171438755686017,
-0.447405275913523));
#51654=CARTESIAN_POINT('Ctrl Pts',(-0.231842009976495,-0.0434621145155262,
-0.434686003092537));
#51655=CARTESIAN_POINT('Ctrl Pts',(-0.0889178870534499,-0.21847947809828,
-0.421966730271551));
#51656=CARTESIAN_POINT('Ctrl Pts',(0.135602752200584,-0.193006649067832,
-0.409247457450565));
#51657=CARTESIAN_POINT('Ctrl Pts',(0.235685974516513,0.00958093959523976,
-0.396528184629579));
#51658=CARTESIAN_POINT('Ctrl Pts',(0.119489265933811,0.20337646942222,-0.383808911808593));
#51659=CARTESIAN_POINT('Ctrl Pts',(-0.106358134575664,0.210541255342925,
-0.371089638987607));
#51660=CARTESIAN_POINT('Ctrl Pts',(-0.234604776065496,0.0245004495613401,
-0.358370366166621));
#51661=CARTESIAN_POINT('Ctrl Pts',(-0.147563660825225,-0.184023474027218,
-0.345651093345635));
#51662=CARTESIAN_POINT('Ctrl Pts',(0.0748909360789789,-0.223676151397489,
-0.332931820524649));
#51663=CARTESIAN_POINT('Ctrl Pts',(0.228621008521177,-0.0580698493273639,
-0.320212547703664));
#51664=CARTESIAN_POINT('Ctrl Pts',(0.172554397257742,0.160824914104033,
-0.307493274882677));
#51665=CARTESIAN_POINT('Ctrl Pts',(-0.0418587313987176,0.232136855608358,
-0.294774002061692));
#51666=CARTESIAN_POINT('Ctrl Pts',(-0.217859715111443,0.0904257549484663,
-0.282054729240705));
#51667=CARTESIAN_POINT('Ctrl Pts',(-0.193939241065975,-0.134265572685697,
-0.26933545641972));
#51668=CARTESIAN_POINT('Ctrl Pts',(0.00795180063483016,-0.23574656447556,
-0.256616183598734));
#51669=CARTESIAN_POINT('Ctrl Pts',(0.202545773298689,-0.12089201855432,
-0.243896910777748));
#51670=CARTESIAN_POINT('Ctrl Pts',(0.211271315496057,0.10490046033926,-0.231177637956761));
#51671=CARTESIAN_POINT('Ctrl Pts',(0.0261212881376767,0.234429852510476,
-0.218458365135776));
#51672=CARTESIAN_POINT('Ctrl Pts',(-0.182999181298496,0.148831968805373,
-0.20573909231479));
#51673=CARTESIAN_POINT('Ctrl Pts',(-0.224188466684687,-0.0733431981456951,
-0.193019819493804));
#51674=CARTESIAN_POINT('Ctrl Pts',(-0.0596484344001499,-0.228214284403755,
-0.180300546672818));
#51675=CARTESIAN_POINT('Ctrl Pts',(0.159628272860435,-0.173661646916563,
-0.167581273851832));
#51676=CARTESIAN_POINT('Ctrl Pts',(0.232421018722115,0.0402530640696309,
-0.154862001030846));
#51677=CARTESIAN_POINT('Ctrl Pts',(0.0919285295363725,0.217230088081641,
-0.14214272820986));
#51678=CARTESIAN_POINT('Ctrl Pts',(-0.132920504851494,0.194861535061435,
-0.129423455388874));
#51679=CARTESIAN_POINT('Ctrl Pts',(-0.235798703843206,-0.00632031137431454,
-0.116704182567888));
#51680=CARTESIAN_POINT('Ctrl Pts',(-0.122283640616722,-0.201709157150624,
-0.103984909746902));
#51681=CARTESIAN_POINT('Ctrl Pts',(0.10342756844873,-0.21198412740384,-0.091265636925916));
#51682=CARTESIAN_POINT('Ctrl Pts',(0.234263184552909,-0.0277545195405686,
-0.0785463641049296));
#51683=CARTESIAN_POINT('Ctrl Pts',(0.150056069810251,0.181992167351128,
-0.0658270912839439));
#51684=CARTESIAN_POINT('Ctrl Pts',(-0.0717210418700825,0.224640263091484,
-0.0531078184629578));
#51685=CARTESIAN_POINT('Ctrl Pts',(-0.227933705557797,0.0613210400915578,
-0.040388545641972));
#51686=CARTESIAN_POINT('Ctrl Pts',(-0.174482868217891,-0.158625442429202,
-0.0276692728209859));
#51687=CARTESIAN_POINT('Ctrl Pts',(-0.0328441439546209,-0.207662155862942,
-0.0191897576069953));
#51688=CARTESIAN_POINT('Ctrl Pts',(0.0326814423280684,-0.196779569448551,
-0.01495));
#51689=CARTESIAN_POINT('Ctrl Pts',(-0.0698093673657081,-0.202998596068489,
-1.53249182567888));
#51690=CARTESIAN_POINT('Ctrl Pts',(-0.00221290875353342,-0.226244402213306,
-1.52825206807188));
#51691=CARTESIAN_POINT('Ctrl Pts',(0.156854555777397,-0.199487415039017,
-1.51977255285789));
#51692=CARTESIAN_POINT('Ctrl Pts',(0.252840866551755,0.0243896328951931,
-1.50705328003691));
#51693=CARTESIAN_POINT('Ctrl Pts',(0.116213437351133,0.225596998424227,
-1.49433400721592));
#51694=CARTESIAN_POINT('Ctrl Pts',(-0.126760523989183,0.219925051861978,
-1.48161473439493));
#51695=CARTESIAN_POINT('Ctrl Pts',(-0.253566231042706,0.0123626962904411,
-1.46889546157395));
#51696=CARTESIAN_POINT('Ctrl Pts',(-0.147602816551325,-0.2065058897154,
-1.45617618875296));
#51697=CARTESIAN_POINT('Ctrl Pts',(0.0937674367161456,-0.235892193285902,
-1.44345691593198));
#51698=CARTESIAN_POINT('Ctrl Pts',(0.249113267698544,-0.0487987234249642,
-1.43073764311099));
#51699=CARTESIAN_POINT('Ctrl Pts',(0.175845736571276,0.183069889272311,
-1.41801837029));
#51700=CARTESIAN_POINT('Ctrl Pts',(-0.0587824954251087,0.24694524333112,
-1.40529909746902));
#51701=CARTESIAN_POINT('Ctrl Pts',(-0.239471525754721,0.084206937546123,
-1.39257982464803));
#51702=CARTESIAN_POINT('Ctrl Pts',(-0.200405077009279,-0.155804023890208,
-1.37986055182705));
#51703=CARTESIAN_POINT('Ctrl Pts',(0.0225644946070967,-0.252840062191573,
-1.36714127900606));
#51704=CARTESIAN_POINT('Ctrl Pts',(0.224827965993676,-0.117854303398096,
-1.35442200618508));
#51705=CARTESIAN_POINT('Ctrl Pts',(0.220775237476226,0.125281689063758,
-1.34170273336409));
#51706=CARTESIAN_POINT('Ctrl Pts',(0.0141257149141647,0.253451567217642,
-1.3289834605431));
#51707=CARTESIAN_POINT('Ctrl Pts',(-0.205486498938039,0.149038683086135,
-1.31626418772212));
#51708=CARTESIAN_POINT('Ctrl Pts',(-0.236531640785584,-0.0921412368862326,
-1.30354491490113));
#51709=CARTESIAN_POINT('Ctrl Pts',(-0.0505208349581985,-0.248766705486787,
-1.29082564208014));
#51710=CARTESIAN_POINT('Ctrl Pts',(0.181851002795451,-0.177108556133318,
-1.27810636925916));
#51711=CARTESIAN_POINT('Ctrl Pts',(0.247345182238226,0.0570752835595998,
-1.26538709643817));
#51712=CARTESIAN_POINT('Ctrl Pts',(0.0858602281027615,0.238883337590998,
-1.25266782361719));
#51713=CARTESIAN_POINT('Ctrl Pts',(-0.154415348051328,0.201477363243982,
-1.2399485507962));
#51714=CARTESIAN_POINT('Ctrl Pts',(-0.252989912722593,-0.020816618156529,
-1.22722927797522));
#51715=CARTESIAN_POINT('Ctrl Pts',(-0.119405390013515,-0.224007991934886,
-1.21451000515423));
#51716=CARTESIAN_POINT('Ctrl Pts',(0.123752855114802,-0.221635869030513,
-1.20179073233324));
#51717=CARTESIAN_POINT('Ctrl Pts',(0.253347876832675,-0.0158770553122787,
-1.18907145951226));
#51718=CARTESIAN_POINT('Ctrl Pts',(0.15045532097779,0.204451519882976,-1.17635218669127));
#51719=CARTESIAN_POINT('Ctrl Pts',(-0.0905042815017902,0.237162818794389,
-1.16363291387028));
#51720=CARTESIAN_POINT('Ctrl Pts',(-0.248411594622011,0.0522389437600805,
-1.1509136410493));
#51721=CARTESIAN_POINT('Ctrl Pts',(-0.178361165966253,-0.180622595664678,
-1.13819436822831));
#51722=CARTESIAN_POINT('Ctrl Pts',(0.0553644272025067,-0.247733743743779,
-1.12547509540733));
#51723=CARTESIAN_POINT('Ctrl Pts',(0.238284220344061,-0.0875091876533035,
-1.11275582258634));
#51724=CARTESIAN_POINT('Ctrl Pts',(0.202539772572176,0.153019175645918,
-1.10003654976536));
#51725=CARTESIAN_POINT('Ctrl Pts',(-0.0190676146789165,0.253127741781273,
-1.08731727694437));
#51726=CARTESIAN_POINT('Ctrl Pts',(-0.223177387174513,0.120950739736435,
-1.07459800412338));
#51727=CARTESIAN_POINT('Ctrl Pts',(-0.222485877045032,-0.122218092377381,
-1.0618787313024));
#51728=CARTESIAN_POINT('Ctrl Pts',(-0.0176276564718308,-0.253232093772011,
-1.04915945848141));
#51729=CARTESIAN_POINT('Ctrl Pts',(0.203406784733772,-0.151864767188167,
-1.03644018566043));
#51730=CARTESIAN_POINT('Ctrl Pts',(0.237782662831572,0.0888630004308762,
-1.02372091283944));
#51731=CARTESIAN_POINT('Ctrl Pts',(0.053954560004209,0.248044619057944,
-1.01100164001845));
#51732=CARTESIAN_POINT('Ctrl Pts',(-0.179385562083873,0.179605255225736,
-0.998282367197467));
#51733=CARTESIAN_POINT('Ctrl Pts',(-0.248110470846155,-0.0536509258573303,
-0.98556309437648));
#51734=CARTESIAN_POINT('Ctrl Pts',(-0.0891539675023196,-0.237673721028313,
-0.972843821555496));
#51735=CARTESIAN_POINT('Ctrl Pts',(0.151615694095433,-0.203592506966266,
-0.960124548734509));
#51736=CARTESIAN_POINT('Ctrl Pts',(0.253253479431093,0.0173177003350314,
-0.947405275913524));
#51737=CARTESIAN_POINT('Ctrl Pts',(0.122490311993534,0.222336121798901,
-0.934686003092538));
#51738=CARTESIAN_POINT('Ctrl Pts',(-0.120677491608289,0.22332525743404,
-0.92196673027155));
#51739=CARTESIAN_POINT('Ctrl Pts',(-0.253104214412132,0.0193774156085542,
-0.909247457450568));
#51740=CARTESIAN_POINT('Ctrl Pts',(-0.15326695919509,-0.202352333339499,
-0.896528184629577));
#51741=CARTESIAN_POINT('Ctrl Pts',(0.087217474594219,-0.238391148565243,
-0.883808911808594));
#51742=CARTESIAN_POINT('Ctrl Pts',(0.24766579500138,-0.0556675989708875,
-0.871089638987607));
#51743=CARTESIAN_POINT('Ctrl Pts',(0.180840765178744,0.17813995969017,-0.858370366166622));
#51744=CARTESIAN_POINT('Ctrl Pts',(-0.0519348617381085,0.248475346312451,
-0.845651093345635));
#51745=CARTESIAN_POINT('Ctrl Pts',(-0.237051868614696,0.0907944886825747,
-0.83293182052465));
#51746=CARTESIAN_POINT('Ctrl Pts',(-0.204635516239977,-0.150204970230839,
-0.820212547703662));
#51747=CARTESIAN_POINT('Ctrl Pts',(0.0155669587666708,-0.253367119776039,
-0.807493274882678));
#51748=CARTESIAN_POINT('Ctrl Pts',(0.22148423596564,-0.124024033185368,
-0.794774002061692));
#51749=CARTESIAN_POINT('Ctrl Pts',(0.224153970116863,0.119131126367953,
-0.782054729240706));
#51750=CARTESIAN_POINT('Ctrl Pts',(0.0211262491330936,0.252964244877444,
-0.769335456419719));
#51751=CARTESIAN_POINT('Ctrl Pts',(-0.201288216064753,0.154661830010893,
-0.756616183598734));
#51752=CARTESIAN_POINT('Ctrl Pts',(-0.238988246931607,-0.0855677825902145,
-0.743896910777748));
#51753=CARTESIAN_POINT('Ctrl Pts',(-0.0573779788313004,-0.247275140550125,
-0.731177637956761));
#51754=CARTESIAN_POINT('Ctrl Pts',(0.176885847982398,-0.182067636806757,
-0.718458365135776));
#51755=CARTESIAN_POINT('Ctrl Pts',(0.248828352713755,0.0502163168164291,
-0.705739092314789));
#51756=CARTESIAN_POINT('Ctrl Pts',(0.0924306728301907,0.236418692807924,
-0.693019819493804));
#51757=CARTESIAN_POINT('Ctrl Pts',(-0.148787071438908,0.205668750571112,
-0.680300546672817));
#51758=CARTESIAN_POINT('Ctrl Pts',(-0.253468657387831,-0.0138154736024218,
-0.667581273851832));
#51759=CARTESIAN_POINT('Ctrl Pts',(-0.125551830049769,-0.220621770367303,
-0.654862001030845));
#51760=CARTESIAN_POINT('Ctrl Pts',(0.117579070522484,-0.224971975507879,
-0.64214272820986));
#51761=CARTESIAN_POINT('Ctrl Pts',(0.25281219185396,-0.0228740735079175,
-0.629423455388874));
#51762=CARTESIAN_POINT('Ctrl Pts',(0.156049313005971,0.200214483739847,
-0.616704182567888));
#51763=CARTESIAN_POINT('Ctrl Pts',(-0.0839140032206536,0.239573929408717,
-0.603984909746902));
#51764=CARTESIAN_POINT('Ctrl Pts',(-0.246872674364797,0.0590856178847445,
-0.591265636925916));
#51765=CARTESIAN_POINT('Ctrl Pts',(-0.183285811505085,-0.175623286866439,
-0.57854636410493));
#51766=CARTESIAN_POINT('Ctrl Pts',(0.0484953731830222,-0.249169473187805,
-0.565827091283944));
#51767=CARTESIAN_POINT('Ctrl Pts',(0.235774223853273,-0.0940624417886129,
-0.553107818462958));
#51768=CARTESIAN_POINT('Ctrl Pts',(0.206692160604566,0.147362065449236,
-0.540388545641972));
#51769=CARTESIAN_POINT('Ctrl Pts',(-0.0120633285064898,0.253558087416263,
-0.527669272820986));
#51770=CARTESIAN_POINT('Ctrl Pts',(-0.219748766201783,0.127073629607583,
-0.51495));
#51771=CARTESIAN_POINT('Ctrl Pts',(-0.225779234532946,-0.116021398209831,
-0.502230727179014));
#51772=CARTESIAN_POINT('Ctrl Pts',(-0.024620805243708,-0.252648062604875,
-0.489511454358028));
#51773=CARTESIAN_POINT('Ctrl Pts',(0.199131187654392,-0.157429341903644,
-0.476792181537042));
#51774=CARTESIAN_POINT('Ctrl Pts',(0.2401481680199,0.0822562154825955,-0.464072908716056));
#51775=CARTESIAN_POINT('Ctrl Pts',(0.0607904345615275,0.246458415670172,
-0.45135363589507));
#51776=CARTESIAN_POINT('Ctrl Pts',(-0.174352336651932,0.18449523108459,
-0.438634363074084));
#51777=CARTESIAN_POINT('Ctrl Pts',(-0.249498691439802,-0.0467721130434017,
-0.425915090253098));
#51778=CARTESIAN_POINT('Ctrl Pts',(-0.0956897176127717,-0.235118492535058,
-0.413195817432112));
#51779=CARTESIAN_POINT('Ctrl Pts',(0.145930020331997,-0.207705697455295,
-0.400476544611126));
#51780=CARTESIAN_POINT('Ctrl Pts',(0.253635405587391,0.0103106071760593,
-0.38775727179014));
#51781=CARTESIAN_POINT('Ctrl Pts',(0.128589359170113,0.218865265167579,
-0.375037998969154));
#51782=CARTESIAN_POINT('Ctrl Pts',(-0.114458183843801,0.226575708636578,
-0.362318726148168));
#51783=CARTESIAN_POINT('Ctrl Pts',(-0.252471864955808,0.0263663608931849,
-0.349599453327182));
#51784=CARTESIAN_POINT('Ctrl Pts',(-0.158801850810788,-0.198038379535493,
-0.336880180506196));
#51785=CARTESIAN_POINT('Ctrl Pts',(0.0805944986169714,-0.240710935371991,
-0.32416090768521));
#51786=CARTESIAN_POINT('Ctrl Pts',(0.246032384154468,-0.0624923473565169,
-0.311441634864224));
#51787=CARTESIAN_POINT('Ctrl Pts',(0.185695837964635,0.173073057915355,
-0.298722362043239));
#51788=CARTESIAN_POINT('Ctrl Pts',(-0.0450466190763633,0.249815991998634,
-0.286003089222252));
#51789=CARTESIAN_POINT('Ctrl Pts',(-0.234451529484512,0.0973124220859982,
-0.273283816401267));
#51790=CARTESIAN_POINT('Ctrl Pts',(-0.208709314026801,-0.14449100356701,
-0.26056454358028));
#51791=CARTESIAN_POINT('Ctrl Pts',(0.00855739584547627,-0.25370060997161,
-0.247845270759295));
#51792=CARTESIAN_POINT('Ctrl Pts',(0.217971304682049,-0.130098942973611,
-0.235125997938309));
#51793=CARTESIAN_POINT('Ctrl Pts',(0.227361368892445,0.112889495690325,
-0.222406725117322));
#51794=CARTESIAN_POINT('Ctrl Pts',(0.0281106396969799,0.252283619529175,
-0.209687452296337));
#51795=CARTESIAN_POINT('Ctrl Pts',(-0.196936078466359,0.160166750905562,
-0.196968179475351));
#51796=CARTESIAN_POINT('Ctrl Pts',(-0.241262267694262,-0.0789288876731861,
-0.184248906654365));
#51797=CARTESIAN_POINT('Ctrl Pts',(-0.0641911547039274,-0.245594684640545,
-0.171529633833379));
#51798=CARTESIAN_POINT('Ctrl Pts',(0.171785282570279,-0.186887413818386,
-0.158810361012393));
#51799=CARTESIAN_POINT('Ctrl Pts',(0.250121796477491,0.0433186669354408,
-0.146091088191407));
#51800=CARTESIAN_POINT('Ctrl Pts',(0.0989296453547647,0.233773951162762,
-0.133371815370421));
#51801=CARTESIAN_POINT('Ctrl Pts',(-0.143043497722123,0.209701848317776,
-0.120652542549435));
#51802=CARTESIAN_POINT('Ctrl Pts',(-0.253756720182186,-0.00680165522004821,
-0.107933269728449));
#51803=CARTESIAN_POINT('Ctrl Pts',(-0.131596548535188,-0.217070973313282,
-0.0952139969074629));
#51804=CARTESIAN_POINT('Ctrl Pts',(0.111304430932834,-0.228128467306803,
-0.0824947240864769));
#51805=CARTESIAN_POINT('Ctrl Pts',(0.25210425843184,-0.0298682551432968,
-0.0697754512654907));
#51806=CARTESIAN_POINT('Ctrl Pts',(0.161484077299248,0.195852372100306,
-0.0570561784445048));
#51807=CARTESIAN_POINT('Ctrl Pts',(-0.0771831908164463,0.241748472124187,
-0.0443369056235189));
#51808=CARTESIAN_POINT('Ctrl Pts',(-0.245292737401046,0.0659911431156193,
-0.0316176328025329));
#51809=CARTESIAN_POINT('Ctrl Pts',(-0.187771177895848,-0.170706078329624,
-0.018898359981547));
#51810=CARTESIAN_POINT('Ctrl Pts',(-0.0353454964394484,-0.223477341982261,
-0.0104188447675563));
#51811=CARTESIAN_POINT('Ctrl Pts',(0.0351704037419476,-0.211765956844829,
-0.006179087160561));
#51812=CARTESIAN_POINT('Ctrl Pts',(-0.0747496809024987,-0.217364529322869,
-1.52372091283944));
#51813=CARTESIAN_POINT('Ctrl Pts',(-0.00236951328217214,-0.2422554094041,
-1.51948115523244));
#51814=CARTESIAN_POINT('Ctrl Pts',(0.167954938354344,-0.213604866809831,
-1.51100164001845));
#51815=CARTESIAN_POINT('Ctrl Pts',(0.270734069180786,0.0261156538877355,
-1.49828236719747));
#51816=CARTESIAN_POINT('Ctrl Pts',(0.124437703511504,0.241562189733518,
-1.48556309437648));
#51817=CARTESIAN_POINT('Ctrl Pts',(-0.135731193058758,0.235488847263547,
-1.47284382155549));
#51818=CARTESIAN_POINT('Ctrl Pts',(-0.271510766725581,0.0132375874137922,
-1.46012454873451));
#51819=CARTESIAN_POINT('Ctrl Pts',(-0.158048466185375,-0.221120029348596,
-1.44740527591352));
#51820=CARTESIAN_POINT('Ctrl Pts',(0.100403230083129,-0.252585961467587,
-1.43468600309254));
#51821=CARTESIAN_POINT('Ctrl Pts',(0.266742673250346,-0.0522521424002653,
-1.42196673027155));
#51822=CARTESIAN_POINT('Ctrl Pts',(0.188290099062327,0.196025495178498,
-1.40924745745057));
#51823=CARTESIAN_POINT('Ctrl Pts',(-0.062942452302435,0.264421220760959,
-1.39652818462958));
#51824=CARTESIAN_POINT('Ctrl Pts',(-0.25641859840421,0.0901661474508833,
-1.38380891180859));
#51825=CARTESIAN_POINT('Ctrl Pts',(-0.21458747046378,-0.166830061761007,
-1.37108963898761));
#51826=CARTESIAN_POINT('Ctrl Pts',(0.0241613530569681,-0.270733207897134,
-1.35837036616662));
#51827=CARTESIAN_POINT('Ctrl Pts',(0.240738733928709,-0.126194691406434,
-1.34565109334564));
#51828=CARTESIAN_POINT('Ctrl Pts',(0.236399199351971,0.134147703006429,
-1.33293182052465));
#51829=CARTESIAN_POINT('Ctrl Pts',(0.0151253724564228,0.2713879882983,-1.32021254770366));
#51830=CARTESIAN_POINT('Ctrl Pts',(-0.220028497678877,0.1595859470328,-1.30749327488268));
#51831=CARTESIAN_POINT('Ctrl Pts',(-0.253270661793043,-0.0986619463133894,
-1.29477400206169));
#51832=CARTESIAN_POINT('Ctrl Pts',(-0.0540961254135104,-0.266371585304427,
-1.28205472924071));
#51833=CARTESIAN_POINT('Ctrl Pts',(0.194720349771229,-0.189642286639183,
-1.26933545641972));
#51834=CARTESIAN_POINT('Ctrl Pts',(0.264849462798021,0.0611144233860401,
-1.25661618359873));
#51835=CARTESIAN_POINT('Ctrl Pts',(0.0919364391210603,0.255788784967876,
-1.24389691077775));
#51836=CARTESIAN_POINT('Ctrl Pts',(-0.165343111230579,0.215735640930078,
-1.23117763795676));
#51837=CARTESIAN_POINT('Ctrl Pts',(-0.270893663145469,-0.0222897817783964,
-1.21845836513578));
#51838=CARTESIAN_POINT('Ctrl Pts',(-0.127855546302129,-0.23986073142624,
-1.20573909231479));
#51839=CARTESIAN_POINT('Ctrl Pts',(0.132510675567995,-0.237320736625336,
-1.1930198194938));
#51840=CARTESIAN_POINT('Ctrl Pts',(0.271276959886478,-0.0170006528213758,
-1.18030054667282));
#51841=CARTESIAN_POINT('Ctrl Pts',(0.161102838452268,0.218920274570346,
-1.16758127385183));
#51842=CARTESIAN_POINT('Ctrl Pts',(-0.0969091458332232,0.253946507407051,
-1.15486200103085));
#51843=CARTESIAN_POINT('Ctrl Pts',(-0.265991343728995,0.0559358224275761,
-1.14214272820986));
#51844=CARTESIAN_POINT('Ctrl Pts',(-0.190983541958354,-0.193405009946382,
-1.12942345538888));
#51845=CARTESIAN_POINT('Ctrl Pts',(0.0592824920623715,-0.265265522270368,
-1.11670418256789));
#51846=CARTESIAN_POINT('Ctrl Pts',(0.255147269012042,-0.093702093285758,
-1.1039849097469));
#51847=CARTESIAN_POINT('Ctrl Pts',(0.216873235514688,0.163848133611853,
-1.09126563692592));
#51848=CARTESIAN_POINT('Ctrl Pts',(-0.0204170037146158,0.271041246178294,
-1.07854636410493));
#51849=CARTESIAN_POINT('Ctrl Pts',(-0.238971345901963,0.129510258313282,
-1.06582709128394));
#51850=CARTESIAN_POINT('Ctrl Pts',(-0.238230898545541,-0.130867299768838,
-1.05310781846296));
#51851=CARTESIAN_POINT('Ctrl Pts',(-0.0188751416328633,-0.271152983016823,
-1.04038854564197));
#51852=CARTESIAN_POINT('Ctrl Pts',(0.21780160494222,-0.162612029245002,
-1.02766927282099));
#51853=CARTESIAN_POINT('Ctrl Pts',(0.254610216959755,0.0951517135436653,
-1.01495));
#51854=CARTESIAN_POINT('Ctrl Pts',(0.0577728504889806,0.265598397805716,
-1.00223072717901));
#51855=CARTESIAN_POINT('Ctrl Pts',(-0.192080433189419,0.192315673714733,
-0.989511454358027));
#51856=CARTESIAN_POINT('Ctrl Pts',(-0.265668909834996,-0.0574477285684278,
-0.976792181537043));
#51857=CARTESIAN_POINT('Ctrl Pts',(-0.0954632719571637,-0.254493565493941,
-0.964072908716056));
#51858=CARTESIAN_POINT('Ctrl Pts',(0.162345329589841,-0.218000470483329,
-0.95135363589507));
#51859=CARTESIAN_POINT('Ctrl Pts',(0.271175882109777,0.0185432503238013,
-0.938634363074085));
#51860=CARTESIAN_POINT('Ctrl Pts',(0.131158783995253,0.238070545325274,
-0.925915090253097));
#51861=CARTESIAN_POINT('Ctrl Pts',(-0.129217672788485,0.2391296807377,-0.913195817432114));
#51862=CARTESIAN_POINT('Ctrl Pts',(-0.271016053809387,0.0207487288327176,
-0.900476544611126));
#51863=CARTESIAN_POINT('Ctrl Pts',(-0.164113452464216,-0.21667253146364,
-0.887757271790141));
#51864=CARTESIAN_POINT('Ctrl Pts',(0.0933897360920922,-0.255261764397326,
-0.875037998969154));
#51865=CARTESIAN_POINT('Ctrl Pts',(0.265192764888317,-0.0596071188825326,
-0.862318726148169));
#51866=CARTESIAN_POINT('Ctrl Pts',(0.193638619018841,0.190746681216378,
-0.849599453327181));
#51867=CARTESIAN_POINT('Ctrl Pts',(-0.0556102209364207,0.266059607039455,
-0.836880180506197));
#51868=CARTESIAN_POINT('Ctrl Pts',(-0.253827705434749,0.097219890579639,
-0.82416090768521));
#51869=CARTESIAN_POINT('Ctrl Pts',(-0.21911729209811,-0.160834770725045,
-0.811441634864225));
#51870=CARTESIAN_POINT('Ctrl Pts',(0.0166686111669654,-0.27129756462665,
-0.798722362043238));
#51871=CARTESIAN_POINT('Ctrl Pts',(0.237158372695661,-0.132801044540064,
-0.786003089222253));
#51872=CARTESIAN_POINT('Ctrl Pts',(0.240017040284684,0.127561873393136,
-0.773283816401267));
#51873=CARTESIAN_POINT('Ctrl Pts',(0.0226213249160781,0.270866178821993,
-0.76056454358028));
#51874=CARTESIAN_POINT('Ctrl Pts',(-0.215533108063434,0.165607036381619,
-0.747845270759295));
#51875=CARTESIAN_POINT('Ctrl Pts',(-0.255901118599167,-0.0916232976392016,
-0.735125997938309));
#51876=CARTESIAN_POINT('Ctrl Pts',(-0.0614385399885019,-0.26477446435536,
-0.722406725117323));
#51877=CARTESIAN_POINT('Ctrl Pts',(0.189403817736741,-0.194952314675497,
-0.709687452296337));
#51878=CARTESIAN_POINT('Ctrl Pts',(0.26643759522141,0.0537700569389561,
-0.69696817947535));
#51879=CARTESIAN_POINT('Ctrl Pts',(0.0989718652436024,0.253149720641341,
-0.684248906654365));
#51880=CARTESIAN_POINT('Ctrl Pts',(-0.159316529173112,0.220223647010986,
-0.671529633833378));
#51881=CARTESIAN_POINT('Ctrl Pts',(-0.271406287916481,-0.0147931757909765,
-0.658810361012393));
#51882=CARTESIAN_POINT('Ctrl Pts',(-0.134436961500886,-0.236234871585454,
-0.646091088191406));
#51883=CARTESIAN_POINT('Ctrl Pts',(0.125899980676306,-0.240892934799451,
-0.633371815370422));
#51884=CARTESIAN_POINT('Ctrl Pts',(0.270703365213811,-0.0244928404335767,
-0.620652542549433));
#51885=CARTESIAN_POINT('Ctrl Pts',(0.167092709652319,0.214383389169106,
-0.60793326972845));
#51886=CARTESIAN_POINT('Ctrl Pts',(-0.0898524825634798,0.256528249024871,
-0.595213996907462));
#51887=CARTESIAN_POINT('Ctrl Pts',(-0.26434351618805,0.0632670263243382,
-0.582494724086477));
#51888=CARTESIAN_POINT('Ctrl Pts',(-0.196256697932639,-0.188051906895844,
-0.569775451265491));
#51889=CARTESIAN_POINT('Ctrl Pts',(0.051927324476213,-0.266802856325281,
-0.557056178444504));
#51890=CARTESIAN_POINT('Ctrl Pts',(0.25245964349941,-0.100719112261466,
-0.544336905623519));
#51891=CARTESIAN_POINT('Ctrl Pts',(0.22131948237406,0.157790677456764,-0.531617632802532));
#51892=CARTESIAN_POINT('Ctrl Pts',(-0.0129170337808407,0.271502046785822,
-0.518898359981547));
#51893=CARTESIAN_POINT('Ctrl Pts',(-0.235300086108064,0.136066456733929,
-0.506179087160561));
#51894=CARTESIAN_POINT('Ctrl Pts',(-0.241757322442635,-0.124232074022583,
-0.493459814339575));
#51895=CARTESIAN_POINT('Ctrl Pts',(-0.0263631859874709,-0.270527620762044,
-0.480740541518589));
#51896=CARTESIAN_POINT('Ctrl Pts',(0.213223429699964,-0.168570401309326,
-0.468021268697603));
#51897=CARTESIAN_POINT('Ctrl Pts',(0.257143125717892,0.0880773754524993,
-0.455301995876617));
#51898=CARTESIAN_POINT('Ctrl Pts',(0.0650924905477743,0.263899940971675,
-0.442582723055631));
#51899=CARTESIAN_POINT('Ctrl Pts',(-0.186691013271359,0.197551706483163,
-0.429863450234646));
#51900=CARTESIAN_POINT('Ctrl Pts',(-0.267155372903108,-0.050082111571277,
-0.417144177413658));
#51901=CARTESIAN_POINT('Ctrl Pts',(-0.102461548172094,-0.251757506971836,
-0.404424904592674));
#51902=CARTESIAN_POINT('Ctrl Pts',(0.156257288463409,-0.222404745842757,
-0.391705631771687));
#51903=CARTESIAN_POINT('Ctrl Pts',(0.271584836658268,0.0110402747568785,
-0.378986358950701));
#51904=CARTESIAN_POINT('Ctrl Pts',(0.137689452406416,0.234354060912939,
-0.366267086129715));
#51905=CARTESIAN_POINT('Ctrl Pts',(-0.122558233111938,0.242610161930231,
-0.353547813308729));
#51906=CARTESIAN_POINT('Ctrl Pts',(-0.27033895384612,0.0282322722250301,
-0.340828540487743));
#51907=CARTESIAN_POINT('Ctrl Pts',(-0.170040040796351,-0.212053285043769,
-0.328109267666758));
#51908=CARTESIAN_POINT('Ctrl Pts',(0.0862980611549639,-0.257745719346492,
-0.315389994845771));
#51909=CARTESIAN_POINT('Ctrl Pts',(0.263443759787759,-0.0669148453856698,
-0.302670722024786));
#51910=CARTESIAN_POINT('Ctrl Pts',(0.198837278671528,0.185321201726677,
-0.289951449203799));
#51911=CARTESIAN_POINT('Ctrl Pts',(-0.0482345067540092,0.267495128388911,
-0.277232176382814));
#51912=CARTESIAN_POINT('Ctrl Pts',(-0.25104334385758,0.10419908922353,-0.264512903561827));
#51913=CARTESIAN_POINT('Ctrl Pts',(-0.223479386987627,-0.154716434448323,
-0.251793630740842));
#51914=CARTESIAN_POINT('Ctrl Pts',(0.00916299105612257,-0.27165465546766,
-0.239074357919855));
#51915=CARTESIAN_POINT('Ctrl Pts',(0.233396836065409,-0.139305867392902,
-0.22635508509887));
#51916=CARTESIAN_POINT('Ctrl Pts',(0.243451422288832,0.120878531041389,
-0.213635812277883));
#51917=CARTESIAN_POINT('Ctrl Pts',(0.0300999912562831,0.270137386547874,
-0.200916539456898));
#51918=CARTESIAN_POINT('Ctrl Pts',(-0.210872975634221,0.171501533005751,
-0.188197266635911));
#51919=CARTESIAN_POINT('Ctrl Pts',(-0.258336068703837,-0.084514577200677,
-0.175477993814926));
#51920=CARTESIAN_POINT('Ctrl Pts',(-0.068733875007705,-0.262975084877335,
-0.16275872099394));
#51921=CARTESIAN_POINT('Ctrl Pts',(0.183942292280123,-0.200113180720208,
-0.150039448172954));
#51922=CARTESIAN_POINT('Ctrl Pts',(0.267822574232866,0.0463842698012505,
-0.137320175351968));
#51923=CARTESIAN_POINT('Ctrl Pts',(0.105930761173157,0.250317814243884,
-0.124600902530982));
#51924=CARTESIAN_POINT('Ctrl Pts',(-0.153166490592751,0.224542161574117,
-0.111881629709996));
#51925=CARTESIAN_POINT('Ctrl Pts',(-0.271714736521166,-0.00728299906578173,
-0.0991623568890098));
#51926=CARTESIAN_POINT('Ctrl Pts',(-0.140909456453654,-0.232432789475941,
-0.0864430840680238));
#51927=CARTESIAN_POINT('Ctrl Pts',(0.119181293416937,-0.244272807209766,
-0.0737238112470379));
#51928=CARTESIAN_POINT('Ctrl Pts',(0.26994533231077,-0.0319819907460251,
-0.0610045384260516));
#51929=CARTESIAN_POINT('Ctrl Pts',(0.172912084788245,0.209712576849484,
-0.0482852656050659));
#51930=CARTESIAN_POINT('Ctrl Pts',(-0.0826453397628101,0.258856681156889,
-0.0355659927840798));
#51931=CARTESIAN_POINT('Ctrl Pts',(-0.262651769244295,0.0706612461396808,
-0.0228467199630939));
#51932=CARTESIAN_POINT('Ctrl Pts',(-0.201059487573804,-0.182786714230045,
-0.0101274471421079));
#51933=CARTESIAN_POINT('Ctrl Pts',(-0.0378468489242762,-0.23929252810158,
-0.00164793192811731));
#51934=CARTESIAN_POINT('Ctrl Pts',(0.0376593651558268,-0.226752344241108,
0.00259182567887802));
#51935=CARTESIAN_POINT('Ctrl Pts',(-0.0796899944392894,-0.231730462577249,
-1.51495));
#51936=CARTESIAN_POINT('Ctrl Pts',(-0.00252611781081108,-0.258266416594894,
-1.510710242393));
#51937=CARTESIAN_POINT('Ctrl Pts',(0.179055320931291,-0.227722318580645,
-1.50223072717901));
#51938=CARTESIAN_POINT('Ctrl Pts',(0.288627271809818,0.0278416748802775,
-1.48951145435803));
#51939=CARTESIAN_POINT('Ctrl Pts',(0.132661969671875,0.25752738104281,-1.47679218153704));
#51940=CARTESIAN_POINT('Ctrl Pts',(-0.144701862128332,0.251052642665116,
-1.46407290871606));
#51941=CARTESIAN_POINT('Ctrl Pts',(-0.289455302408456,0.0141124785371433,
-1.45135363589507));
#51942=CARTESIAN_POINT('Ctrl Pts',(-0.168494115819424,-0.235734168981793,
-1.43863436307408));
#51943=CARTESIAN_POINT('Ctrl Pts',(0.107039023450112,-0.269279729649273,
-1.4259150902531));
#51944=CARTESIAN_POINT('Ctrl Pts',(0.284372078802149,-0.0557055613755665,
-1.41319581743211));
#51945=CARTESIAN_POINT('Ctrl Pts',(0.200734461553377,0.208981101084686,
-1.40047654461112));
#51946=CARTESIAN_POINT('Ctrl Pts',(-0.0671024091797608,0.281897198190798,
-1.38775727179014));
#51947=CARTESIAN_POINT('Ctrl Pts',(-0.2733656710537,0.0961253573556439,
-1.37503799896915));
#51948=CARTESIAN_POINT('Ctrl Pts',(-0.22876986391828,-0.177856099631807,
-1.36231872614817));
#51949=CARTESIAN_POINT('Ctrl Pts',(0.0257582115068392,-0.288626353602694,
-1.34959945332718));
#51950=CARTESIAN_POINT('Ctrl Pts',(0.256649501863742,-0.134535079414771,
-1.3368801805062));
#51951=CARTESIAN_POINT('Ctrl Pts',(0.252023161227715,0.143013716949099,
-1.32416090768521));
#51952=CARTESIAN_POINT('Ctrl Pts',(0.0161250299986812,0.289324409378958,
-1.31144163486423));
#51953=CARTESIAN_POINT('Ctrl Pts',(-0.234570496419716,0.170133210979464,
-1.29872236204324));
#51954=CARTESIAN_POINT('Ctrl Pts',(-0.270009682800502,-0.105182655740546,
-1.28600308922225));
#51955=CARTESIAN_POINT('Ctrl Pts',(-0.0576714158688228,-0.283976465122066,
-1.27328381640127));
#51956=CARTESIAN_POINT('Ctrl Pts',(0.207589696747008,-0.202176017145047,
-1.26056454358028));
#51957=CARTESIAN_POINT('Ctrl Pts',(0.282353743357815,0.0651535632124803,
-1.2478452707593));
#51958=CARTESIAN_POINT('Ctrl Pts',(0.0980126501393592,0.272694232344753,
-1.23512599793831));
#51959=CARTESIAN_POINT('Ctrl Pts',(-0.176270874409831,0.229993918616173,
-1.22240672511732));
#51960=CARTESIAN_POINT('Ctrl Pts',(-0.288797413568345,-0.0237629454002635,
-1.20968745229634));
#51961=CARTESIAN_POINT('Ctrl Pts',(-0.136305702590742,-0.255713470917593,
-1.19696817947535));
#51962=CARTESIAN_POINT('Ctrl Pts',(0.141268496021188,-0.253005604220159,
-1.18424890665437));
#51963=CARTESIAN_POINT('Ctrl Pts',(0.289206042940281,-0.0181242503304727,
-1.17152963383338));
#51964=CARTESIAN_POINT('Ctrl Pts',(0.171750355926746,0.233389029257715,
-1.15881036101239));
#51965=CARTESIAN_POINT('Ctrl Pts',(-0.103314010164656,0.270730196019714,
-1.14609108819141));
#51966=CARTESIAN_POINT('Ctrl Pts',(-0.283571092835979,0.0596327010950711,
-1.13337181537042));
#51967=CARTESIAN_POINT('Ctrl Pts',(-0.203605917950455,-0.206187424228085,
-1.12065254254943));
#51968=CARTESIAN_POINT('Ctrl Pts',(0.0632005569222366,-0.282797300796956,
-1.10793326972845));
#51969=CARTESIAN_POINT('Ctrl Pts',(0.272010317680024,-0.0998949989182119,
-1.09521399690746));
#51970=CARTESIAN_POINT('Ctrl Pts',(0.2312066984572,0.174677091577786,-1.08249472408648));
#51971=CARTESIAN_POINT('Ctrl Pts',(-0.0217663927503151,0.288954750575316,
-1.06977545126549));
#51972=CARTESIAN_POINT('Ctrl Pts',(-0.254765304629413,0.138069776890128,
-1.0570561784445));
#51973=CARTESIAN_POINT('Ctrl Pts',(-0.25397592004605,-0.139516507160294,
-1.04433690562352));
#51974=CARTESIAN_POINT('Ctrl Pts',(-0.0201226267938958,-0.289073872261636,
-1.03161763280253));
#51975=CARTESIAN_POINT('Ctrl Pts',(0.232196425150669,-0.173359291301837,
-1.01889835998155));
#51976=CARTESIAN_POINT('Ctrl Pts',(0.271437771087937,0.101440426656454,
-1.00617908716056));
#51977=CARTESIAN_POINT('Ctrl Pts',(0.0615911409737527,0.283152176553489,
-0.993459814339575));
#51978=CARTESIAN_POINT('Ctrl Pts',(-0.204775304294965,0.205026092203729,
-0.980740541518589));
#51979=CARTESIAN_POINT('Ctrl Pts',(-0.283227348823837,-0.0612445312795246,
-0.968021268697604));
#51980=CARTESIAN_POINT('Ctrl Pts',(-0.101772576412007,-0.27131340995957,
-0.955301995876616));
#51981=CARTESIAN_POINT('Ctrl Pts',(0.173074965084248,-0.232408434000391,
-0.942582723055633));
#51982=CARTESIAN_POINT('Ctrl Pts',(0.28909828478846,0.0197688003125712,
-0.929863450234644));
#51983=CARTESIAN_POINT('Ctrl Pts',(0.139827255996971,0.253804968851647,
-0.91714417741366));
#51984=CARTESIAN_POINT('Ctrl Pts',(-0.137757853968682,0.25493410404136,
-0.904424904592673));
#51985=CARTESIAN_POINT('Ctrl Pts',(-0.288927893206643,0.0221200420568807,
-0.891705631771688));
#51986=CARTESIAN_POINT('Ctrl Pts',(-0.174959945733342,-0.230992729587781,
-0.8789863589507));
#51987=CARTESIAN_POINT('Ctrl Pts',(0.0995619975899653,-0.272132380229409,
-0.866267086129716));
#51988=CARTESIAN_POINT('Ctrl Pts',(0.282719734775254,-0.0635466387941777,
-0.853547813308729));
#51989=CARTESIAN_POINT('Ctrl Pts',(0.206436472858937,0.203353402742587,
-0.840828540487744));
#51990=CARTESIAN_POINT('Ctrl Pts',(-0.0592855801347328,0.283643867766458,
-0.828109267666757));
#51991=CARTESIAN_POINT('Ctrl Pts',(-0.270603542254802,0.103645292476704,
-0.815389994845772));
#51992=CARTESIAN_POINT('Ctrl Pts',(-0.233599067956243,-0.171464571219253,
-0.802670722024785));
#51993=CARTESIAN_POINT('Ctrl Pts',(0.0177702635672599,-0.28922800947726,
-0.7899514492038));
#51994=CARTESIAN_POINT('Ctrl Pts',(0.252832509425682,-0.14157805589476,
-0.777232176382813));
#51995=CARTESIAN_POINT('Ctrl Pts',(0.255880110452505,0.135992620418319,
-0.764512903561829));
#51996=CARTESIAN_POINT('Ctrl Pts',(0.0241164006990628,0.288768112766542,
-0.75179363074084));
#51997=CARTESIAN_POINT('Ctrl Pts',(-0.229778000062115,0.176552242752344,
-0.739074357919857));
#51998=CARTESIAN_POINT('Ctrl Pts',(-0.272813990266727,-0.0976788126881887,
-0.726355085098868));
#51999=CARTESIAN_POINT('Ctrl Pts',(-0.0654991011457034,-0.282273788160596,
-0.713635812277885));
#52000=CARTESIAN_POINT('Ctrl Pts',(0.201921787491083,-0.207836992544237,
-0.700916539456897));
#52001=CARTESIAN_POINT('Ctrl Pts',(0.284046837729065,0.0573237970614832,
-0.688197266635913));
#52002=CARTESIAN_POINT('Ctrl Pts',(0.105513057657014,0.269880748474758,
-0.675477993814925));
#52003=CARTESIAN_POINT('Ctrl Pts',(-0.169845986907316,0.23477854345086,
-0.662758720993941));
#52004=CARTESIAN_POINT('Ctrl Pts',(-0.289343918445131,-0.0157708779795308,
-0.650039448172953));
#52005=CARTESIAN_POINT('Ctrl Pts',(-0.143322092952003,-0.251847972803605,
-0.637320175351968));
#52006=CARTESIAN_POINT('Ctrl Pts',(0.134220890830127,-0.256813894091022,
-0.624600902530981));
#52007=CARTESIAN_POINT('Ctrl Pts',(0.288594538573662,-0.0261116073592364,
-0.611881629709995));
#52008=CARTESIAN_POINT('Ctrl Pts',(0.178136106298667,0.228552294598365,
-0.599162356889011));
#52009=CARTESIAN_POINT('Ctrl Pts',(-0.0957909619063059,0.273482568641024,
-0.586443084068023));
#52010=CARTESIAN_POINT('Ctrl Pts',(-0.281814358011304,0.0674484347639324,
-0.573723811247039));
#52011=CARTESIAN_POINT('Ctrl Pts',(-0.209227584360194,-0.20048052692525,
-0.561004538426051));
#52012=CARTESIAN_POINT('Ctrl Pts',(0.055359275769404,-0.284436239462757,
-0.548285265605067));
#52013=CARTESIAN_POINT('Ctrl Pts',(0.269145063145547,-0.107375782734319,
-0.535565992784079));
#52014=CARTESIAN_POINT('Ctrl Pts',(0.235946804143553,0.168219289464292,
-0.522846719963094));
#52015=CARTESIAN_POINT('Ctrl Pts',(-0.0137707390551913,0.289446006155381,
-0.510127447142108));
#52016=CARTESIAN_POINT('Ctrl Pts',(-0.250851406014347,0.145059283860275,
-0.497408174321121));
#52017=CARTESIAN_POINT('Ctrl Pts',(-0.257735410352323,-0.132442749835334,
-0.484688901500136));
#52018=CARTESIAN_POINT('Ctrl Pts',(-0.028105566731234,-0.288407178919214,
-0.471969628679149));
#52019=CARTESIAN_POINT('Ctrl Pts',(0.227315671745536,-0.179711460715009,
-0.459250355858164));
#52020=CARTESIAN_POINT('Ctrl Pts',(0.274138083415885,0.0938985354224031,
-0.446531083037178));
#52021=CARTESIAN_POINT('Ctrl Pts',(0.069394546534021,0.281341466273177,
-0.433811810216192));
#52022=CARTESIAN_POINT('Ctrl Pts',(-0.199029689890786,0.210608181881736,
-0.421092537395206));
#52023=CARTESIAN_POINT('Ctrl Pts',(-0.284812054366414,-0.0533921100991525,
-0.40837326457422));
#52024=CARTESIAN_POINT('Ctrl Pts',(-0.109233378731415,-0.268396521408613,
-0.395653991753234));
#52025=CARTESIAN_POINT('Ctrl Pts',(0.166584556594821,-0.237103794230219,
-0.382934718932248));
#52026=CARTESIAN_POINT('Ctrl Pts',(0.289534267729147,0.0117699423376978,
-0.370215446111262));
#52027=CARTESIAN_POINT('Ctrl Pts',(0.146789545642719,0.249842856658299,
-0.357496173290276));
#52028=CARTESIAN_POINT('Ctrl Pts',(-0.130658282380074,0.258644615223885,
-0.34477690046929));
#52029=CARTESIAN_POINT('Ctrl Pts',(-0.288206042736432,0.030098183556875,
-0.332057627648304));
#52030=CARTESIAN_POINT('Ctrl Pts',(-0.181278230781915,-0.226068190552044,
-0.319338354827318));
#52031=CARTESIAN_POINT('Ctrl Pts',(0.0920016236929569,-0.274780503320994,
-0.306619082006332));
#52032=CARTESIAN_POINT('Ctrl Pts',(0.28085513542105,-0.0713373434148228,
-0.293899809185346));
#52033=CARTESIAN_POINT('Ctrl Pts',(0.211978719378421,0.197569345537999,
-0.281180536364361));
#52034=CARTESIAN_POINT('Ctrl Pts',(-0.0514223944316555,0.285174264779187,
-0.268461263543374));
#52035=CARTESIAN_POINT('Ctrl Pts',(-0.267635158230649,0.111085756361062,
-0.255741990722389));
#52036=CARTESIAN_POINT('Ctrl Pts',(-0.238249459948454,-0.164941865329635,
-0.243022717901402));
#52037=CARTESIAN_POINT('Ctrl Pts',(0.00976858626676915,-0.28960870096371,
-0.230303445080417));
#52038=CARTESIAN_POINT('Ctrl Pts',(0.248822367448769,-0.148512791812193,
-0.217584172259431));
#52039=CARTESIAN_POINT('Ctrl Pts',(0.25954147568522,0.128867566392453,-0.204864899438444));
#52040=CARTESIAN_POINT('Ctrl Pts',(0.032089342815586,0.287991153566572,
-0.192145626617459));
#52041=CARTESIAN_POINT('Ctrl Pts',(-0.224809872802084,0.182836315105941,
-0.179426353796473));
#52042=CARTESIAN_POINT('Ctrl Pts',(-0.275409869713412,-0.0901002667281681,
-0.166707080975487));
#52043=CARTESIAN_POINT('Ctrl Pts',(-0.0732765953114828,-0.280355485114124,
-0.153987808154501));
#52044=CARTESIAN_POINT('Ctrl Pts',(0.196099301989967,-0.213338947622031,
-0.141268535333515));
#52045=CARTESIAN_POINT('Ctrl Pts',(0.285523351988242,0.0494498726670601,
-0.128549262512529));
#52046=CARTESIAN_POINT('Ctrl Pts',(0.112931876991549,0.266861677325006,
-0.115829989691543));
#52047=CARTESIAN_POINT('Ctrl Pts',(-0.16328948346338,0.239382474830457,
-0.103110716870557));
#52048=CARTESIAN_POINT('Ctrl Pts',(-0.289672752860146,-0.00776434291151507,
-0.0903914440495708));
#52049=CARTESIAN_POINT('Ctrl Pts',(-0.15022236437212,-0.2477946056386,-0.0776721712285848));
#52050=CARTESIAN_POINT('Ctrl Pts',(0.127058155901041,-0.260417147112729,
-0.0649528984075989));
#52051=CARTESIAN_POINT('Ctrl Pts',(0.2877864061897,-0.0340957263487534,
-0.0522336255866126));
#52052=CARTESIAN_POINT('Ctrl Pts',(0.184340092277242,0.223572781598662,
-0.0395143527656268));
#52053=CARTESIAN_POINT('Ctrl Pts',(-0.0881074887091739,0.275964890189591,
-0.0267950799446408));
#52054=CARTESIAN_POINT('Ctrl Pts',(-0.280010801087544,0.0753313491637424,
-0.0140758071236549));
#52055=CARTESIAN_POINT('Ctrl Pts',(-0.214347797251761,-0.194867350130467,
-0.00135653430266889));
#52056=CARTESIAN_POINT('Ctrl Pts',(-0.0403482014091038,-0.255107714220899,
0.00712298091132171));
#52057=CARTESIAN_POINT('Ctrl Pts',(0.0401483265697059,-0.241738731637386,
0.011362738518317));
#52058=CARTESIAN_POINT('Ctrl Pts',(-0.24544712988196,-4.00287140078511E-5,
-0.0907327496212059));
#52059=CARTESIAN_POINT('Ctrl Pts',(-0.245452120854431,-0.00221980312011781,
-0.0906189810973275));
#52060=CARTESIAN_POINT('Ctrl Pts',(-0.245425583143613,-0.00439945378707234,
-0.0905052125734492));
#52061=CARTESIAN_POINT('Ctrl Pts',(-0.24536714321268,-0.0065782504090337,
-0.0903914440495708));
#52062=CARTESIAN_POINT('Ctrl Pts',(-0.243189290030804,-0.0877744304872093,
-0.0861516864425755));
#52063=CARTESIAN_POINT('Ctrl Pts',(-0.196705827201461,-0.167784518062905,
-0.0819119288355801));
#52064=CARTESIAN_POINT('Ctrl Pts',(-0.127250675741264,-0.209893318763107,
-0.0776721712285849));
#52065=CARTESIAN_POINT('Ctrl Pts',(-0.0577955242810662,-0.25200211946331,
-0.0734324136215895));
#52066=CARTESIAN_POINT('Ctrl Pts',(0.0346313158099865,-0.256209633288019,
-0.0691926560145943));
#52067=CARTESIAN_POINT('Ctrl Pts',(0.10763277757029,-0.220593153406378,
-0.0649528984075989));
#52068=CARTESIAN_POINT('Ctrl Pts',(0.180634239330593,-0.184976673524737,
-0.0607131408006035));
#52069=CARTESIAN_POINT('Ctrl Pts',(0.234210322760147,-0.109536199936745,
-0.056473383193608));
#52070=CARTESIAN_POINT('Ctrl Pts',(0.24375731215618,-0.0288712118181801,
-0.0522336255866127));
#52071=CARTESIAN_POINT('Ctrl Pts',(0.253304301552214,0.0517937763003857,
-0.0479938679796173));
#52072=CARTESIAN_POINT('Ctrl Pts',(0.218822196914728,0.137683278949523,
-0.0437541103726222));
#52073=CARTESIAN_POINT('Ctrl Pts',(0.156173214431582,0.189360048372581,
-0.0395143527656269));
#52074=CARTESIAN_POINT('Ctrl Pts',(0.093524231948437,0.241036817795638,
-0.0352745951586316));
#52075=CARTESIAN_POINT('Ctrl Pts',(0.00270837161963094,0.258500853992614,
-0.0310348375516362));
#52076=CARTESIAN_POINT('Ctrl Pts',(-0.0746834439411661,0.233793948586794,
-0.0267950799446409));
#52077=CARTESIAN_POINT('Ctrl Pts',(-0.146756136718545,0.210785143458111,
-0.0228467199630937));
#52078=CARTESIAN_POINT('Ctrl Pts',(-0.20718663585062,0.151202989772472,
-0.0188983599815467));
#52079=CARTESIAN_POINT('Ctrl Pts',(-0.232146082211076,0.0797430227058862,
-0.0149499999999996));
#52080=CARTESIAN_POINT('',(0.197117931249732,0.0326679887445553,-1.51495));
#52081=CARTESIAN_POINT('Ctrl Pts',(0.197120364464142,0.0326678919976635,
-1.51495));
#52082=CARTESIAN_POINT('Ctrl Pts',(0.19839158954313,0.0282478473569942,
-1.51495));
#52083=CARTESIAN_POINT('Ctrl Pts',(0.19949723577291,0.0237887889107814,
-1.51495));
#52084=CARTESIAN_POINT('Ctrl Pts',(0.200432284720987,0.0192980969514664,
-1.51495));
#52085=CARTESIAN_POINT('Ctrl Pts',(0.202577213948768,0.00899680047248181,
-1.51495));
#52086=CARTESIAN_POINT('Ctrl Pts',(0.203826058329088,-0.00147033997848461,
-1.51495));
#52087=CARTESIAN_POINT('Ctrl Pts',(0.20423417638802,-0.01200912787121,-1.51495));
#52088=CARTESIAN_POINT('Ctrl Pts',(0.204460722409734,-0.0178592009530887,
-1.51495));
#52089=CARTESIAN_POINT('Ctrl Pts',(0.204427206594989,-0.0237345590497023,
-1.51495));
#52090=CARTESIAN_POINT('Ctrl Pts',(0.204142815235946,-0.0295947455656042,
-1.51495));
#52091=CARTESIAN_POINT('Ctrl Pts',(0.203701770180365,-0.038682948161926,
-1.51495));
#52092=CARTESIAN_POINT('Ctrl Pts',(0.202658993444603,-0.047746378507929,
-1.51495));
#52093=CARTESIAN_POINT('Ctrl Pts',(0.201046184074424,-0.0567275139665697,
-1.51495));
#52094=CARTESIAN_POINT('Ctrl Pts',(0.200183877514263,-0.0615293784440873,
-1.51495));
#52095=CARTESIAN_POINT('Ctrl Pts',(0.199158432739084,-0.0663077749781463,
-1.51495));
#52096=CARTESIAN_POINT('Ctrl Pts',(0.197973440998626,-0.0710540933796172,
-1.51495));
#52097=CARTESIAN_POINT('Ctrl Pts',(0.196939744036605,-0.0751944217421482,
-1.51495));
#52098=CARTESIAN_POINT('Ctrl Pts',(0.195785043563296,-0.0793077977796779,
-1.51495));
#52099=CARTESIAN_POINT('Ctrl Pts',(0.194515550626655,-0.0833781506086003,
-1.51495));
#52100=CARTESIAN_POINT('Ctrl Pts',(0.19033267790619,-0.0967896216923322,
-1.51495));
#52101=CARTESIAN_POINT('Ctrl Pts',(0.184899873663921,-0.109766099393497,
-1.51495));
#52102=CARTESIAN_POINT('Ctrl Pts',(0.178313994607811,-0.122111154788251,
-1.51495));
#52103=CARTESIAN_POINT('Ctrl Pts',(0.173663514747407,-0.130828355787502,
-1.51495));
#52104=CARTESIAN_POINT('Ctrl Pts',(0.168436916876066,-0.139231082048986,
-1.51495));
#52105=CARTESIAN_POINT('Ctrl Pts',(0.162653150682954,-0.147246871784982,
-1.51495));
#52106=CARTESIAN_POINT('Ctrl Pts',(0.160516541128603,-0.150208024148989,
-1.51495));
#52107=CARTESIAN_POINT('Ctrl Pts',(0.158305528707968,-0.153113639786799,
-1.51495));
#52108=CARTESIAN_POINT('Ctrl Pts',(0.156026676769085,-0.155953801417746,
-1.51495));
#52109=CARTESIAN_POINT('Ctrl Pts',(0.150504934476818,-0.162835617795061,
-1.51495));
#52110=CARTESIAN_POINT('Ctrl Pts',(0.144577160304343,-0.169344859396806,
-1.51495));
#52111=CARTESIAN_POINT('Ctrl Pts',(0.138263901802813,-0.175434489995263,
-1.51495));
#52112=CARTESIAN_POINT('Ctrl Pts',(0.131281509670573,-0.182169552208951,
-1.51495));
#52113=CARTESIAN_POINT('Ctrl Pts',(0.123827735071421,-0.188391742560213,
-1.51495));
#52114=CARTESIAN_POINT('Ctrl Pts',(0.115968478775398,-0.194097892548868,
-1.51495));
#52115=CARTESIAN_POINT('Ctrl Pts',(0.11169834481699,-0.197198189055378,
-1.51495));
#52116=CARTESIAN_POINT('Ctrl Pts',(0.107308328841664,-0.200146016980857,
-1.51495));
#52117=CARTESIAN_POINT('Ctrl Pts',(0.102807906095061,-0.202939831405905,
-1.51495));
#52118=CARTESIAN_POINT('Ctrl Pts',(0.0986064882257294,-0.205548026793295,
-1.51495));
#52119=CARTESIAN_POINT('Ctrl Pts',(0.0943066784205236,-0.208022722670441,
-1.51495));
#52120=CARTESIAN_POINT('Ctrl Pts',(0.0899371264991721,-0.210351864187837,
-1.51495));
#52121=CARTESIAN_POINT('Ctrl Pts',(0.0771241238284205,-0.217181694115504,
-1.51495));
#52122=CARTESIAN_POINT('Ctrl Pts',(0.0636786011257452,-0.222786608559561,
-1.51495));
#52123=CARTESIAN_POINT('Ctrl Pts',(0.0498091216440218,-0.227155802214754,
-1.51495));
#52124=CARTESIAN_POINT('Ctrl Pts',(0.0425067356028674,-0.229456215781162,
-1.51495));
#52125=CARTESIAN_POINT('Ctrl Pts',(0.0350861499587181,-0.23141347164588,
-1.51495));
#52126=CARTESIAN_POINT('Ctrl Pts',(0.0275745313202283,-0.233021485604181,
-1.51495));
#52127=CARTESIAN_POINT('Ctrl Pts',(0.0230174188518951,-0.233997027735816,
-1.51495));
#52128=CARTESIAN_POINT('Ctrl Pts',(0.0184267660685815,-0.234843966119456,
-1.51495));
#52129=CARTESIAN_POINT('Ctrl Pts',(0.0138084231203835,-0.235560309102908,
-1.51495));
#52130=CARTESIAN_POINT('Ctrl Pts',(0.00959330062632784,-0.236214109276883,
-1.51495));
#52131=CARTESIAN_POINT('Ctrl Pts',(0.0053639592813879,-0.236757676588111,
-1.51495));
#52132=CARTESIAN_POINT('Ctrl Pts',(0.00112882195410514,-0.237190325076065,
-1.51495));
#52133=CARTESIAN_POINT('Ctrl Pts',(-0.0140084176727373,-0.23873669850631,
-1.51495));
#52134=CARTESIAN_POINT('Ctrl Pts',(-0.029232575277218,-0.238871978685379,
-1.51495));
#52135=CARTESIAN_POINT('Ctrl Pts',(-0.0443347748320724,-0.237560860275706,
-1.51495));
#52136=CARTESIAN_POINT('Ctrl Pts',(-0.0562275106107457,-0.23652837591711,
-1.51495));
#52137=CARTESIAN_POINT('Ctrl Pts',(-0.0680455301589941,-0.234598198295124,
-1.51495));
#52138=CARTESIAN_POINT('Ctrl Pts',(-0.0796899944392881,-0.23173046257725,
-1.51495));
#52139=CARTESIAN_POINT('Ctrl Pts',(0.197120364464142,0.0326678919976615,
-1.51495));
#52140=CARTESIAN_POINT('Ctrl Pts',(0.186733145342478,0.0934018504203839,
-1.51100164001845));
#52141=CARTESIAN_POINT('Ctrl Pts',(0.102816589942559,0.209511059178545,
-1.50281352242991));
#52142=CARTESIAN_POINT('Ctrl Pts',(-0.117789854919609,0.204361256460409,
-1.49038564723437));
#52143=CARTESIAN_POINT('Ctrl Pts',(-0.19826172011417,0.0726406085090636,
-1.48169916992909));
#52144=CARTESIAN_POINT('Ctrl Pts',(-0.199801535574945,0.00328497078691713,
-1.47725245023081));
#52145=CARTESIAN_POINT('Ctrl Pts',(-0.199789055725603,5.64207037231446E-5,
-1.47704548813952));
#52146=CARTESIAN_POINT('Origin',(-5.69858952725515E-17,8.58067791224701E-18,
-1.51495));
#52147=CARTESIAN_POINT('',(0.0326814423280644,0.196779569448552,-1.51495));
#52148=CARTESIAN_POINT('Ctrl Pts',(-0.232146081401957,-0.0797429895224413,
-1.51495));
#52149=CARTESIAN_POINT('Ctrl Pts',(-0.233507180164754,-0.0743161098729126,
-1.51495));
#52150=CARTESIAN_POINT('Ctrl Pts',(-0.234667146884371,-0.0688472205568463,
-1.51495));
#52151=CARTESIAN_POINT('Ctrl Pts',(-0.235618161880822,-0.0633432983169081,
-1.51495));
#52152=CARTESIAN_POINT('Ctrl Pts',(-0.237412919419644,-0.0529562844737211,
-1.51495));
#52153=CARTESIAN_POINT('Ctrl Pts',(-0.238464190995544,-0.0424443441387855,
-1.51495));
#52154=CARTESIAN_POINT('Ctrl Pts',(-0.238796731864267,-0.031878682006575,
-1.51495));
#52155=CARTESIAN_POINT('Ctrl Pts',(-0.238949768024948,-0.0270163371947305,
-1.51495));
#52156=CARTESIAN_POINT('Ctrl Pts',(-0.238950418479618,-0.0221426391101435,
-1.51495));
#52157=CARTESIAN_POINT('Ctrl Pts',(-0.238800286344163,-0.0172647716021107,
-1.51495));
#52158=CARTESIAN_POINT('Ctrl Pts',(-0.23864300623783,-0.0121546629767112,
-1.51495));
#52159=CARTESIAN_POINT('Ctrl Pts',(-0.238320478407458,-0.00704904230179029,
-1.51495));
#52160=CARTESIAN_POINT('Ctrl Pts',(-0.237836107021191,-0.00195869766834203,
-1.51495));
#52161=CARTESIAN_POINT('Ctrl Pts',(-0.236971804892792,0.00712440638305752,
-1.51495));
#52162=CARTESIAN_POINT('Ctrl Pts',(-0.235592459223133,0.0161619095527178,
-1.51495));
#52163=CARTESIAN_POINT('Ctrl Pts',(-0.23371173453278,0.0251065661509408,
-1.51495));
#52164=CARTESIAN_POINT('Ctrl Pts',(-0.232387557061457,0.0314043048985863,
-1.51495));
#52165=CARTESIAN_POINT('Ctrl Pts',(-0.230814689799066,0.0376559832384288,
-1.51495));
#52166=CARTESIAN_POINT('Ctrl Pts',(-0.228996136394989,0.0438440137987597,
-1.51495));
#52167=CARTESIAN_POINT('Ctrl Pts',(-0.227643249260427,0.0484475117848916,
-1.51495));
#52168=CARTESIAN_POINT('Ctrl Pts',(-0.226156705072274,0.0530074190901877,
-1.51495));
#52169=CARTESIAN_POINT('Ctrl Pts',(-0.224540759462049,0.0575117578727007,
-1.51495));
#52170=CARTESIAN_POINT('Ctrl Pts',(-0.219610975017165,0.0712531976365204,
-1.51495));
#52171=CARTESIAN_POINT('Ctrl Pts',(-0.213475147483757,0.0844959874752671,
-1.51495));
#52172=CARTESIAN_POINT('Ctrl Pts',(-0.206180399857752,0.097038108714997,
-1.51495));
#52173=CARTESIAN_POINT('Ctrl Pts',(-0.202999684165652,0.102506827289607,
-1.51495));
#52174=CARTESIAN_POINT('Ctrl Pts',(-0.199598120417428,0.107841928421567,
-1.51495));
#52175=CARTESIAN_POINT('Ctrl Pts',(-0.195977474949733,0.113024282643653,
-1.51495));
#52176=CARTESIAN_POINT('Ctrl Pts',(-0.193573374376874,0.116465354371122,
-1.51495));
#52177=CARTESIAN_POINT('Ctrl Pts',(-0.191072657180778,0.119839047867209,
-1.51495));
#52178=CARTESIAN_POINT('Ctrl Pts',(-0.188475578155228,0.123139297813982,
-1.51495));
#52179=CARTESIAN_POINT('Ctrl Pts',(-0.185966834432807,0.126327295273794,
-1.51495));
#52180=CARTESIAN_POINT('Ctrl Pts',(-0.183373651456097,0.129439708498115,
-1.51495));
#52181=CARTESIAN_POINT('Ctrl Pts',(-0.180699002448782,0.132469932176183,
-1.51495));
#52182=CARTESIAN_POINT('Ctrl Pts',(-0.175543696738069,0.138310597396014,
-1.51495));
#52183=CARTESIAN_POINT('Ctrl Pts',(-0.170083756237131,0.1438489438949,-1.51495));
#52184=CARTESIAN_POINT('Ctrl Pts',(-0.164325079865127,0.149051084203145,
-1.51495));
#52185=CARTESIAN_POINT('Ctrl Pts',(-0.153833986014853,0.158528286718191,
-1.51495));
#52186=CARTESIAN_POINT('Ctrl Pts',(-0.142351819020326,0.166892632944104,
-1.51495));
#52187=CARTESIAN_POINT('Ctrl Pts',(-0.130079371647154,0.174079981710603,
-1.51495));
#52188=CARTESIAN_POINT('Ctrl Pts',(-0.125535356483719,0.176741180474532,
-1.51495));
#52189=CARTESIAN_POINT('Ctrl Pts',(-0.120878783344098,0.179242125924473,
-1.51495));
#52190=CARTESIAN_POINT('Ctrl Pts',(-0.116145488887229,0.181566320250997,
-1.51495));
#52191=CARTESIAN_POINT('Ctrl Pts',(-0.104698309453902,0.187187240254196,
-1.51495));
#52192=CARTESIAN_POINT('Ctrl Pts',(-0.0927779625431565,0.191793755001339,
-1.51495));
#52193=CARTESIAN_POINT('Ctrl Pts',(-0.0805361366432621,0.195346249694064,
-1.51495));
#52194=CARTESIAN_POINT('Ctrl Pts',(-0.0695096699048282,0.198546055416519,
-1.51495));
#52195=CARTESIAN_POINT('Ctrl Pts',(-0.0582215637403063,0.20089035007889,
-1.51495));
#52196=CARTESIAN_POINT('Ctrl Pts',(-0.0467843784263279,0.202323822435583,
-1.51495));
#52197=CARTESIAN_POINT('Ctrl Pts',(-0.0426471497538938,0.202842359363371,
-1.51495));
#52198=CARTESIAN_POINT('Ctrl Pts',(-0.0384978685117633,0.203240408900611,
-1.51495));
#52199=CARTESIAN_POINT('Ctrl Pts',(-0.0343490085389219,0.20351577767736,
-1.51495));
#52200=CARTESIAN_POINT('Ctrl Pts',(-0.0213910546068069,0.204375825002844,
-1.51495));
#52201=CARTESIAN_POINT('Ctrl Pts',(-0.0084143667936003,0.204045484383494,
-1.51495));
#52202=CARTESIAN_POINT('Ctrl Pts',(0.0044149276201895,0.202455455781444,
-1.51495));
#52203=CARTESIAN_POINT('Ctrl Pts',(0.0139437527039043,0.201274478563339,
-1.51495));
#52204=CARTESIAN_POINT('Ctrl Pts',(0.0233913223400742,0.199397635842591,
-1.51495));
#52205=CARTESIAN_POINT('Ctrl Pts',(0.0326814423280607,0.196779569448552,
-1.51495));
#52206=CARTESIAN_POINT('Origin',(0.,0.,-1.51495));
#52207=CARTESIAN_POINT('Origin',(0.,0.,-1.69285451186048));
#52208=CARTESIAN_POINT('Ctrl Pts',(0.0326814423280649,0.196779569448552,
-1.51495));
#52209=CARTESIAN_POINT('Ctrl Pts',(-0.0328441439546247,0.207662155862942,
-1.51071024239301));
#52210=CARTESIAN_POINT('Ctrl Pts',(-0.15586916575445,0.16506957102402,-1.50334507967983));
#52211=CARTESIAN_POINT('Ctrl Pts',(-0.19892022304172,0.0488485439360305,
-1.49597991696666));
#52212=CARTESIAN_POINT('Ctrl Pts',(-0.199405781844198,-0.000173944371801573,
-1.49285451186048));
#52213=CARTESIAN_POINT('Ctrl Pts',(0.0401483265697123,0.241738731637385,
-1.54126273851832));
#52214=CARTESIAN_POINT('Ctrl Pts',(-0.0403482014090971,0.2551077142209,
-1.53702298091132));
#52215=CARTESIAN_POINT('Ctrl Pts',(-0.214347846184126,0.194867167024894,
-1.52854346569733));
#52216=CARTESIAN_POINT('Ctrl Pts',(-0.280010781085592,-0.0753312380677012,
-1.51582419287635));
#52217=CARTESIAN_POINT('Ctrl Pts',(-0.0881075174888988,-0.275964967577725,
-1.50310492005536));
#52218=CARTESIAN_POINT('Ctrl Pts',(0.184340118489057,-0.223572751555067,
-1.49038564723437));
#52219=CARTESIAN_POINT('Ctrl Pts',(0.28778640445331,0.0340957051198576,
-1.47766637441339));
#52220=CARTESIAN_POINT('Ctrl Pts',(0.127058169441575,0.260417170385679,
-1.4649471015924));
#52221=CARTESIAN_POINT('Ctrl Pts',(-0.150222375650171,0.247794607963362,
-1.45222782877142));
#52222=CARTESIAN_POINT('Ctrl Pts',(-0.289672761002644,0.00776434744478158,
-1.43950855595043));
#52223=CARTESIAN_POINT('Ctrl Pts',(-0.163289491859137,-0.239382486652227,
-1.42678928312944));
#52224=CARTESIAN_POINT('Ctrl Pts',(0.11293188259826,-0.266861686500435,
-1.41407001030846));
#52225=CARTESIAN_POINT('Ctrl Pts',(0.285523362567467,-0.0494498753666089,
-1.40135073748747));
#52226=CARTESIAN_POINT('Ctrl Pts',(0.196099310106758,0.213338956448214,
-1.38863146466649));
#52227=CARTESIAN_POINT('Ctrl Pts',(-0.0732765984215447,0.280355495930703,
-1.3759121918455));
#52228=CARTESIAN_POINT('Ctrl Pts',(-0.275409880441213,0.0901002704077519,
-1.36319291902451));
#52229=CARTESIAN_POINT('Ctrl Pts',(-0.224809881733275,-0.182836322382666,
-1.35047364620353));
#52230=CARTESIAN_POINT('Ctrl Pts',(0.0320893441203098,-0.287991164877318,
-1.33775437338254));
#52231=CARTESIAN_POINT('Ctrl Pts',(0.259541485891461,-0.128867571492712,
-1.32503510056156));
#52232=CARTESIAN_POINT('Ctrl Pts',(0.248822377267493,0.148512797676952,
-1.31231582774057));
#52233=CARTESIAN_POINT('Ctrl Pts',(0.00976858664482186,0.289608712370884,
-1.29959655491958));
#52234=CARTESIAN_POINT('Ctrl Pts',(-0.238249469334144,0.164941871833619,
-1.2868772820986));
#52235=CARTESIAN_POINT('Ctrl Pts',(-0.267635168780419,-0.111085760740929,
-1.27415800927761));
#52236=CARTESIAN_POINT('Ctrl Pts',(-0.0514223964570787,-0.285174276017006,
-1.26143873645663));
#52237=CARTESIAN_POINT('Ctrl Pts',(0.211978727731969,-0.197569353324888,
-1.24871946363564));
#52238=CARTESIAN_POINT('Ctrl Pts',(0.280855146490056,0.0713373462265733,
-1.23600019081465));
#52239=CARTESIAN_POINT('Ctrl Pts',(0.0920016273185971,0.274780514150071,
-1.22328091799367));
#52240=CARTESIAN_POINT('Ctrl Pts',(-0.18127823792608,0.226068199461604,
-1.21056164517268));
#52241=CARTESIAN_POINT('Ctrl Pts',(-0.288206054094843,-0.030098184743108,
-1.1978423723517));
#52242=CARTESIAN_POINT('Ctrl Pts',(-0.130658287529358,-0.258644625417178,
-1.18512309953071));
#52243=CARTESIAN_POINT('Ctrl Pts',(0.146789551427754,-0.249842866504755,
-1.17240382670972));
#52244=CARTESIAN_POINT('Ctrl Pts',(0.289534279139855,-0.011769942801552,
-1.15968455388874));
#52245=CARTESIAN_POINT('Ctrl Pts',(0.166584563160005,0.237103803574601,
-1.14696528106775));
#52246=CARTESIAN_POINT('Ctrl Pts',(-0.109233383036356,0.268396531986266,
-1.13424600824676));
#52247=CARTESIAN_POINT('Ctrl Pts',(-0.284812065591009,0.0533921122033667,
-1.12152673542578));
#52248=CARTESIAN_POINT('Ctrl Pts',(-0.199029697734655,-0.210608190181913,
-1.10880746260479));
#52249=CARTESIAN_POINT('Ctrl Pts',(0.0693945492688924,-0.281341477360996,
-1.09608818978381));
#52250=CARTESIAN_POINT('Ctrl Pts',(0.274138094219812,-0.0938985391229988,
-1.08336891696282));
#52251=CARTESIAN_POINT('Ctrl Pts',(0.22731568070417,0.17971146779753,-1.07064964414184));
#52252=CARTESIAN_POINT('Ctrl Pts',(-0.0281055678388845,0.288407190285495,
-1.05793037132085));
#52253=CARTESIAN_POINT('Ctrl Pts',(-0.257735420509811,0.132442755054978,
-1.04521109849987));
#52254=CARTESIAN_POINT('Ctrl Pts',(-0.250851415900536,-0.145059289577135,
-1.03249182567888));
#52255=CARTESIAN_POINT('Ctrl Pts',(-0.0137707395979083,-0.289446017562602,
-1.01977255285789));
#52256=CARTESIAN_POINT('Ctrl Pts',(0.23594681344234,-0.168219296093908,
-1.00705328003691));
#52257=CARTESIAN_POINT('Ctrl Pts',(0.269145073752699,0.107375786966052,
-0.994334007215921));
#52258=CARTESIAN_POINT('Ctrl Pts',(0.0553592779511471,0.28443625067254,
-0.981614734394934));
#52259=CARTESIAN_POINT('Ctrl Pts',(-0.209227592605962,0.200480534826297,
-0.968895461573949));
#52260=CARTESIAN_POINT('Ctrl Pts',(-0.281814369117759,-0.0674484374221064,
-0.956176188752962));
#52261=CARTESIAN_POINT('Ctrl Pts',(-0.0957909656814833,-0.273482579419117,
-0.943456915931977));
#52262=CARTESIAN_POINT('Ctrl Pts',(0.178136113319103,-0.228552303605735,
-0.93073764311099));
#52263=CARTESIAN_POINT('Ctrl Pts',(0.288594549947327,0.0261116083883038,
-0.918018370290005));
#52264=CARTESIAN_POINT('Ctrl Pts',(0.134220896119848,0.256813904212193,
-0.905299097469018));
#52265=CARTESIAN_POINT('Ctrl Pts',(-0.143322098600399,0.25184798272907,
-0.892579824648033));
#52266=CARTESIAN_POINT('Ctrl Pts',(-0.289343929848329,0.0157708786010744,
-0.879860551827046));
#52267=CARTESIAN_POINT('Ctrl Pts',(-0.16984599360104,-0.234778552703606,
-0.867141279006061));
#52268=CARTESIAN_POINT('Ctrl Pts',(0.105513061815336,-0.269880759110903,
-0.854422006185075));
#52269=CARTESIAN_POINT('Ctrl Pts',(0.284046848923501,-0.0573237993206493,
-0.841702733364088));
#52270=CARTESIAN_POINT('Ctrl Pts',(0.201921795448932,0.207837000735201,
-0.828983460543103));
#52271=CARTESIAN_POINT('Ctrl Pts',(-0.0654991037270535,0.282273799285157,
-0.816264187722116));
#52272=CARTESIAN_POINT('Ctrl Pts',(-0.27281400101847,0.0976788165377675,
-0.803544914901131));
#52273=CARTESIAN_POINT('Ctrl Pts',(-0.22977800911779,-0.176552249710359,
-0.790825642080144));
#52274=CARTESIAN_POINT('Ctrl Pts',(0.0241164016494981,-0.288768124147047,
-0.778106369259159));
#52275=CARTESIAN_POINT('Ctrl Pts',(0.255880120536876,-0.135992625777865,
-0.765387096438172));
#52276=CARTESIAN_POINT('Ctrl Pts',(0.252832519389947,0.141578061474426,
-0.752667823617187));
#52277=CARTESIAN_POINT('Ctrl Pts',(0.017770264267596,0.28922802087589,-0.7399485507962));
#52278=CARTESIAN_POINT('Ctrl Pts',(-0.233599077162506,0.171464577976764,
-0.727229277975216));
#52279=CARTESIAN_POINT('Ctrl Pts',(-0.270603552919432,-0.103645296561416,
-0.714510005154228));
#52280=CARTESIAN_POINT('Ctrl Pts',(-0.0592855824712138,-0.283643878945013,
-0.701790732333244));
#52281=CARTESIAN_POINT('Ctrl Pts',(0.206436480994706,-0.203353410756857,
-0.689071459512256));
#52282=CARTESIAN_POINT('Ctrl Pts',(0.282719745917391,0.0635466412985803,
-0.676352186691271));
#52283=CARTESIAN_POINT('Ctrl Pts',(0.0995620015137612,0.272132390954289,
-0.663632913870285));
#52284=CARTESIAN_POINT('Ctrl Pts',(-0.174959952628603,0.230992738691331,
-0.650913641049299));
#52285=CARTESIAN_POINT('Ctrl Pts',(-0.288927904593446,-0.0221200429286395,
-0.638194368228313));
#52286=CARTESIAN_POINT('Ctrl Pts',(-0.137757859397795,-0.254934114088448,
-0.625475095407327));
#52287=CARTESIAN_POINT('Ctrl Pts',(0.139827261507635,-0.253804978854237,
-0.612755822586341));
#52288=CARTESIAN_POINT('Ctrl Pts',(0.289098296181977,-0.0197688010916725,
-0.600036549765355));
#52289=CARTESIAN_POINT('Ctrl Pts',(0.173074971905226,0.23240844315973,-0.587317276944369));
#52290=CARTESIAN_POINT('Ctrl Pts',(-0.101772580422917,0.271313420652177,
-0.574598004123382));
#52291=CARTESIAN_POINT('Ctrl Pts',(-0.283227359985977,0.0612445336932068,
-0.561878731302398));
#52292=CARTESIAN_POINT('Ctrl Pts',(-0.204775312365271,-0.205026100283915,
-0.54915945848141));
#52293=CARTESIAN_POINT('Ctrl Pts',(0.0615911434010899,-0.283152187712668,
-0.536440185660426));
#52294=CARTESIAN_POINT('Ctrl Pts',(0.271437781785443,-0.101440430654277,
-0.523720912839439));
#52295=CARTESIAN_POINT('Ctrl Pts',(0.232196434301655,0.173359298134017,
-0.511001640018453));
#52296=CARTESIAN_POINT('Ctrl Pts',(-0.0201226275869376,0.289073883654192,
-0.498282367197468));
#52297=CARTESIAN_POINT('Ctrl Pts',(-0.253975930055376,0.139516512658715,
-0.48556309437648));
#52298=CARTESIAN_POINT('Ctrl Pts',(-0.25476531466985,-0.138069782331531,
-0.472843821555496));
#52299=CARTESIAN_POINT('Ctrl Pts',(-0.0217663936081401,-0.288954761963176,
-0.460124548734509));
#52300=CARTESIAN_POINT('Ctrl Pts',(0.231206707569178,-0.174677098461904,
-0.447405275913524));
#52301=CARTESIAN_POINT('Ctrl Pts',(0.272010328400097,0.0998950028551257,
-0.434686003092537));
#52302=CARTESIAN_POINT('Ctrl Pts',(0.0632005594130015,0.28279731194215,
-0.421966730271552));
#52303=CARTESIAN_POINT('Ctrl Pts',(-0.203605925974667,0.206187432354038,
-0.409247457450565));
#52304=CARTESIAN_POINT('Ctrl Pts',(-0.283571104011678,-0.0596327034452211,
-0.39652818462958));
#52305=CARTESIAN_POINT('Ctrl Pts',(-0.103314014236298,-0.270730206689346,
-0.383808911808593));
#52306=CARTESIAN_POINT('Ctrl Pts',(0.171750362695484,-0.23338903845568,
-0.371089638987607));
#52307=CARTESIAN_POINT('Ctrl Pts',(0.28920605433811,0.0181242510447194,
-0.358370366166621));
#52308=CARTESIAN_POINT('Ctrl Pts',(0.141268501588536,0.253005614191318,
-0.345651093345636));
#52309=CARTESIAN_POINT('Ctrl Pts',(-0.136305707962405,0.255713480995264,
-0.332931820524649));
#52310=CARTESIAN_POINT('Ctrl Pts',(-0.288797424950404,0.0237629463370206,
-0.320212547703663));
#52311=CARTESIAN_POINT('Ctrl Pts',(-0.176270881356031,-0.229993927680813,
-0.307493274882677));
#52312=CARTESIAN_POINT('Ctrl Pts',(0.0980126540007645,-0.272694243090937,
-0.294774002061692));
#52313=CARTESIAN_POINT('Ctrl Pts',(0.282353754487939,-0.0651535657817629,
-0.282054729240705));
#52314=CARTESIAN_POINT('Ctrl Pts',(0.207589704923852,0.202176025115757,
-0.26933545641972));
#52315=CARTESIAN_POINT('Ctrl Pts',(-0.0576714181337695,0.283976476308512,
-0.256616183598733));
#52316=CARTESIAN_POINT('Ctrl Pts',(-0.270009693456009,0.10518265989541,
-0.243896910777747));
#52317=CARTESIAN_POINT('Ctrl Pts',(-0.234570505638583,-0.170133217702001,
-0.231177637956762));
#52318=CARTESIAN_POINT('Ctrl Pts',(0.0161250305881685,-0.289324420749436,
-0.218458365135775));
#52319=CARTESIAN_POINT('Ctrl Pts',(0.25202317124219,-0.143013722643587,
-0.20573909231479));
#52320=CARTESIAN_POINT('Ctrl Pts',(0.256649511832594,0.134535084822825,
-0.193019819493804));
#52321=CARTESIAN_POINT('Ctrl Pts',(0.0257582127796514,0.288626364785306,
-0.180300546672817));
#52322=CARTESIAN_POINT('Ctrl Pts',(-0.228769873386647,0.177856106989376,
-0.167581273851832));
#52323=CARTESIAN_POINT('Ctrl Pts',(-0.273365681038595,-0.0961253617725913,
-0.154862001030846));
#52324=CARTESIAN_POINT('Ctrl Pts',(-0.0671024131868596,-0.281897208169119,
-0.14214272820986));
#52325=CARTESIAN_POINT('Ctrl Pts',(0.200734471793731,-0.20898111135007,
-0.129423455388874));
#52326=CARTESIAN_POINT('Ctrl Pts',(0.284372086079907,0.0557055671966431,
-0.116704182567887));
#52327=CARTESIAN_POINT('Ctrl Pts',(0.107039034186323,0.269279733812547,
-0.103984909746902));
#52328=CARTESIAN_POINT('Ctrl Pts',(-0.168494133032722,0.235734189686348,
-0.0912656369259156));
#52329=CARTESIAN_POINT('Ctrl Pts',(-0.289455297174828,-0.014112499183932,
-0.0785463641049299));
#52330=CARTESIAN_POINT('Ctrl Pts',(-0.144701892960455,-0.251052617385527,
-0.0658270912839438));
#52331=CARTESIAN_POINT('Ctrl Pts',(0.132662010889486,-0.257527452585136,
-0.0531078184629578));
#52332=CARTESIAN_POINT('Ctrl Pts',(0.288627233657158,-0.0278415686410112,
-0.0403885456419716));
#52333=CARTESIAN_POINT('Ctrl Pts',(0.17905539955801,0.227722146128134,-0.0276692728209858));
#52334=CARTESIAN_POINT('Ctrl Pts',(-0.00252611781081248,0.258266416594894,
-0.0191897576069951));
#52335=CARTESIAN_POINT('Ctrl Pts',(-0.0796899944392906,0.231730462577249,
-0.0149499999999998));
#52336=CARTESIAN_POINT('Ctrl Pts',(0.0376593651558298,0.226752344241107,
-1.53249182567888));
#52337=CARTESIAN_POINT('Ctrl Pts',(-0.0378468489242729,0.239292528101581,
-1.52825206807188));
#52338=CARTESIAN_POINT('Ctrl Pts',(-0.201059533472651,0.182786542475944,
-1.51977255285789));
#52339=CARTESIAN_POINT('Ctrl Pts',(-0.262651750482346,-0.0706611419309478,
-1.50705328003691));
#52340=CARTESIAN_POINT('Ctrl Pts',(-0.0826453667583571,-0.258856753747412,
-1.49433400721592));
#52341=CARTESIAN_POINT('Ctrl Pts',(0.172912109375083,-0.209712548668413,
-1.48161473439494));
#52342=CARTESIAN_POINT('Ctrl Pts',(0.269945330682025,0.0319819708332,-1.46889546157395));
#52343=CARTESIAN_POINT('Ctrl Pts',(0.119181306118034,0.244272829039931,
-1.45617618875296));
#52344=CARTESIAN_POINT('Ctrl Pts',(-0.140909467032535,0.23243279165658,
-1.44345691593198));
#52345=CARTESIAN_POINT('Ctrl Pts',(-0.271714744158876,0.00728300331800845,
-1.43073764311099));
#52346=CARTESIAN_POINT('Ctrl Pts',(-0.153166498468018,-0.224542172663008,
-1.41801837029));
#52347=CARTESIAN_POINT('Ctrl Pts',(0.105930766432288,-0.250317822850489,
-1.40529909746902));
#52348=CARTESIAN_POINT('Ctrl Pts',(0.267822584156242,-0.0463842723334394,
-1.39257982464803));
#52349=CARTESIAN_POINT('Ctrl Pts',(0.183942299893718,0.200113188999222,
-1.37986055182705));
#52350=CARTESIAN_POINT('Ctrl Pts',(-0.0687338779249646,0.262975095023348,
-1.36714127900606));
#52351=CARTESIAN_POINT('Ctrl Pts',(-0.258336078766579,0.0845145806521449,
-1.35442200618507));
#52352=CARTESIAN_POINT('Ctrl Pts',(-0.210872984011728,-0.171501539831365,
-1.34170273336409));
#52353=CARTESIAN_POINT('Ctrl Pts',(0.0300999924801246,-0.270137397157419,
-1.3289834605431));
#52354=CARTESIAN_POINT('Ctrl Pts',(0.243451431862348,-0.120878535825459,
-1.31626418772212));
#52355=CARTESIAN_POINT('Ctrl Pts',(0.233396845275428,0.139305872894083,
-1.30354491490113));
#52356=CARTESIAN_POINT('Ctrl Pts',(0.009162991410735,0.271654666167656,
-1.29082564208014));
#52357=CARTESIAN_POINT('Ctrl Pts',(-0.223479395791461,0.154716440549094,
-1.27810636925916));
#52358=CARTESIAN_POINT('Ctrl Pts',(-0.251043353753325,-0.104199093331874,
-1.26538709643817));
#52359=CARTESIAN_POINT('Ctrl Pts',(-0.048234508653865,-0.267495138930051,
-1.25266782361719));
#52360=CARTESIAN_POINT('Ctrl Pts',(0.198837286507208,-0.185321209030822,
-1.2399485507962));
#52361=CARTESIAN_POINT('Ctrl Pts',(0.26344377017055,0.0669148480231117,
-1.22722927797521));
#52362=CARTESIAN_POINT('Ctrl Pts',(0.0862980645558325,0.257745729504231,
-1.21451000515423));
#52363=CARTESIAN_POINT('Ctrl Pts',(-0.170040047497623,0.212053293400986,
-1.20179073233324));
#52364=CARTESIAN_POINT('Ctrl Pts',(-0.270338964500376,-0.0282322733377271,
-1.18907145951226));
#52365=CARTESIAN_POINT('Ctrl Pts',(-0.122558237941992,-0.242610171491602,
-1.17635218669127));
#52366=CARTESIAN_POINT('Ctrl Pts',(0.137689457832816,-0.234354070148971,
-1.16363291387029));
#52367=CARTESIAN_POINT('Ctrl Pts',(0.271584847361581,-0.011040275191973,
-1.1509136410493));
#52368=CARTESIAN_POINT('Ctrl Pts',(0.156257294621586,0.222404754607843,
-1.13819436822831));
#52369=CARTESIAN_POINT('Ctrl Pts',(-0.102461552210156,0.251757516893735,
-1.12547509540732));
#52370=CARTESIAN_POINT('Ctrl Pts',(-0.267155383431844,0.0500821135450386,
-1.11275582258634));
#52371=CARTESIAN_POINT('Ctrl Pts',(-0.186691020628951,-0.19755171426878,
-1.10003654976535));
#52372=CARTESIAN_POINT('Ctrl Pts',(0.0650924931131031,-0.263899951372112,
-1.08731727694437));
#52373=CARTESIAN_POINT('Ctrl Pts',(0.25714313585204,-0.0880773789236763,
-1.07459800412338));
#52374=CARTESIAN_POINT('Ctrl Pts',(0.213223438103214,0.168570407952775,
-1.0618787313024));
#52375=CARTESIAN_POINT('Ctrl Pts',(-0.0263631870264576,0.270527631423682,
-1.04915945848141));
#52376=CARTESIAN_POINT('Ctrl Pts',(-0.241757331970419,0.124232078918636,
-1.03644018566043));
#52377=CARTESIAN_POINT('Ctrl Pts',(-0.235300095381367,-0.13606646209638,
-1.02372091283944));
#52378=CARTESIAN_POINT('Ctrl Pts',(-0.0129170342899085,-0.271502057485862,
-1.01100164001845));
#52379=CARTESIAN_POINT('Ctrl Pts',(0.221319491096378,-0.15779068367538,
-0.998282367197467));
#52380=CARTESIAN_POINT('Ctrl Pts',(0.252459653448979,0.100719116230859,
-0.985563094376481));
#52381=CARTESIAN_POINT('Ctrl Pts',(0.0519273265226976,0.266802866840123,
-0.972843821555495));
#52382=CARTESIAN_POINT('Ctrl Pts',(-0.19625670566722,0.188051914307071,
-0.96012454873451));
#52383=CARTESIAN_POINT('Ctrl Pts',(-0.264343526605969,-0.0632670288177248,
-0.947405275913523));
#52384=CARTESIAN_POINT('Ctrl Pts',(-0.0898524861046148,-0.256528259134786,
-0.934686003092538));
#52385=CARTESIAN_POINT('Ctrl Pts',(0.167092716237531,-0.21438339761807,
-0.921966730271551));
#52386=CARTESIAN_POINT('Ctrl Pts',(0.270703375882375,0.0244928413988521,
-0.909247457450566));
#52387=CARTESIAN_POINT('Ctrl Pts',(0.125899985638092,0.240892944293169,
-0.896528184629579));
#52388=CARTESIAN_POINT('Ctrl Pts',(-0.134436966799118,0.236234880895597,
-0.883808911808593));
#52389=CARTESIAN_POINT('Ctrl Pts',(-0.271406298612747,0.014793176373984,
-0.871089638987608));
#52390=CARTESIAN_POINT('Ctrl Pts',(-0.159316535451862,-0.220223655690117,
-0.858370366166621));
#52391=CARTESIAN_POINT('Ctrl Pts',(0.0989718691441357,-0.253149730618106,
-0.845651093345636));
#52392=CARTESIAN_POINT('Ctrl Pts',(0.266437605721858,-0.0537700590580635,
-0.832931820524649));
#52393=CARTESIAN_POINT('Ctrl Pts',(0.189403825201247,0.194952322358671,
-0.820212547703663));
#52394=CARTESIAN_POINT('Ctrl Pts',(-0.0614385424098267,0.264774474790263,
-0.807493274882678));
#52395=CARTESIAN_POINT('Ctrl Pts',(-0.255901128684366,0.0916233012501255,
-0.794774002061691));
#52396=CARTESIAN_POINT('Ctrl Pts',(-0.215533116557709,-0.16560704290828,
-0.782054729240706));
#52397=CARTESIAN_POINT('Ctrl Pts',(0.0226213258075957,-0.270866189496973,
-0.769335456419719));
#52398=CARTESIAN_POINT('Ctrl Pts',(0.240017049743885,-0.127561878420417,
-0.756616183598734));
#52399=CARTESIAN_POINT('Ctrl Pts',(0.237158382042199,0.132801049773826,
-0.743896910777747));
#52400=CARTESIAN_POINT('Ctrl Pts',(0.016668611823881,0.271297575318631,
-0.731177637956762));
#52401=CARTESIAN_POINT('Ctrl Pts',(-0.21911730073364,0.160834777063628,
-0.718458365135776));
#52402=CARTESIAN_POINT('Ctrl Pts',(-0.253827715438233,-0.097219894411127,
-0.70573909231479));
#52403=CARTESIAN_POINT('Ctrl Pts',(-0.0556102231280499,-0.266059617525005,
-0.693019819493804));
#52404=CARTESIAN_POINT('Ctrl Pts',(0.193638626650242,-0.190746688733808,
-0.680300546672818));
#52405=CARTESIAN_POINT('Ctrl Pts',(0.265192775339705,0.0596071212316804,
-0.667581273851832));
#52406=CARTESIAN_POINT('Ctrl Pts',(0.0933897397726324,0.255261774457328,
-0.654862001030846));
#52407=CARTESIAN_POINT('Ctrl Pts',(-0.164113458932014,0.216672540002821,
-0.64214272820986));
#52408=CARTESIAN_POINT('Ctrl Pts',(-0.271016064490275,-0.0207487296504358,
-0.629423455388874));
#52409=CARTESIAN_POINT('Ctrl Pts',(-0.129217677881022,-0.239129690161929,
-0.616704182567888));
#52410=CARTESIAN_POINT('Ctrl Pts',(0.131158789164291,-0.23807055470776,
-0.603984909746902));
#52411=CARTESIAN_POINT('Ctrl Pts',(0.271175892796963,-0.0185432510545995,
-0.591265636925916));
#52412=CARTESIAN_POINT('Ctrl Pts',(0.162345335987956,0.218000479074844,
-0.57854636410493));
#52413=CARTESIAN_POINT('Ctrl Pts',(-0.0954632757194232,0.254493575523668,
-0.565827091283944));
#52414=CARTESIAN_POINT('Ctrl Pts',(-0.265668920305149,0.0574477308324719,
-0.553107818462958));
#52415=CARTESIAN_POINT('Ctrl Pts',(-0.19208044075941,-0.192315681293997,
-0.540388545641972));
#52416=CARTESIAN_POINT('Ctrl Pts',(0.0577728527658405,-0.265598408273091,
-0.527669272820986));
#52417=CARTESIAN_POINT('Ctrl Pts',(0.254610226994079,-0.0951517172936434,
-0.51495));
#52418=CARTESIAN_POINT('Ctrl Pts',(0.217801613525897,0.16261203565363,-0.502230727179015));
#52419=CARTESIAN_POINT('Ctrl Pts',(-0.0188751423767444,0.271152993703107,
-0.489511454358028));
#52420=CARTESIAN_POINT('Ctrl Pts',(-0.238230907934349,0.130867304926385,
-0.476792181537042));
#52421=CARTESIAN_POINT('Ctrl Pts',(-0.238971355319949,-0.129510263417352,
-0.464072908716056));
#52422=CARTESIAN_POINT('Ctrl Pts',(-0.0204170045192572,-0.271041256860175,
-0.45135363589507));
#52423=CARTESIAN_POINT('Ctrl Pts',(0.216873244061779,-0.163848140069192,
-0.438634363074084));
#52424=CARTESIAN_POINT('Ctrl Pts',(0.255147279067533,0.0937020969786091,
-0.425915090253098));
#52425=CARTESIAN_POINT('Ctrl Pts',(0.0592824943987202,0.265265532724626,
-0.413195817432112));
#52426=CARTESIAN_POINT('Ctrl Pts',(-0.190983549485114,0.193405017568571,
-0.400476544611126));
#52427=CARTESIAN_POINT('Ctrl Pts',(-0.265991354211865,-0.0559358246320336,
-0.38775727179014));
#52428=CARTESIAN_POINT('Ctrl Pts',(-0.0969091496524436,-0.25394651741523,
-0.375037998969154));
#52429=CARTESIAN_POINT('Ctrl Pts',(0.161102844801386,-0.218920283198089,
-0.362318726148168));
#52430=CARTESIAN_POINT('Ctrl Pts',(0.271276970577709,0.0170006534913469,
-0.349599453327182));
#52431=CARTESIAN_POINT('Ctrl Pts',(0.132510680790197,0.237320745978342,
-0.336880180506196));
#52432=CARTESIAN_POINT('Ctrl Pts',(-0.127855551340783,0.239860740879152,
-0.32416090768521));
#52433=CARTESIAN_POINT('Ctrl Pts',(-0.270893673821908,0.0222897826570762,
-0.311441634864224));
#52434=CARTESIAN_POINT('Ctrl Pts',(-0.165343117746152,-0.215735649432766,
-0.298722362043238));
#52435=CARTESIAN_POINT('Ctrl Pts',(0.0919364427430842,-0.255788795047858,
-0.286003089222253));
#52436=CARTESIAN_POINT('Ctrl Pts',(0.264849473238144,-0.0611144257960386,
-0.273283816401266));
#52437=CARTESIAN_POINT('Ctrl Pts',(0.194720357441154,0.189642294115757,
-0.260564543580281));
#52438=CARTESIAN_POINT('Ctrl Pts',(-0.0540961275380471,0.266371595797377,
-0.247845270759294));
#52439=CARTESIAN_POINT('Ctrl Pts',(-0.253270671787972,0.0986619502106732,
-0.235125997938308));
#52440=CARTESIAN_POINT('Ctrl Pts',(-0.220028506326227,-0.159585953338581,
-0.222406725117323));
#52441=CARTESIAN_POINT('Ctrl Pts',(0.0151253730093691,-0.271387998963875,
-0.209687452296336));
#52442=CARTESIAN_POINT('Ctrl Pts',(0.236399208745608,-0.134147708347888,
-0.196968179475351));
#52443=CARTESIAN_POINT('Ctrl Pts',(0.240738743279549,0.126194696479222,
-0.184248906654364));
#52444=CARTESIAN_POINT('Ctrl Pts',(0.0241613542508698,0.27073321838649,
-0.171529633833378));
#52445=CARTESIAN_POINT('Ctrl Pts',(-0.214587479345165,0.166830068662447,
-0.158810361012393));
#52446=CARTESIAN_POINT('Ctrl Pts',(-0.2564186077701,-0.0901661515940091,
-0.146091088191407));
#52447=CARTESIAN_POINT('Ctrl Pts',(-0.0629424560611133,-0.264421230120684,
-0.133371815370421));
#52448=CARTESIAN_POINT('Ctrl Pts',(0.188290108667841,-0.196025504807486,
-0.120652542549435));
#52449=CARTESIAN_POINT('Ctrl Pts',(0.266742680076926,0.0522521478604723,
-0.107933269728448));
#52450=CARTESIAN_POINT('Ctrl Pts',(0.100403240153755,0.252585965372765,
-0.0952139969074626));
#52451=CARTESIAN_POINT('Ctrl Pts',(-0.158048482331552,0.221120048769588,
-0.0824947240864768));
#52452=CARTESIAN_POINT('Ctrl Pts',(-0.271510761816407,-0.013237606780604,
-0.0697754512654906));
#52453=CARTESIAN_POINT('Ctrl Pts',(-0.135731221979467,-0.235488823551147,
-0.0570561784445049));
#52454=CARTESIAN_POINT('Ctrl Pts',(0.124437742173868,-0.241562256840637,
-0.0443369056235188));
#52455=CARTESIAN_POINT('Ctrl Pts',(0.270734033393368,-0.0261155542346787,
-0.0316176328025325));
#52456=CARTESIAN_POINT('Ctrl Pts',(0.167955012106663,0.213604705048369,
-0.0188983599815468));
#52457=CARTESIAN_POINT('Ctrl Pts',(-0.00236951328217672,0.2422554094041,
-0.0104188447675561));
#52458=CARTESIAN_POINT('Ctrl Pts',(-0.0747496809025027,0.217364529322868,
-0.00617908716056078));
#52459=CARTESIAN_POINT('Ctrl Pts',(0.0351704037419473,0.21176595684483,
-1.52372091283944));
#52460=CARTESIAN_POINT('Ctrl Pts',(-0.0353454964394489,0.223477341982261,
-1.51948115523244));
#52461=CARTESIAN_POINT('Ctrl Pts',(-0.187771220761176,0.170705917926994,
-1.51100164001845));
#52462=CARTESIAN_POINT('Ctrl Pts',(-0.2452927198791,-0.0659910457941944,
-1.49828236719747));
#52463=CARTESIAN_POINT('Ctrl Pts',(-0.0771832160278151,-0.2417485399171,
-1.48556309437648));
#52464=CARTESIAN_POINT('Ctrl Pts',(0.161484100261109,-0.19585234578176,
-1.47284382155549));
#52465=CARTESIAN_POINT('Ctrl Pts',(0.252104256910741,0.0298682365465424,
-1.46012454873451));
#52466=CARTESIAN_POINT('Ctrl Pts',(0.111304442794493,0.228128487694183,
-1.44740527591352));
#52467=CARTESIAN_POINT('Ctrl Pts',(-0.131596558414898,0.217070975349797,
-1.43468600309254));
#52468=CARTESIAN_POINT('Ctrl Pts',(-0.253756727315109,0.00680165919123546,
-1.42196673027155));
#52469=CARTESIAN_POINT('Ctrl Pts',(-0.143043505076898,-0.209701858673789,
-1.40924745745057));
#52470=CARTESIAN_POINT('Ctrl Pts',(0.0989296502663155,-0.233773959200543,
-1.39652818462958));
#52471=CARTESIAN_POINT('Ctrl Pts',(0.250121805745017,-0.04331866930027,
-1.38380891180859));
#52472=CARTESIAN_POINT('Ctrl Pts',(0.171785289680678,0.18688742155023,-1.37108963898761));
#52473=CARTESIAN_POINT('Ctrl Pts',(-0.0641911574283849,0.245594694115993,
-1.35837036616662));
#52474=CARTESIAN_POINT('Ctrl Pts',(-0.241262277091944,0.0789288908965379,
-1.34565109334564));
#52475=CARTESIAN_POINT('Ctrl Pts',(-0.196936086290182,-0.160166757280064,
-1.33293182052465));
#52476=CARTESIAN_POINT('Ctrl Pts',(0.0281106408399401,-0.25228362943752,
-1.32021254770367));
#52477=CARTESIAN_POINT('Ctrl Pts',(0.227361377833234,-0.112889500158205,
-1.30749327488268));
#52478=CARTESIAN_POINT('Ctrl Pts',(0.217971313283363,0.130098948111214,
-1.29477400206169));
#52479=CARTESIAN_POINT('Ctrl Pts',(0.00855739617664794,0.253700619964428,
-1.2820547292407));
#52480=CARTESIAN_POINT('Ctrl Pts',(-0.208709322248779,0.14449100926457,
-1.26933545641972));
#52481=CARTESIAN_POINT('Ctrl Pts',(-0.234451538726231,-0.0973124259228192,
-1.25661618359873));
#52482=CARTESIAN_POINT('Ctrl Pts',(-0.0450466208506513,-0.249816001843096,
-1.24389691077775));
#52483=CARTESIAN_POINT('Ctrl Pts',(0.185695845282446,-0.173073064736756,
-1.23117763795676));
#52484=CARTESIAN_POINT('Ctrl Pts',(0.246032393851044,0.0624923498196499,
-1.21845836513578));
#52485=CARTESIAN_POINT('Ctrl Pts',(0.0805945017930683,0.240710944858392,
-1.20573909231479));
#52486=CARTESIAN_POINT('Ctrl Pts',(-0.158801857069166,0.198038387340367,
-1.19301981949381));
#52487=CARTESIAN_POINT('Ctrl Pts',(-0.252471874905908,-0.026366361932346,
-1.18030054667282));
#52488=CARTESIAN_POINT('Ctrl Pts',(-0.114458188354627,-0.226575717566026,
-1.16758127385183));
#52489=CARTESIAN_POINT('Ctrl Pts',(0.128589364237878,-0.218865273793187,
-1.15486200103085));
#52490=CARTESIAN_POINT('Ctrl Pts',(0.253635415583305,-0.0103106075823939,
-1.14214272820986));
#52491=CARTESIAN_POINT('Ctrl Pts',(0.145930026083168,0.207705705641086,
-1.12942345538887));
#52492=CARTESIAN_POINT('Ctrl Pts',(-0.0956897213839561,0.235118501801203,
-1.11670418256789));
#52493=CARTESIAN_POINT('Ctrl Pts',(-0.24949870127268,0.0467721148867109,
-1.1039849097469));
#52494=CARTESIAN_POINT('Ctrl Pts',(-0.174352343523248,-0.184495238355647,
-1.09126563692592));
#52495=CARTESIAN_POINT('Ctrl Pts',(0.0607904369573136,-0.246458425383229,
-1.07854636410493));
#52496=CARTESIAN_POINT('Ctrl Pts',(0.240148177484268,-0.0822562187243539,
-1.06582709128394));
#52497=CARTESIAN_POINT('Ctrl Pts',(0.199131195502257,0.15742934810802,-1.05310781846296));
#52498=CARTESIAN_POINT('Ctrl Pts',(-0.0246208062140303,0.252648072561869,
-1.04038854564197));
#52499=CARTESIAN_POINT('Ctrl Pts',(-0.225779243431027,0.116021402782294,
-1.02766927282099));
#52500=CARTESIAN_POINT('Ctrl Pts',(-0.219748774862197,-0.127073634615625,
-1.01495));
#52501=CARTESIAN_POINT('Ctrl Pts',(-0.0120633289819088,-0.253558097409122,
-1.00223072717902));
#52502=CARTESIAN_POINT('Ctrl Pts',(0.206692168750416,-0.147362071256852,
-0.989511454358028));
#52503=CARTESIAN_POINT('Ctrl Pts',(0.235774233145259,0.0940624454956667,
-0.976792181537043));
#52504=CARTESIAN_POINT('Ctrl Pts',(0.0484953750942479,0.249169483007708,
-0.964072908716057));
#52505=CARTESIAN_POINT('Ctrl Pts',(-0.183285818728479,0.175623293787844,
-0.951353635895069));
#52506=CARTESIAN_POINT('Ctrl Pts',(-0.24687268409418,-0.059085620213343,
-0.938634363074085));
#52507=CARTESIAN_POINT('Ctrl Pts',(-0.0839140065277464,-0.239573938850455,
-0.925915090253097));
#52508=CARTESIAN_POINT('Ctrl Pts',(0.15604931915596,-0.200214491630405,
-0.913195817432113));
#52509=CARTESIAN_POINT('Ctrl Pts',(0.252812201817423,0.0228740744094001,
-0.900476544611126));
#52510=CARTESIAN_POINT('Ctrl Pts',(0.117579075156335,0.224971984374146,
-0.887757271790141));
#52511=CARTESIAN_POINT('Ctrl Pts',(-0.125551834997836,0.220621779062123,
-0.875037998969154));
#52512=CARTESIAN_POINT('Ctrl Pts',(-0.253468667377166,0.0138154741468941,
-0.862318726148169));
#52513=CARTESIAN_POINT('Ctrl Pts',(-0.148787077302684,-0.205668758676629,
-0.849599453327182));
#52514=CARTESIAN_POINT('Ctrl Pts',(0.0924306764729358,-0.236418702125309,
-0.836880180506197));
#52515=CARTESIAN_POINT('Ctrl Pts',(0.248828362520214,-0.0502163187954781,
-0.82416090768521));
#52516=CARTESIAN_POINT('Ctrl Pts',(0.176885854953561,0.182067643982142,
-0.811441634864225));
#52517=CARTESIAN_POINT('Ctrl Pts',(-0.0573779810926002,0.247275150295369,
-0.798722362043238));
#52518=CARTESIAN_POINT('Ctrl Pts',(-0.238988256350262,0.0855677859624836,
-0.786003089222252));
#52519=CARTESIAN_POINT('Ctrl Pts',(-0.201288223997627,-0.1546618361062,
-0.773283816401267));
#52520=CARTESIAN_POINT('Ctrl Pts',(0.0211262499656935,-0.252964254846899,
-0.76056454358028));
#52521=CARTESIAN_POINT('Ctrl Pts',(0.224153978950893,-0.11913113106297,
-0.747845270759295));
#52522=CARTESIAN_POINT('Ctrl Pts',(0.22148424469445,0.124024038073226,-0.735125997938308));
#52523=CARTESIAN_POINT('Ctrl Pts',(0.0155669593801661,0.253367129761373,
-0.722406725117323));
#52524=CARTESIAN_POINT('Ctrl Pts',(-0.204635524304775,0.150204976150491,
-0.709687452296336));
#52525=CARTESIAN_POINT('Ctrl Pts',(-0.237051877957034,-0.0907944922608373,
-0.696968179475351));
#52526=CARTESIAN_POINT('Ctrl Pts',(-0.0519348637848862,-0.248475356104998,
-0.684248906654364));
#52527=CARTESIAN_POINT('Ctrl Pts',(0.180840772305777,-0.178139966710758,
-0.671529633833379));
#52528=CARTESIAN_POINT('Ctrl Pts',(0.24766580476202,0.0556676011647803,
-0.658810361012393));
#52529=CARTESIAN_POINT('Ctrl Pts',(0.0872174780315035,0.238391157960366,
-0.646091088191407));
#52530=CARTESIAN_POINT('Ctrl Pts',(-0.153266965235425,0.202352341314311,
-0.633371815370422));
#52531=CARTESIAN_POINT('Ctrl Pts',(-0.253104224387104,-0.019377416372232,
-0.620652542549434));
#52532=CARTESIAN_POINT('Ctrl Pts',(-0.120677496364249,-0.22332526623541,
-0.60793326972845));
#52533=CARTESIAN_POINT('Ctrl Pts',(0.122490316820947,-0.222336130561283,
-0.595213996907462));
#52534=CARTESIAN_POINT('Ctrl Pts',(0.253253489411948,-0.0173177010175265,
-0.582494724086478));
#52535=CARTESIAN_POINT('Ctrl Pts',(0.151615700070685,0.203592514989958,
-0.569775451265491));
#52536=CARTESIAN_POINT('Ctrl Pts',(-0.0891539710159297,0.237673730395159,
-0.557056178444505));
#52537=CARTESIAN_POINT('Ctrl Pts',(-0.248110480624322,0.0536509279717373,
-0.544336905623519));
#52538=CARTESIAN_POINT('Ctrl Pts',(-0.17938556915355,-0.179605262304078,
-0.531617632802533));
#52539=CARTESIAN_POINT('Ctrl Pts',(0.0539545621305916,-0.248044628833514,
-0.518898359981547));
#52540=CARTESIAN_POINT('Ctrl Pts',(0.237782672202715,-0.0888630039330099,
-0.506179087160561));
#52541=CARTESIAN_POINT('Ctrl Pts',(0.203406792750139,0.151864773173242,
-0.493459814339576));
#52542=CARTESIAN_POINT('Ctrl Pts',(-0.0176276571665515,0.253232103752022,
-0.480740541518589));
#52543=CARTESIAN_POINT('Ctrl Pts',(-0.222485885813322,0.122218097194056,
-0.468021268697603));
#52544=CARTESIAN_POINT('Ctrl Pts',(-0.223177395970049,-0.120950744503174,
-0.455301995876617));
#52545=CARTESIAN_POINT('Ctrl Pts',(-0.0190676154303742,-0.253127751757173,
-0.442582723055631));
#52546=CARTESIAN_POINT('Ctrl Pts',(0.20253978055438,-0.15301918167648,-0.429863450234645));
#52547=CARTESIAN_POINT('Ctrl Pts',(0.238284229734968,0.0875091911020926,
-0.417144177413659));
#52548=CARTESIAN_POINT('Ctrl Pts',(0.055364429384439,0.247733753507101,
-0.404424904592674));
#52549=CARTESIAN_POINT('Ctrl Pts',(-0.178361172995562,0.180622602783104,
-0.391705631771686));
#52550=CARTESIAN_POINT('Ctrl Pts',(-0.248411604412052,-0.0522389458188462,
-0.378986358950701));
#52551=CARTESIAN_POINT('Ctrl Pts',(-0.0905042850685891,-0.237162828141114,
-0.366267086129715));
#52552=CARTESIAN_POINT('Ctrl Pts',(0.150455326907289,-0.204451527940497,
-0.353547813308729));
#52553=CARTESIAN_POINT('Ctrl Pts',(0.253347886817307,0.0158770559379742,
-0.340828540487743));
#52554=CARTESIAN_POINT('Ctrl Pts',(0.123752859991858,0.221635877765367,
-0.328109267666758));
#52555=CARTESIAN_POINT('Ctrl Pts',(-0.119405394719161,0.22400800076304,
-0.315389994845771));
#52556=CARTESIAN_POINT('Ctrl Pts',(-0.25298992269341,0.0208166189771321,
-0.302670722024786));
#52557=CARTESIAN_POINT('Ctrl Pts',(-0.154415354136274,-0.201477371184718,
-0.289951449203799));
#52558=CARTESIAN_POINT('Ctrl Pts',(0.085860231485404,-0.238883347004778,
-0.277232176382814));
#52559=CARTESIAN_POINT('Ctrl Pts',(0.247345191988348,-0.0570752858103143,
-0.264512903561827));
#52560=CARTESIAN_POINT('Ctrl Pts',(0.181851009958456,0.177108563115757,
-0.251793630740842));
#52561=CARTESIAN_POINT('Ctrl Pts',(-0.0505208369423248,0.248766715286243,
-0.239074357919855));
#52562=CARTESIAN_POINT('Ctrl Pts',(-0.236531650119936,0.0921412405259361,
-0.22635508509887));
#52563=CARTESIAN_POINT('Ctrl Pts',(-0.20548650701387,-0.149038688975162,
-0.213635812277883));
#52564=CARTESIAN_POINT('Ctrl Pts',(0.0141257154305693,-0.253451577178313,
-0.200916539456898));
#52565=CARTESIAN_POINT('Ctrl Pts',(0.220775246249027,-0.12528169405219,
-0.188197266635911));
#52566=CARTESIAN_POINT('Ctrl Pts',(0.224827974726504,0.11785430813562,-0.175477993814926));
#52567=CARTESIAN_POINT('Ctrl Pts',(0.0225644957220879,0.252840071987673,
-0.162758720993939));
#52568=CARTESIAN_POINT('Ctrl Pts',(-0.200405085303683,0.155804030335518,
-0.150039448172954));
#52569=CARTESIAN_POINT('Ctrl Pts',(-0.239471534501604,-0.0842069414154272,
-0.137320175351968));
#52570=CARTESIAN_POINT('Ctrl Pts',(-0.0587824989353668,-0.246945252072248,
-0.124600902530982));
#52571=CARTESIAN_POINT('Ctrl Pts',(0.17584574554195,-0.183069898264903,
-0.111881629709996));
#52572=CARTESIAN_POINT('Ctrl Pts',(0.249113274073944,0.048798728524302,
-0.0991623568890095));
#52573=CARTESIAN_POINT('Ctrl Pts',(0.0937674461211858,0.235892196932982,
-0.0864430840680236));
#52574=CARTESIAN_POINT('Ctrl Pts',(-0.147602831630382,0.206505907852829,
-0.0737238112470377));
#52575=CARTESIAN_POINT('Ctrl Pts',(-0.253566226457987,-0.0123627143772766,
-0.0610045384260517));
#52576=CARTESIAN_POINT('Ctrl Pts',(-0.126760550998478,-0.219925029716766,
-0.0482852656050658));
#52577=CARTESIAN_POINT('Ctrl Pts',(0.116213473458248,-0.225597061096139,
-0.0355659927840799));
#52578=CARTESIAN_POINT('Ctrl Pts',(0.252840833129579,-0.0243895398283461,
-0.0228467199630935));
#52579=CARTESIAN_POINT('Ctrl Pts',(0.156854624655317,0.199487263968605,
-0.0101274471421078));
#52580=CARTESIAN_POINT('Ctrl Pts',(-0.00221290875354078,0.226244402213306,
-0.00164793192811709));
#52581=CARTESIAN_POINT('Ctrl Pts',(-0.0698093673657148,0.202998596068486,
0.00259182567887824));
#52582=CARTESIAN_POINT('Ctrl Pts',(0.0326814423280649,0.196779569448552,
-1.51495));
#52583=CARTESIAN_POINT('Ctrl Pts',(-0.0328441439546247,0.207662155862942,
-1.51071024239301));
#52584=CARTESIAN_POINT('Ctrl Pts',(-0.174482908049702,0.158625293378044,
-1.50223072717901));
#52585=CARTESIAN_POINT('Ctrl Pts',(-0.227933689275854,-0.061320949657441,
-1.48951145435803));
#52586=CARTESIAN_POINT('Ctrl Pts',(-0.0717210652972735,-0.224640326086787,
-1.47679218153704));
#52587=CARTESIAN_POINT('Ctrl Pts',(0.150056091147136,-0.181992142895108,
-1.46407290871606));
#52588=CARTESIAN_POINT('Ctrl Pts',(0.234263183139456,0.0277545022598852,
-1.45135363589507));
#52589=CARTESIAN_POINT('Ctrl Pts',(0.103427579470953,0.211984146348435,
-1.43863436307408));
#52590=CARTESIAN_POINT('Ctrl Pts',(-0.122283649797262,0.201709159043015,
-1.4259150902531));
#52591=CARTESIAN_POINT('Ctrl Pts',(-0.235798710471342,0.00632031506446229,
-1.41319581743211));
#52592=CARTESIAN_POINT('Ctrl Pts',(-0.132920511685779,-0.194861544684569,
-1.40047654461113));
#52593=CARTESIAN_POINT('Ctrl Pts',(0.0919285341003431,-0.217230095550597,
-1.38775727179014));
#52594=CARTESIAN_POINT('Ctrl Pts',(0.232421027333792,-0.0402530662671006,
-1.37503799896916));
#52595=CARTESIAN_POINT('Ctrl Pts',(0.159628279467637,0.173661654101238,
-1.36231872614817));
#52596=CARTESIAN_POINT('Ctrl Pts',(-0.059648436931805,0.228214293208638,
-1.34959945332718));
#52597=CARTESIAN_POINT('Ctrl Pts',(-0.224188475417309,0.0733432011409307,
-1.3368801805062));
#52598=CARTESIAN_POINT('Ctrl Pts',(-0.182999188568635,-0.148831974728763,
-1.32416090768521));
#52599=CARTESIAN_POINT('Ctrl Pts',(0.0261212891997552,-0.23442986171762,
-1.31144163486423));
#52600=CARTESIAN_POINT('Ctrl Pts',(0.211271323804121,-0.104900464490951,
-1.29872236204324));
#52601=CARTESIAN_POINT('Ctrl Pts',(0.202545781291298,0.120892023328345,
-1.28600308922225));
#52602=CARTESIAN_POINT('Ctrl Pts',(0.00795180094256099,0.2357465737612,
-1.27328381640127));
#52603=CARTESIAN_POINT('Ctrl Pts',(-0.193939248706097,0.134265577980045,
-1.26056454358028));
#52604=CARTESIAN_POINT('Ctrl Pts',(-0.217859723699137,-0.0904257585137644,
-1.24784527075929));
#52605=CARTESIAN_POINT('Ctrl Pts',(-0.0418587330474375,-0.232136864756142,
-1.23512599793831));
#52606=CARTESIAN_POINT('Ctrl Pts',(0.172554404057684,-0.16082492044269,
-1.22240672511732));
#52607=CARTESIAN_POINT('Ctrl Pts',(0.228621017531538,0.0580698516161886,
-1.20968745229634));
#52608=CARTESIAN_POINT('Ctrl Pts',(0.0748909390303039,0.223676160212552,
-1.19696817947535));
#52609=CARTESIAN_POINT('Ctrl Pts',(-0.147563666640709,0.18402348127975,
-1.18424890665437));
#52610=CARTESIAN_POINT('Ctrl Pts',(-0.234604785311441,-0.0245004505269651,
-1.17152963383338));
#52611=CARTESIAN_POINT('Ctrl Pts',(-0.106358138767262,-0.21054126364045,
-1.15881036101239));
#52612=CARTESIAN_POINT('Ctrl Pts',(0.11948927064294,-0.203376477437402,
-1.14609108819141));
#52613=CARTESIAN_POINT('Ctrl Pts',(0.23568598380503,-0.00958093997281493,
-1.13337181537042));
#52614=CARTESIAN_POINT('Ctrl Pts',(0.13560275754475,0.193006656674328,-1.12065254254944));
#52615=CARTESIAN_POINT('Ctrl Pts',(-0.0889178905577564,0.218479486708672,
-1.10793326972845));
#52616=CARTESIAN_POINT('Ctrl Pts',(-0.231842019113515,0.0434621162283831,
-1.09521399690746));
#52617=CARTESIAN_POINT('Ctrl Pts',(-0.162013666417545,-0.171438762442514,
-1.08249472408648));
#52618=CARTESIAN_POINT('Ctrl Pts',(0.0564883808015244,-0.229016899394345,
-1.06977545126549));
#52619=CARTESIAN_POINT('Ctrl Pts',(0.223153219116496,-0.0764350585250314,
-1.0570561784445));
#52620=CARTESIAN_POINT('Ctrl Pts',(0.1850389529013,0.146288288263266,-1.04433690562352));
#52621=CARTESIAN_POINT('Ctrl Pts',(-0.022878425401603,0.234768513700057,
-1.03161763280253));
#52622=CARTESIAN_POINT('Ctrl Pts',(-0.209801154891635,0.107810726645952,
-1.01889835998155));
#52623=CARTESIAN_POINT('Ctrl Pts',(-0.204197454343028,-0.118080807134871,
-1.00617908716056));
#52624=CARTESIAN_POINT('Ctrl Pts',(-0.011209623673909,-0.235614137332382,
-0.993459814339576));
#52625=CARTESIAN_POINT('Ctrl Pts',(0.192064846404454,-0.136933458838324,
-0.980740541518589));
#52626=CARTESIAN_POINT('Ctrl Pts',(0.219088812841539,0.0874057747604746,
-0.968021268697603));
#52627=CARTESIAN_POINT('Ctrl Pts',(0.045063423665798,0.231536099175291,
-0.955301995876618));
#52628=CARTESIAN_POINT('Ctrl Pts',(-0.170314931789737,0.163194673268617,
-0.942582723055631));
#52629=CARTESIAN_POINT('Ctrl Pts',(-0.22940184158239,-0.0549042116089614,
-0.929863450234646));
#52630=CARTESIAN_POINT('Ctrl Pts',(-0.0779755269508779,-0.222619618566124,
-0.917144177413659));
#52631=CARTESIAN_POINT('Ctrl Pts',(0.145005922074389,-0.186045585642739,
-0.904424904592673));
#52632=CARTESIAN_POINT('Ctrl Pts',(0.234921027752471,0.0212553074199478,
-0.891705631771688));
#52633=CARTESIAN_POINT('Ctrl Pts',(0.109258164674579,0.209051024455123,
-0.878986358950702));
#52634=CARTESIAN_POINT('Ctrl Pts',(-0.116666703196555,0.20500867722865,
-0.866267086129715));
#52635=CARTESIAN_POINT('Ctrl Pts',(-0.235531036141585,0.0128377719198042,
-0.853547813308731));
#52636=CARTESIAN_POINT('Ctrl Pts',(-0.138257619153505,-0.19111386166314,
-0.840828540487742));
#52637=CARTESIAN_POINT('Ctrl Pts',(0.0858894838017356,-0.219687673632512,
-0.828109267666759));
#52638=CARTESIAN_POINT('Ctrl Pts',(0.23121911931857,-0.0466625785328924,
-0.81538999484577));
#52639=CARTESIAN_POINT('Ctrl Pts',(0.164367884705876,0.169182965605612,
-0.802670722024787));
#52640=CARTESIAN_POINT('Ctrl Pts',(-0.0533174197753734,0.229775825800475,
-0.789951449203798));
#52641=CARTESIAN_POINT('Ctrl Pts',(-0.222075384016159,0.0795122706748416,
-0.777232176382814));
#52642=CARTESIAN_POINT('Ctrl Pts',(-0.187043331437545,-0.143716629304121,
-0.764512903561827));
#52643=CARTESIAN_POINT('Ctrl Pts',(0.0196311741237908,-0.235062320196826,
-0.751793630740842));
#52644=CARTESIAN_POINT('Ctrl Pts',(0.208290908157902,-0.110700383705523,
-0.739074357919856));
#52645=CARTESIAN_POINT('Ctrl Pts',(0.205810107346701,0.115247026372627,
-0.726355085098869));
#52646=CARTESIAN_POINT('Ctrl Pts',(0.0144653069364513,0.235436684204114,
-0.713635812277884));
#52647=CARTESIAN_POINT('Ctrl Pts',(-0.190153747875909,0.139575175237355,
-0.700916539456897));
#52648=CARTESIAN_POINT('Ctrl Pts',(-0.220276040475835,-0.0843690901105478,
-0.688197266635912));
#52649=CARTESIAN_POINT('Ctrl Pts',(-0.0482595044417223,-0.23089109468499,
-0.675477993814925));
#52650=CARTESIAN_POINT('Ctrl Pts',(0.168042917961313,-0.165533244687709,
-0.662758720993941));
#52651=CARTESIAN_POINT('Ctrl Pts',(0.230138834184335,0.0517280810978802,
-0.650039448172953));
#52652=CARTESIAN_POINT('Ctrl Pts',(0.0810452162903746,0.221520541463405,
-0.637320175351968));
#52653=CARTESIAN_POINT('Ctrl Pts',(-0.142420471538835,0.1880321426258,-0.624600902530982));
#52654=CARTESIAN_POINT('Ctrl Pts',(-0.235192384283932,-0.018006103094028,
-0.611881629709995));
#52655=CARTESIAN_POINT('Ctrl Pts',(-0.112137314847476,-0.207520842308891,
-0.599162356889011));
#52656=CARTESIAN_POINT('Ctrl Pts',(0.113821844477603,-0.206601706414806,
-0.586443084068023));
#52657=CARTESIAN_POINT('Ctrl Pts',(0.235331086026933,-0.0160921509804536,
-0.573723811247038));
#52658=CARTESIAN_POINT('Ctrl Pts',(0.140886064153414,0.189184550905072,
-0.561004538426052));
#52659=CARTESIAN_POINT('Ctrl Pts',(-0.0828446663124362,0.22085388526665,
-0.548285265605067));
#52660=CARTESIAN_POINT('Ctrl Pts',(-0.230552040943494,0.0498541251110027,
-0.535565992784079));
#52661=CARTESIAN_POINT('Ctrl Pts',(-0.16669069754769,-0.16689484331416,
-0.522846719963095));
#52662=CARTESIAN_POINT('Ctrl Pts',(0.0501362714953425,-0.230490849393937,
-0.510127447142107));
#52663=CARTESIAN_POINT('Ctrl Pts',(0.220955117411352,-0.0825742905723761,
-0.497408174321123));
#52664=CARTESIAN_POINT('Ctrl Pts',(0.189011971974381,0.141117510692855,
-0.484688901500136));
#52665=CARTESIAN_POINT('Ctrl Pts',(-0.0163801719563586,0.235311213800938,
-0.47196962867915));
#52666=CARTESIAN_POINT('Ctrl Pts',(-0.206740863692295,0.113568889461726,
-0.459250355858164));
#52667=CARTESIAN_POINT('Ctrl Pts',(-0.207383436620149,-0.112391225588995,
-0.446531083037178));
#52668=CARTESIAN_POINT('Ctrl Pts',(-0.0177182263414914,-0.235214246654171,
-0.433811810216192));
#52669=CARTESIAN_POINT('Ctrl Pts',(0.188206317046981,-0.142190223283767,
-0.421092537395206));
#52670=CARTESIAN_POINT('Ctrl Pts',(0.221421180402404,0.081316285225576,
-0.40837326457422));
#52671=CARTESIAN_POINT('Ctrl Pts',(0.051446364370158,0.230201974289577,
-0.395653991753234));
#52672=CARTESIAN_POINT('Ctrl Pts',(-0.165738796506009,0.167840187997636,
-0.382934718932248));
#52673=CARTESIAN_POINT('Ctrl Pts',(-0.230831854612239,-0.048542067005659,
-0.370215446111262));
#52674=CARTESIAN_POINT('Ctrl Pts',(-0.0840994204847348,-0.220379138866998,
-0.357496173290276));
#52675=CARTESIAN_POINT('Ctrl Pts',(0.139807809013192,-0.189982772682906,
-0.344776900469291));
#52676=CARTESIAN_POINT('Ctrl Pts',(0.235418803056905,0.014753458384602,
-0.332057627648304));
#52677=CARTESIAN_POINT('Ctrl Pts',(0.11499503919352,0.205951009552392,-0.319338354827319));
#52678=CARTESIAN_POINT('Ctrl Pts',(-0.110955238097539,0.208155260646928,
-0.306619082006331));
#52679=CARTESIAN_POINT('Ctrl Pts',(-0.235086171564913,0.0193434552971877,
-0.293899809185347));
#52680=CARTESIAN_POINT('Ctrl Pts',(-0.143487590526395,-0.18721909293667,
-0.28118053636436));
#52681=CARTESIAN_POINT('Ctrl Pts',(0.0797840202277238,-0.221977898961698,
-0.268461263543375));
#52682=CARTESIAN_POINT('Ctrl Pts',(0.229840910738551,-0.0530361458245903,
-0.255741990722388));
#52683=CARTESIAN_POINT('Ctrl Pts',(0.168981662475758,0.164574832115758,
-0.243022717901402));
#52684=CARTESIAN_POINT('Ctrl Pts',(-0.0469455463466026,0.231161834775108,
-0.230303445080416));
#52685=CARTESIAN_POINT('Ctrl Pts',(-0.219792628451899,0.0856205308411988,
-0.217584172259431));
#52686=CARTESIAN_POINT('Ctrl Pts',(-0.190944507701513,-0.138491424611743,
-0.204864899438444));
#52687=CARTESIAN_POINT('Ctrl Pts',(0.0131260578517699,-0.235515155392752,
-0.192145626617459));
#52688=CARTESIAN_POINT('Ctrl Pts',(0.205151283752445,-0.116415679756492,
-0.179426353796472));
#52689=CARTESIAN_POINT('Ctrl Pts',(0.208917206173459,0.109513919792018,
-0.166707080975487));
#52690=CARTESIAN_POINT('Ctrl Pts',(0.0209676371933062,0.234946925588856,
-0.1539878081545));
#52691=CARTESIAN_POINT('Ctrl Pts',(-0.186222691262201,0.144777992008589,
-0.141268535333515));
#52692=CARTESIAN_POINT('Ctrl Pts',(-0.222524461233109,-0.078247731236845,
-0.128549262512529));
#52693=CARTESIAN_POINT('Ctrl Pts',(-0.0546225418096208,-0.229469274023813,
-0.115829989691543));
#52694=CARTESIAN_POINT('Ctrl Pts',(0.16340138241606,-0.170114291722319,
-0.103110716870557));
#52695=CARTESIAN_POINT('Ctrl Pts',(0.231483868070962,0.0453453091881316,
-0.0903914440495704));
#52696=CARTESIAN_POINT('Ctrl Pts',(0.0871316520886174,0.219198428493199,
-0.0776721712285846));
#52697=CARTESIAN_POINT('Ctrl Pts',(-0.137157180929212,0.191891766936069,
-0.0649528984075987));
#52698=CARTESIAN_POINT('Ctrl Pts',(-0.235621691099566,-0.0114878219739488,
-0.0522336255866127));
#52699=CARTESIAN_POINT('Ctrl Pts',(-0.117789880017489,-0.204361235882386,
-0.0395143527656268));
#52700=CARTESIAN_POINT('Ctrl Pts',(0.10798920474263,-0.20963186535164,-0.0267950799446408));
#52701=CARTESIAN_POINT('Ctrl Pts',(0.23494763286579,-0.0226635254220135,
-0.0140758071236545));
#52702=CARTESIAN_POINT('Ctrl Pts',(0.14575423720397,0.18536982288884,-0.00135653430266873));
#52703=CARTESIAN_POINT('Ctrl Pts',(-0.00205630422490502,0.210233395022512,
0.00712298091132193));
#52704=CARTESIAN_POINT('Ctrl Pts',(-0.0648690538289269,0.188632662814105,
0.0113627385183173));
#52705=CARTESIAN_POINT('Ctrl Pts',(-0.0796899944392906,0.231730462577249,
-0.0149499999999998));
#52706=CARTESIAN_POINT('Ctrl Pts',(-0.00252611781081202,0.258266416594894,
-0.0191897576069952));
#52707=CARTESIAN_POINT('Ctrl Pts',(0.0882646408735982,0.242994281361514,
-0.0234295152139904));
#52708=CARTESIAN_POINT('Ctrl Pts',(0.151921992565662,0.1927642612833,-0.0276692728209858));
#52709=CARTESIAN_POINT('Ctrl Pts',(0.215579344257725,0.142534241205086,
-0.031909030427981));
#52710=CARTESIAN_POINT('Ctrl Pts',(0.252103288957442,0.0573463362820363,
-0.0361487880349764));
#52711=CARTESIAN_POINT('Ctrl Pts',(0.244371057512688,-0.0235285968368411,
-0.0403885456419717));
#52712=CARTESIAN_POINT('Ctrl Pts',(0.236638826067934,-0.10440352995572,
-0.0446283032489671));
#52713=CARTESIAN_POINT('Ctrl Pts',(0.184650418478711,-0.180965491270427,
-0.0488680608559624));
#52714=CARTESIAN_POINT('Ctrl Pts',(0.112428897375775,-0.218167332727847,
-0.0531078184629578));
#52715=CARTESIAN_POINT('Ctrl Pts',(0.0402073762728397,-0.255369174185266,
-0.0573475760699531));
#52716=CARTESIAN_POINT('Ctrl Pts',(-0.0522472583438086,-0.253210895785397,
-0.0615873336769485));
#52717=CARTESIAN_POINT('Ctrl Pts',(-0.122600143021194,-0.212641736885196,
-0.0658270912839438));
#52718=CARTESIAN_POINT('Ctrl Pts',(-0.19295302769858,-0.172072577984995,
-0.0700668488909392));
#52719=CARTESIAN_POINT('Ctrl Pts',(-0.241204162436703,-0.0930925385844643,
-0.0743066064979345));
#52720=CARTESIAN_POINT('Ctrl Pts',(-0.245169535782081,-0.0119614040724845,
-0.0785463641049298));
#52721=CARTESIAN_POINT('Ctrl Pts',(-0.245363103914123,-0.00800101981856802,
-0.0787533261962178));
#52722=CARTESIAN_POINT('Ctrl Pts',(-0.245451145027683,-0.00403550979405535,
-0.0789602882875058));
#52723=CARTESIAN_POINT('Ctrl Pts',(-0.245435813781494,-6.93175206961383E-5,
-0.0791672503787938));
#52724=CARTESIAN_POINT('Origin',(0.425436949301274,-0.075016012752114,0.04));
#52725=CARTESIAN_POINT('',(0.418820640002835,-0.0722099128071448,0.04));
#52726=CARTESIAN_POINT('',(0.418259909571329,-0.0753899731090502,0.04));
#52727=CARTESIAN_POINT('Origin',(0.,0.,0.04));
#52728=CARTESIAN_POINT('',(0.412634448512115,-0.0727585864424439,0.04));
#52729=CARTESIAN_POINT('',(0.439454987334101,-0.0703797847906986,0.04));
#52730=CARTESIAN_POINT('',(0.412634448512115,-0.0727585864424439,0.04));
#52731=CARTESIAN_POINT('Origin',(0.412634448512115,-0.0727585864424439,
0.04));
#52732=CARTESIAN_POINT('',(0.418259909571329,-0.0753899731090502,0.485));
#52733=CARTESIAN_POINT('',(0.418259909571329,-0.0753899731090502,0.2425));
#52734=CARTESIAN_POINT('',(0.412634448512115,-0.0727585864424439,0.491));
#52735=CARTESIAN_POINT('',(0.412634448512115,-0.0727585864424439,0.04));
#52736=CARTESIAN_POINT('Ctrl Pts',(0.41825990957133,-0.0753899731090502,
0.485));
#52737=CARTESIAN_POINT('Ctrl Pts',(0.415427183327153,-0.0740649265056499,
0.488022849530655));
#52738=CARTESIAN_POINT('Ctrl Pts',(0.412634448512115,-0.0727585864424439,
0.491));
#52739=CARTESIAN_POINT('Origin',(0.439454987334101,-0.0703797847906986,
0.04));
#52740=CARTESIAN_POINT('',(0.418820640002835,-0.0722099128071448,0.485));
#52741=CARTESIAN_POINT('',(0.418820640002835,-0.0722099128071448,0.2425));
#52742=CARTESIAN_POINT('Ctrl Pts',(0.412634448512115,-0.0727585864424439,
0.491));
#52743=CARTESIAN_POINT('Ctrl Pts',(0.415705555425236,-0.0724861998865247,
0.488022849530686));
#52744=CARTESIAN_POINT('Ctrl Pts',(0.418820640002835,-0.0722099128071448,
0.485));
#52745=CARTESIAN_POINT('Origin',(0.405947212179512,-0.147752701916689,0.04));
#52746=CARTESIAN_POINT('',(0.399918693627878,-0.143840322882602,0.04));
#52747=CARTESIAN_POINT('',(0.398814270275285,-0.146874701105371,0.04));
#52748=CARTESIAN_POINT('Origin',(0.,0.,0.04));
#52749=CARTESIAN_POINT('',(0.393731208109296,-0.143306440053456,0.04));
#52750=CARTESIAN_POINT('',(0.420557357253009,-0.145621115434422,0.04));
#52751=CARTESIAN_POINT('',(0.393731208109296,-0.143306440053456,0.04));
#52752=CARTESIAN_POINT('Origin',(0.393731208109296,-0.143306440053456,0.04));
#52753=CARTESIAN_POINT('',(0.398814270275285,-0.146874701105371,0.485));
#52754=CARTESIAN_POINT('',(0.398814270275285,-0.146874701105371,0.2425));
#52755=CARTESIAN_POINT('',(0.393731208109296,-0.143306440053456,0.491));
#52756=CARTESIAN_POINT('',(0.393731208109296,-0.143306440053456,0.04));
#52757=CARTESIAN_POINT('Ctrl Pts',(0.398814270275285,-0.146874701105371,
0.485));
#52758=CARTESIAN_POINT('Ctrl Pts',(0.396254671435792,-0.14507788718706,
0.488022849530738));
#52759=CARTESIAN_POINT('Ctrl Pts',(0.393731208109296,-0.143306440053456,
0.491));
#52760=CARTESIAN_POINT('Origin',(0.420557357253009,-0.145621115434422,0.04));
#52761=CARTESIAN_POINT('',(0.399918693627878,-0.143840322882602,0.485));
#52762=CARTESIAN_POINT('',(0.399918693627878,-0.143840322882602,0.2425));
#52763=CARTESIAN_POINT('Ctrl Pts',(0.393731208109296,-0.143306440053456,
0.491));
#52764=CARTESIAN_POINT('Ctrl Pts',(0.396802957436579,-0.143571483780241,
0.488022849530825));
#52765=CARTESIAN_POINT('Ctrl Pts',(0.399918693627878,-0.143840322882602,
0.485));
#52766=CARTESIAN_POINT('Origin',(0.374122974434878,-0.216,0.04));
#52767=CARTESIAN_POINT('',(0.368865420115662,-0.211100217533986,0.04));
#52768=CARTESIAN_POINT('',(0.367250861186684,-0.21389671563079,0.04));
#52769=CARTESIAN_POINT('Origin',(0.,0.,0.04));
#52770=CARTESIAN_POINT('',(0.36286464418568,-0.2095,0.04));
#52771=CARTESIAN_POINT('',(0.388881304684075,-0.216437822173509,0.04));
#52772=CARTESIAN_POINT('',(0.36286464418568,-0.2095,0.04));
#52773=CARTESIAN_POINT('Origin',(0.36286464418568,-0.2095,0.04));
#52774=CARTESIAN_POINT('',(0.367250861186684,-0.21389671563079,0.485));
#52775=CARTESIAN_POINT('',(0.367250861186684,-0.21389671563079,0.2425));
#52776=CARTESIAN_POINT('',(0.36286464418568,-0.2095,0.491));
#52777=CARTESIAN_POINT('',(0.36286464418568,-0.2095,0.04));
#52778=CARTESIAN_POINT('Ctrl Pts',(0.367250861186684,-0.21389671563079,
0.485));
#52779=CARTESIAN_POINT('Ctrl Pts',(0.365042161867486,-0.211682729679295,
0.488022849530718));
#52780=CARTESIAN_POINT('Ctrl Pts',(0.36286464418568,-0.2095,0.491));
#52781=CARTESIAN_POINT('Origin',(0.388881304684075,-0.216437822173509,0.04));
#52782=CARTESIAN_POINT('',(0.368865420115662,-0.211100217533986,0.485));
#52783=CARTESIAN_POINT('',(0.368865420115662,-0.211100217533986,0.2425));
#52784=CARTESIAN_POINT('Ctrl Pts',(0.36286464418568,-0.2095,0.491));
#52785=CARTESIAN_POINT('Ctrl Pts',(0.365843702378499,-0.210294420790001,
0.488022849530667));
#52786=CARTESIAN_POINT('Ctrl Pts',(0.368865420115662,-0.211100217533986,
0.485));
#52787=CARTESIAN_POINT('Origin',(0.330931199427399,-0.277684247384585,0.04));
#52788=CARTESIAN_POINT('',(0.32660435746814,-0.271945938897464,0.04));
#52789=CARTESIAN_POINT('',(0.324528720518828,-0.274419586688728,0.04));
#52790=CARTESIAN_POINT('Origin',(0.,0.,0.04));
#52791=CARTESIAN_POINT('',(0.320972621666852,-0.26932800845866,0.04));
#52792=CARTESIAN_POINT('',(0.345389290455751,-0.280678175208677,0.04));
#52793=CARTESIAN_POINT('',(0.320972621666852,-0.26932800845866,0.04));
#52794=CARTESIAN_POINT('Origin',(0.320972621666852,-0.26932800845866,0.04));
#52795=CARTESIAN_POINT('',(0.324528720518828,-0.274419586688728,0.485));
#52796=CARTESIAN_POINT('',(0.324528720518828,-0.274419586688728,0.2425));
#52797=CARTESIAN_POINT('',(0.320972621666852,-0.26932800845866,0.491));
#52798=CARTESIAN_POINT('',(0.320972621666852,-0.26932800845866,0.04));
#52799=CARTESIAN_POINT('Ctrl Pts',(0.324528720518828,-0.274419586688728,
0.485));
#52800=CARTESIAN_POINT('Ctrl Pts',(0.322738030931108,-0.271855699546901,
0.488022849530649));
#52801=CARTESIAN_POINT('Ctrl Pts',(0.320972621666852,-0.26932800845866,
0.491));
#52802=CARTESIAN_POINT('Origin',(0.345389290455751,-0.280678175208677,0.04));
#52803=CARTESIAN_POINT('',(0.32660435746814,-0.271945938897464,0.485));
#52804=CARTESIAN_POINT('',(0.32660435746814,-0.271945938897464,0.2425));
#52805=CARTESIAN_POINT('Ctrl Pts',(0.320972621666852,-0.26932800845866,
0.491));
#52806=CARTESIAN_POINT('Ctrl Pts',(0.323768471549298,-0.270627668238139,
0.4880228495307));
#52807=CARTESIAN_POINT('Ctrl Pts',(0.32660435746814,-0.271945938897464,
0.485));
#52808=CARTESIAN_POINT('Origin',(0.277684247384585,-0.330931199427399,0.04));
#52809=CARTESIAN_POINT('',(0.274419586688728,-0.324528720518828,0.04));
#52810=CARTESIAN_POINT('',(0.271945938897464,-0.32660435746814,0.04));
#52811=CARTESIAN_POINT('Origin',(0.,0.,0.04));
#52812=CARTESIAN_POINT('',(0.26932800845866,-0.320972621666852,0.04));
#52813=CARTESIAN_POINT('',(0.291402797412343,-0.33639026392014,0.04));
#52814=CARTESIAN_POINT('',(0.26932800845866,-0.320972621666852,0.04));
#52815=CARTESIAN_POINT('Origin',(0.26932800845866,-0.320972621666852,0.04));
#52816=CARTESIAN_POINT('',(0.271945938897464,-0.32660435746814,0.485));
#52817=CARTESIAN_POINT('',(0.271945938897464,-0.32660435746814,0.2425));
#52818=CARTESIAN_POINT('',(0.26932800845866,-0.320972621666852,0.491));
#52819=CARTESIAN_POINT('',(0.26932800845866,-0.320972621666852,0.04));
#52820=CARTESIAN_POINT('Ctrl Pts',(0.271945938897464,-0.32660435746814,
0.485));
#52821=CARTESIAN_POINT('Ctrl Pts',(0.270627668238179,-0.323768471549385,
0.488022849530608));
#52822=CARTESIAN_POINT('Ctrl Pts',(0.26932800845866,-0.320972621666852,
0.491));
#52823=CARTESIAN_POINT('Origin',(0.291402797412343,-0.33639026392014,0.04));
#52824=CARTESIAN_POINT('',(0.274419586688728,-0.324528720518828,0.485));
#52825=CARTESIAN_POINT('',(0.274419586688728,-0.324528720518828,0.2425));
#52826=CARTESIAN_POINT('Ctrl Pts',(0.26932800845866,-0.320972621666852,
0.491));
#52827=CARTESIAN_POINT('Ctrl Pts',(0.271855699546945,-0.322738030931138,
0.488022849530598));
#52828=CARTESIAN_POINT('Ctrl Pts',(0.274419586688728,-0.324528720518828,
0.485));
#52829=CARTESIAN_POINT('Origin',(0.216,-0.374122974434878,0.04));
#52830=CARTESIAN_POINT('',(0.21389671563079,-0.367250861186684,0.04));
#52831=CARTESIAN_POINT('',(0.211100217533986,-0.368865420115662,0.04));
#52832=CARTESIAN_POINT('Origin',(0.,0.,0.04));
#52833=CARTESIAN_POINT('',(0.2095,-0.36286464418568,0.04));
#52834=CARTESIAN_POINT('',(0.228562177826491,-0.381881304684075,0.04));
#52835=CARTESIAN_POINT('',(0.2095,-0.36286464418568,0.04));
#52836=CARTESIAN_POINT('Origin',(0.2095,-0.36286464418568,0.04));
#52837=CARTESIAN_POINT('',(0.211100217533986,-0.368865420115662,0.485));
#52838=CARTESIAN_POINT('',(0.211100217533986,-0.368865420115662,0.2425));
#52839=CARTESIAN_POINT('',(0.2095,-0.36286464418568,0.491));
#52840=CARTESIAN_POINT('',(0.2095,-0.36286464418568,0.04));
#52841=CARTESIAN_POINT('Ctrl Pts',(0.211100217533986,-0.368865420115662,
0.485));
#52842=CARTESIAN_POINT('Ctrl Pts',(0.210294420789968,-0.365843702378377,
0.488022849530788));
#52843=CARTESIAN_POINT('Ctrl Pts',(0.2095,-0.36286464418568,0.491));
#52844=CARTESIAN_POINT('Origin',(0.228562177826491,-0.381881304684075,0.04));
#52845=CARTESIAN_POINT('',(0.21389671563079,-0.367250861186684,0.485));
#52846=CARTESIAN_POINT('',(0.21389671563079,-0.367250861186684,0.2425));
#52847=CARTESIAN_POINT('Ctrl Pts',(0.2095,-0.36286464418568,0.491));
#52848=CARTESIAN_POINT('Ctrl Pts',(0.211682729679329,-0.36504216186752,
0.488022849530672));
#52849=CARTESIAN_POINT('Ctrl Pts',(0.21389671563079,-0.367250861186684,
0.485));
#52850=CARTESIAN_POINT('Origin',(0.147752701916689,-0.405947212179513,0.04));
#52851=CARTESIAN_POINT('',(0.146874701105371,-0.398814270275285,0.04));
#52852=CARTESIAN_POINT('',(0.143840322882601,-0.399918693627879,0.04));
#52853=CARTESIAN_POINT('Origin',(0.,0.,0.04));
#52854=CARTESIAN_POINT('',(0.143306440053455,-0.393731208109296,0.04));
#52855=CARTESIAN_POINT('',(0.158776812125424,-0.41576907524645,0.04));
#52856=CARTESIAN_POINT('',(0.143306440053455,-0.393731208109296,0.04));
#52857=CARTESIAN_POINT('Origin',(0.143306440053455,-0.393731208109296,0.04));
#52858=CARTESIAN_POINT('',(0.143840322882601,-0.399918693627878,0.485));
#52859=CARTESIAN_POINT('',(0.143840322882601,-0.399918693627878,0.2425));
#52860=CARTESIAN_POINT('',(0.143306440053455,-0.393731208109296,0.491));
#52861=CARTESIAN_POINT('',(0.143306440053455,-0.393731208109296,0.04));
#52862=CARTESIAN_POINT('Ctrl Pts',(0.143840322882601,-0.399918693627879,
0.485));
#52863=CARTESIAN_POINT('Ctrl Pts',(0.143571483780255,-0.396802957436743,
0.488022849530666));
#52864=CARTESIAN_POINT('Ctrl Pts',(0.143306440053455,-0.393731208109296,
0.491));
#52865=CARTESIAN_POINT('Origin',(0.158776812125424,-0.41576907524645,0.04));
#52866=CARTESIAN_POINT('',(0.146874701105371,-0.398814270275285,0.485));
#52867=CARTESIAN_POINT('',(0.146874701105371,-0.398814270275285,0.2425));
#52868=CARTESIAN_POINT('Ctrl Pts',(0.143306440053455,-0.393731208109296,
0.491));
#52869=CARTESIAN_POINT('Ctrl Pts',(0.145077887187091,-0.396254671435837,
0.488022849530685));
#52870=CARTESIAN_POINT('Ctrl Pts',(0.146874701105371,-0.398814270275285,
0.485));
#52871=CARTESIAN_POINT('Origin',(0.0750160127521138,-0.425436949301274,
0.04));
#52872=CARTESIAN_POINT('',(0.07538997310905,-0.418259909571329,0.04));
#52873=CARTESIAN_POINT('',(0.0722099128071446,-0.418820640002835,0.04));
#52874=CARTESIAN_POINT('Origin',(0.,0.,0.04));
#52875=CARTESIAN_POINT('',(0.0727585864424437,-0.412634448512115,0.04));
#52876=CARTESIAN_POINT('',(0.0841670933328693,-0.437023912846764,0.04));
#52877=CARTESIAN_POINT('',(0.0727585864424437,-0.412634448512115,0.04));
#52878=CARTESIAN_POINT('Origin',(0.0727585864424437,-0.412634448512115,
0.04));
#52879=CARTESIAN_POINT('',(0.0722099128071446,-0.418820640002835,0.485));
#52880=CARTESIAN_POINT('',(0.0722099128071446,-0.418820640002835,0.2425));
#52881=CARTESIAN_POINT('',(0.0727585864424437,-0.412634448512115,0.491));
#52882=CARTESIAN_POINT('',(0.0727585864424437,-0.412634448512115,0.04));
#52883=CARTESIAN_POINT('Ctrl Pts',(0.0722099128071446,-0.418820640002835,
0.485));
#52884=CARTESIAN_POINT('Ctrl Pts',(0.0724861998865257,-0.415705555425222,
0.488022849530699));
#52885=CARTESIAN_POINT('Ctrl Pts',(0.0727585864424437,-0.412634448512115,
0.491));
#52886=CARTESIAN_POINT('Origin',(0.0841670933328693,-0.437023912846764,
0.04));
#52887=CARTESIAN_POINT('',(0.07538997310905,-0.418259909571329,0.485));
#52888=CARTESIAN_POINT('',(0.07538997310905,-0.418259909571329,0.2425));
#52889=CARTESIAN_POINT('Ctrl Pts',(0.0727585864424437,-0.412634448512115,
0.491));
#52890=CARTESIAN_POINT('Ctrl Pts',(0.0740649265056506,-0.415427183327155,
0.488022849530653));
#52891=CARTESIAN_POINT('Ctrl Pts',(0.07538997310905,-0.41825990957133,0.485));
#52892=CARTESIAN_POINT('Origin',(-6.93889390390723E-17,-0.432,0.04));
#52893=CARTESIAN_POINT('',(0.00161455892897798,-0.424996933164776,0.04));
#52894=CARTESIAN_POINT('',(-0.00161455892897815,-0.424996933164776,0.04));
#52895=CARTESIAN_POINT('Origin',(0.,0.,0.04));
#52896=CARTESIAN_POINT('',(-9.71445146547012E-17,-0.419,0.04));
#52897=CARTESIAN_POINT('',(0.00699999999999992,-0.445,0.04));
#52898=CARTESIAN_POINT('',(-9.71445146547012E-17,-0.419,0.04));
#52899=CARTESIAN_POINT('Origin',(-9.71445146547012E-17,-0.419,0.04));
#52900=CARTESIAN_POINT('',(-0.00161455892897816,-0.424996933164776,0.485));
#52901=CARTESIAN_POINT('',(-0.00161455892897816,-0.424996933164776,0.2425));
#52902=CARTESIAN_POINT('',(-9.71445146547012E-17,-0.419,0.491));
#52903=CARTESIAN_POINT('',(-9.71445146547012E-17,-0.419,0.04));
#52904=CARTESIAN_POINT('Ctrl Pts',(-0.00161455892897818,-0.424996933164776,
0.485));
#52905=CARTESIAN_POINT('Ctrl Pts',(-0.000801540510914313,-0.42197715046911,
0.48802284953089));
#52906=CARTESIAN_POINT('Ctrl Pts',(-9.71445146547012E-17,-0.419,0.491));
#52907=CARTESIAN_POINT('Origin',(0.00699999999999992,-0.445,0.04));
#52908=CARTESIAN_POINT('',(0.00161455892897797,-0.424996933164776,0.485));
#52909=CARTESIAN_POINT('',(0.00161455892897797,-0.424996933164776,0.2425));
#52910=CARTESIAN_POINT('Ctrl Pts',(-9.71445146547012E-17,-0.419,0.491));
#52911=CARTESIAN_POINT('Ctrl Pts',(0.000801540510959919,-0.42197715046928,
0.48802284953072));
#52912=CARTESIAN_POINT('Ctrl Pts',(0.00161455892897797,-0.424996933164776,
0.485));
#52913=CARTESIAN_POINT('Origin',(-0.0750160127521139,-0.425436949301274,
0.04));
#52914=CARTESIAN_POINT('',(-0.0722099128071448,-0.418820640002835,0.04));
#52915=CARTESIAN_POINT('',(-0.0753899731090502,-0.418259909571329,0.04));
#52916=CARTESIAN_POINT('Origin',(0.,0.,0.04));
#52917=CARTESIAN_POINT('',(-0.0727585864424438,-0.412634448512115,0.04));
#52918=CARTESIAN_POINT('',(-0.0703797847906986,-0.439454987334101,0.04));
#52919=CARTESIAN_POINT('',(-0.0727585864424438,-0.412634448512115,0.04));
#52920=CARTESIAN_POINT('Origin',(-0.0727585864424438,-0.412634448512115,
0.04));
#52921=CARTESIAN_POINT('',(-0.0753899731090502,-0.418259909571329,0.485));
#52922=CARTESIAN_POINT('',(-0.0753899731090502,-0.418259909571329,0.2425));
#52923=CARTESIAN_POINT('',(-0.0727585864424438,-0.412634448512115,0.491));
#52924=CARTESIAN_POINT('',(-0.0727585864424438,-0.412634448512115,0.04));
#52925=CARTESIAN_POINT('Ctrl Pts',(-0.0753899731090501,-0.41825990957133,
0.485));
#52926=CARTESIAN_POINT('Ctrl Pts',(-0.0740649265055902,-0.415427183327025,
0.488022849530791));
#52927=CARTESIAN_POINT('Ctrl Pts',(-0.0727585864424438,-0.412634448512115,
0.491));
#52928=CARTESIAN_POINT('Origin',(-0.0703797847906986,-0.439454987334101,
0.04));
#52929=CARTESIAN_POINT('',(-0.0722099128071448,-0.418820640002835,0.485));
#52930=CARTESIAN_POINT('',(-0.0722099128071448,-0.418820640002835,0.2425));
#52931=CARTESIAN_POINT('Ctrl Pts',(-0.0727585864424438,-0.412634448512115,
0.491));
#52932=CARTESIAN_POINT('Ctrl Pts',(-0.0724861998865248,-0.415705555425234,
0.488022849530688));
#52933=CARTESIAN_POINT('Ctrl Pts',(-0.0722099128071448,-0.418820640002835,
0.485));
#52934=CARTESIAN_POINT('Origin',(-0.147752701916689,-0.405947212179512,
0.04));
#52935=CARTESIAN_POINT('',(-0.143840322882602,-0.399918693627878,0.04));
#52936=CARTESIAN_POINT('',(-0.146874701105371,-0.398814270275285,0.04));
#52937=CARTESIAN_POINT('Origin',(0.,0.,0.04));
#52938=CARTESIAN_POINT('',(-0.143306440053455,-0.393731208109296,0.04));
#52939=CARTESIAN_POINT('',(-0.145621115434422,-0.420557357253009,0.04));
#52940=CARTESIAN_POINT('',(-0.143306440053455,-0.393731208109296,0.04));
#52941=CARTESIAN_POINT('Origin',(-0.143306440053455,-0.393731208109296,
0.04));
#52942=CARTESIAN_POINT('',(-0.146874701105371,-0.398814270275285,0.485));
#52943=CARTESIAN_POINT('',(-0.146874701105371,-0.398814270275285,0.2425));
#52944=CARTESIAN_POINT('',(-0.143306440053455,-0.393731208109296,0.491));
#52945=CARTESIAN_POINT('',(-0.143306440053455,-0.393731208109296,0.04));
#52946=CARTESIAN_POINT('Ctrl Pts',(-0.146874701105371,-0.398814270275285,
0.485));
#52947=CARTESIAN_POINT('Ctrl Pts',(-0.145077887187028,-0.396254671435746,
0.488022849530792));
#52948=CARTESIAN_POINT('Ctrl Pts',(-0.143306440053455,-0.393731208109296,
0.491));
#52949=CARTESIAN_POINT('Origin',(-0.145621115434422,-0.420557357253009,
0.04));
#52950=CARTESIAN_POINT('',(-0.143840322882602,-0.399918693627878,0.485));
#52951=CARTESIAN_POINT('',(-0.143840322882602,-0.399918693627878,0.2425));
#52952=CARTESIAN_POINT('Ctrl Pts',(-0.143306440053455,-0.393731208109296,
0.491));
#52953=CARTESIAN_POINT('Ctrl Pts',(-0.14357148378024,-0.396802957436561,
0.488022849530842));
#52954=CARTESIAN_POINT('Ctrl Pts',(-0.143840322882602,-0.399918693627878,
0.485));
#52955=CARTESIAN_POINT('Origin',(-0.216,-0.374122974434878,0.04));
#52956=CARTESIAN_POINT('',(-0.211100217533986,-0.368865420115662,0.04));
#52957=CARTESIAN_POINT('',(-0.21389671563079,-0.367250861186684,0.04));
#52958=CARTESIAN_POINT('Origin',(0.,0.,0.04));
#52959=CARTESIAN_POINT('',(-0.2095,-0.36286464418568,0.04));
#52960=CARTESIAN_POINT('',(-0.216437822173509,-0.388881304684075,0.04));
#52961=CARTESIAN_POINT('',(-0.2095,-0.36286464418568,0.04));
#52962=CARTESIAN_POINT('Origin',(-0.2095,-0.36286464418568,0.04));
#52963=CARTESIAN_POINT('',(-0.21389671563079,-0.367250861186684,0.485));
#52964=CARTESIAN_POINT('',(-0.21389671563079,-0.367250861186684,0.2425));
#52965=CARTESIAN_POINT('',(-0.2095,-0.36286464418568,0.491));
#52966=CARTESIAN_POINT('',(-0.2095,-0.36286464418568,0.04));
#52967=CARTESIAN_POINT('Ctrl Pts',(-0.21389671563079,-0.367250861186684,
0.485));
#52968=CARTESIAN_POINT('Ctrl Pts',(-0.211682729679295,-0.365042161867486,
0.488022849530718));
#52969=CARTESIAN_POINT('Ctrl Pts',(-0.2095,-0.36286464418568,0.491));
#52970=CARTESIAN_POINT('Origin',(-0.216437822173509,-0.388881304684075,
0.04));
#52971=CARTESIAN_POINT('',(-0.211100217533986,-0.368865420115662,0.485));
#52972=CARTESIAN_POINT('',(-0.211100217533986,-0.368865420115662,0.2425));
#52973=CARTESIAN_POINT('Ctrl Pts',(-0.2095,-0.36286464418568,0.491));
#52974=CARTESIAN_POINT('Ctrl Pts',(-0.210294420790001,-0.365843702378499,
0.488022849530667));
#52975=CARTESIAN_POINT('Ctrl Pts',(-0.211100217533986,-0.368865420115662,
0.485));
#52976=CARTESIAN_POINT('Origin',(-0.277684247384585,-0.330931199427399,
0.04));
#52977=CARTESIAN_POINT('',(-0.271945938897464,-0.32660435746814,0.04));
#52978=CARTESIAN_POINT('',(-0.274419586688728,-0.324528720518828,0.04));
#52979=CARTESIAN_POINT('Origin',(0.,0.,0.04));
#52980=CARTESIAN_POINT('',(-0.26932800845866,-0.320972621666852,0.04));
#52981=CARTESIAN_POINT('',(-0.280678175208677,-0.345389290455751,0.04));
#52982=CARTESIAN_POINT('',(-0.26932800845866,-0.320972621666852,0.04));
#52983=CARTESIAN_POINT('Origin',(-0.26932800845866,-0.320972621666852,0.04));
#52984=CARTESIAN_POINT('',(-0.274419586688728,-0.324528720518828,0.485));
#52985=CARTESIAN_POINT('',(-0.274419586688728,-0.324528720518828,0.2425));
#52986=CARTESIAN_POINT('',(-0.26932800845866,-0.320972621666852,0.491));
#52987=CARTESIAN_POINT('',(-0.26932800845866,-0.320972621666852,0.04));
#52988=CARTESIAN_POINT('Ctrl Pts',(-0.274419586688728,-0.324528720518828,
0.485));
#52989=CARTESIAN_POINT('Ctrl Pts',(-0.27185569954683,-0.322738030931058,
0.488022849530733));
#52990=CARTESIAN_POINT('Ctrl Pts',(-0.26932800845866,-0.320972621666852,
0.491));
#52991=CARTESIAN_POINT('Origin',(-0.280678175208677,-0.345389290455751,
0.04));
#52992=CARTESIAN_POINT('',(-0.271945938897464,-0.32660435746814,0.485));
#52993=CARTESIAN_POINT('',(-0.271945938897464,-0.32660435746814,0.2425));
#52994=CARTESIAN_POINT('Ctrl Pts',(-0.26932800845866,-0.320972621666852,
0.491));
#52995=CARTESIAN_POINT('Ctrl Pts',(-0.270627668238136,-0.323768471549293,
0.488022849530706));
#52996=CARTESIAN_POINT('Ctrl Pts',(-0.271945938897464,-0.32660435746814,
0.485));
#52997=CARTESIAN_POINT('Origin',(-0.330931199427399,-0.277684247384585,
0.04));
#52998=CARTESIAN_POINT('',(-0.324528720518828,-0.274419586688728,0.04));
#52999=CARTESIAN_POINT('',(-0.32660435746814,-0.271945938897464,0.04));
#53000=CARTESIAN_POINT('Origin',(0.,0.,0.04));
#53001=CARTESIAN_POINT('',(-0.320972621666852,-0.26932800845866,0.04));
#53002=CARTESIAN_POINT('',(-0.33639026392014,-0.291402797412343,0.04));
#53003=CARTESIAN_POINT('',(-0.320972621666852,-0.26932800845866,0.04));
#53004=CARTESIAN_POINT('Origin',(-0.320972621666852,-0.26932800845866,0.04));
#53005=CARTESIAN_POINT('',(-0.32660435746814,-0.271945938897464,0.485));
#53006=CARTESIAN_POINT('',(-0.32660435746814,-0.271945938897464,0.2425));
#53007=CARTESIAN_POINT('',(-0.320972621666852,-0.26932800845866,0.491));
#53008=CARTESIAN_POINT('',(-0.320972621666852,-0.26932800845866,0.04));
#53009=CARTESIAN_POINT('Ctrl Pts',(-0.32660435746814,-0.271945938897464,
0.485));
#53010=CARTESIAN_POINT('Ctrl Pts',(-0.32376847154923,-0.270627668238107,
0.488022849530773));
#53011=CARTESIAN_POINT('Ctrl Pts',(-0.320972621666852,-0.26932800845866,
0.491));
#53012=CARTESIAN_POINT('Origin',(-0.33639026392014,-0.291402797412343,0.04));
#53013=CARTESIAN_POINT('',(-0.324528720518828,-0.274419586688728,0.485));
#53014=CARTESIAN_POINT('',(-0.324528720518828,-0.274419586688728,0.2425));
#53015=CARTESIAN_POINT('Ctrl Pts',(-0.320972621666852,-0.26932800845866,
0.491));
#53016=CARTESIAN_POINT('Ctrl Pts',(-0.322738030931081,-0.271855699546863,
0.488022849530694));
#53017=CARTESIAN_POINT('Ctrl Pts',(-0.324528720518828,-0.274419586688728,
0.485));
#53018=CARTESIAN_POINT('Origin',(-0.374122974434878,-0.216,0.04));
#53019=CARTESIAN_POINT('',(-0.367250861186684,-0.21389671563079,0.04));
#53020=CARTESIAN_POINT('',(-0.368865420115662,-0.211100217533986,0.04));
#53021=CARTESIAN_POINT('Origin',(0.,0.,0.04));
#53022=CARTESIAN_POINT('',(-0.36286464418568,-0.2095,0.04));
#53023=CARTESIAN_POINT('',(-0.381881304684075,-0.228562177826491,0.04));
#53024=CARTESIAN_POINT('',(-0.36286464418568,-0.2095,0.04));
#53025=CARTESIAN_POINT('Origin',(-0.36286464418568,-0.2095,0.04));
#53026=CARTESIAN_POINT('',(-0.368865420115662,-0.211100217533986,0.485));
#53027=CARTESIAN_POINT('',(-0.368865420115662,-0.211100217533986,0.2425));
#53028=CARTESIAN_POINT('',(-0.36286464418568,-0.2095,0.491));
#53029=CARTESIAN_POINT('',(-0.36286464418568,-0.2095,0.04));
#53030=CARTESIAN_POINT('Ctrl Pts',(-0.368865420115662,-0.211100217533986,
0.485));
#53031=CARTESIAN_POINT('Ctrl Pts',(-0.365843702378239,-0.210294420789931,
0.488022849530926));
#53032=CARTESIAN_POINT('Ctrl Pts',(-0.36286464418568,-0.2095,0.491));
#53033=CARTESIAN_POINT('Origin',(-0.381881304684075,-0.228562177826491,
0.04));
#53034=CARTESIAN_POINT('',(-0.367250861186684,-0.21389671563079,0.485));
#53035=CARTESIAN_POINT('',(-0.367250861186684,-0.21389671563079,0.2425));
#53036=CARTESIAN_POINT('Ctrl Pts',(-0.36286464418568,-0.2095,0.491));
#53037=CARTESIAN_POINT('Ctrl Pts',(-0.365042161867381,-0.211682729679189,
0.488022849530862));
#53038=CARTESIAN_POINT('Ctrl Pts',(-0.367250861186684,-0.21389671563079,
0.485));
#53039=CARTESIAN_POINT('Origin',(-0.405947212179513,-0.147752701916689,
0.04));
#53040=CARTESIAN_POINT('',(-0.398814270275285,-0.146874701105371,0.04));
#53041=CARTESIAN_POINT('',(-0.399918693627878,-0.143840322882602,0.04));
#53042=CARTESIAN_POINT('Origin',(0.,0.,0.04));
#53043=CARTESIAN_POINT('',(-0.393731208109296,-0.143306440053455,0.04));
#53044=CARTESIAN_POINT('',(-0.41576907524645,-0.158776812125424,0.04));
#53045=CARTESIAN_POINT('',(-0.393731208109296,-0.143306440053455,0.04));
#53046=CARTESIAN_POINT('Origin',(-0.393731208109296,-0.143306440053455,
0.04));
#53047=CARTESIAN_POINT('',(-0.399918693627878,-0.143840322882602,0.485));
#53048=CARTESIAN_POINT('',(-0.399918693627878,-0.143840322882602,0.2425));
#53049=CARTESIAN_POINT('',(-0.393731208109296,-0.143306440053455,0.491));
#53050=CARTESIAN_POINT('',(-0.393731208109296,-0.143306440053455,0.04));
#53051=CARTESIAN_POINT('Ctrl Pts',(-0.399918693627879,-0.143840322882602,
0.485));
#53052=CARTESIAN_POINT('Ctrl Pts',(-0.396802957436534,-0.143571483780237,
0.488022849530868));
#53053=CARTESIAN_POINT('Ctrl Pts',(-0.393731208109296,-0.143306440053455,
0.491));
#53054=CARTESIAN_POINT('Origin',(-0.41576907524645,-0.158776812125424,0.04));
#53055=CARTESIAN_POINT('',(-0.398814270275285,-0.146874701105371,0.485));
#53056=CARTESIAN_POINT('',(-0.398814270275285,-0.146874701105371,0.2425));
#53057=CARTESIAN_POINT('Ctrl Pts',(-0.393731208109296,-0.143306440053455,
0.491));
#53058=CARTESIAN_POINT('Ctrl Pts',(-0.39625467143586,-0.145077887187107,
0.488022849530658));
#53059=CARTESIAN_POINT('Ctrl Pts',(-0.398814270275285,-0.146874701105371,
0.485));
#53060=CARTESIAN_POINT('Origin',(-0.425436949301274,-0.0750160127521138,
0.04));
#53061=CARTESIAN_POINT('',(-0.418259909571329,-0.07538997310905,0.04));
#53062=CARTESIAN_POINT('',(-0.418820640002835,-0.0722099128071447,0.04));
#53063=CARTESIAN_POINT('Origin',(0.,0.,0.04));
#53064=CARTESIAN_POINT('',(-0.412634448512115,-0.0727585864424437,0.04));
#53065=CARTESIAN_POINT('',(-0.437023912846764,-0.0841670933328693,0.04));
#53066=CARTESIAN_POINT('',(-0.412634448512115,-0.0727585864424437,0.04));
#53067=CARTESIAN_POINT('Origin',(-0.412634448512115,-0.0727585864424437,
0.04));
#53068=CARTESIAN_POINT('',(-0.418820640002835,-0.0722099128071447,0.485));
#53069=CARTESIAN_POINT('',(-0.418820640002835,-0.0722099128071447,0.2425));
#53070=CARTESIAN_POINT('',(-0.412634448512115,-0.0727585864424437,0.491));
#53071=CARTESIAN_POINT('',(-0.412634448512115,-0.0727585864424437,0.04));
#53072=CARTESIAN_POINT('Ctrl Pts',(-0.418820640002835,-0.0722099128071447,
0.485));
#53073=CARTESIAN_POINT('Ctrl Pts',(-0.415705555425184,-0.0724861998865291,
0.488022849530736));
#53074=CARTESIAN_POINT('Ctrl Pts',(-0.412634448512115,-0.0727585864424437,
0.491));
#53075=CARTESIAN_POINT('Origin',(-0.437023912846764,-0.0841670933328693,
0.04));
#53076=CARTESIAN_POINT('',(-0.418259909571329,-0.07538997310905,0.485));
#53077=CARTESIAN_POINT('',(-0.418259909571329,-0.07538997310905,0.2425));
#53078=CARTESIAN_POINT('Ctrl Pts',(-0.412634448512115,-0.0727585864424437,
0.491));
#53079=CARTESIAN_POINT('Ctrl Pts',(-0.415427183326978,-0.0740649265055678,
0.488022849530841));
#53080=CARTESIAN_POINT('Ctrl Pts',(-0.41825990957133,-0.0753899731090501,
0.485));
#53081=CARTESIAN_POINT('Origin',(-0.432,5.55111512312578E-17,0.04));
#53082=CARTESIAN_POINT('',(-0.424996933164776,-0.00161455892897799,0.04));
#53083=CARTESIAN_POINT('',(-0.425,-5.20474889637625E-17,0.04));
#53084=CARTESIAN_POINT('Origin',(0.,0.,0.04));
#53085=CARTESIAN_POINT('',(-0.419,5.55111512312578E-17,0.04));
#53086=CARTESIAN_POINT('',(-0.445,-0.00699999999999995,0.04));
#53087=CARTESIAN_POINT('',(-0.424996933164776,0.0016145589289781,0.04));
#53088=CARTESIAN_POINT('',(-0.419,5.55111512312578E-17,0.04));
#53089=CARTESIAN_POINT('Origin',(0.,0.,0.04));
#53090=CARTESIAN_POINT('Origin',(-0.419,5.55111512312578E-17,0.04));
#53091=CARTESIAN_POINT('',(-0.424996933164776,0.0016145589289781,0.485));
#53092=CARTESIAN_POINT('',(-0.424996933164776,0.0016145589289781,0.2425));
#53093=CARTESIAN_POINT('',(-0.419,5.55111512312578E-17,0.491));
#53094=CARTESIAN_POINT('',(-0.419,5.55111512312578E-17,0.04));
#53095=CARTESIAN_POINT('Ctrl Pts',(-0.424996933164776,0.00161455892897809,
0.485));
#53096=CARTESIAN_POINT('Ctrl Pts',(-0.421977150469231,0.000801540510946881,
0.488022849530769));
#53097=CARTESIAN_POINT('Ctrl Pts',(-0.419,5.55111512312578E-17,0.491));
#53098=CARTESIAN_POINT('Origin',(-0.445,-0.00699999999999995,0.04));
#53099=CARTESIAN_POINT('',(-0.424996933164776,-0.00161455892897801,0.485));
#53100=CARTESIAN_POINT('',(-0.424996933164776,-0.00161455892897801,0.2425));
#53101=CARTESIAN_POINT('Ctrl Pts',(-0.419,5.55111512312578E-17,0.491));
#53102=CARTESIAN_POINT('Ctrl Pts',(-0.421977150469289,-0.000801540510962467,
0.488022849530711));
#53103=CARTESIAN_POINT('Ctrl Pts',(-0.424996933164776,-0.001614558928978,
0.485));
#53104=CARTESIAN_POINT('Origin',(-0.425436949301274,0.0750160127521141,
0.04));
#53105=CARTESIAN_POINT('',(-0.418820640002835,0.072209912807145,0.04));
#53106=CARTESIAN_POINT('',(-0.418259909571329,0.0753899731090504,0.04));
#53107=CARTESIAN_POINT('Origin',(0.,0.,0.04));
#53108=CARTESIAN_POINT('',(-0.412634448512115,0.072758586442444,0.04));
#53109=CARTESIAN_POINT('',(-0.439454987334101,0.0703797847906988,0.04));
#53110=CARTESIAN_POINT('',(-0.412634448512115,0.072758586442444,0.04));
#53111=CARTESIAN_POINT('Origin',(-0.412634448512115,0.072758586442444,0.04));
#53112=CARTESIAN_POINT('',(-0.418259909571329,0.0753899731090503,0.485));
#53113=CARTESIAN_POINT('',(-0.418259909571329,0.0753899731090503,0.2425));
#53114=CARTESIAN_POINT('',(-0.412634448512115,0.072758586442444,0.491));
#53115=CARTESIAN_POINT('',(-0.412634448512115,0.072758586442444,0.04));
#53116=CARTESIAN_POINT('Ctrl Pts',(-0.418259909571329,0.0753899731090504,
0.485));
#53117=CARTESIAN_POINT('Ctrl Pts',(-0.415427183327084,0.0740649265056179,
0.488022849530728));
#53118=CARTESIAN_POINT('Ctrl Pts',(-0.412634448512115,0.072758586442444,
0.491));
#53119=CARTESIAN_POINT('Origin',(-0.439454987334101,0.0703797847906988,
0.04));
#53120=CARTESIAN_POINT('',(-0.418820640002835,0.072209912807145,0.485));
#53121=CARTESIAN_POINT('',(-0.418820640002835,0.072209912807145,0.2425));
#53122=CARTESIAN_POINT('Ctrl Pts',(-0.412634448512115,0.072758586442444,
0.491));
#53123=CARTESIAN_POINT('Ctrl Pts',(-0.415705555425073,0.0724861998865393,
0.488022849530844));
#53124=CARTESIAN_POINT('Ctrl Pts',(-0.418820640002835,0.072209912807145,
0.485));
#53125=CARTESIAN_POINT('Origin',(-0.405947212179513,0.147752701916689,0.04));
#53126=CARTESIAN_POINT('',(-0.399918693627878,0.143840322882602,0.04));
#53127=CARTESIAN_POINT('',(-0.398814270275285,0.146874701105371,0.04));
#53128=CARTESIAN_POINT('Origin',(0.,0.,0.04));
#53129=CARTESIAN_POINT('',(-0.393731208109296,0.143306440053455,0.04));
#53130=CARTESIAN_POINT('',(-0.420557357253009,0.145621115434421,0.04));
#53131=CARTESIAN_POINT('',(-0.393731208109296,0.143306440053455,0.04));
#53132=CARTESIAN_POINT('Origin',(-0.393731208109296,0.143306440053455,0.04));
#53133=CARTESIAN_POINT('',(-0.398814270275285,0.146874701105371,0.485));
#53134=CARTESIAN_POINT('',(-0.398814270275285,0.146874701105371,0.2425));
#53135=CARTESIAN_POINT('',(-0.393731208109296,0.143306440053455,0.491));
#53136=CARTESIAN_POINT('',(-0.393731208109296,0.143306440053455,0.04));
#53137=CARTESIAN_POINT('Ctrl Pts',(-0.398814270275285,0.146874701105371,
0.485));
#53138=CARTESIAN_POINT('Ctrl Pts',(-0.396254671435729,0.145077887187016,
0.488022849530812));
#53139=CARTESIAN_POINT('Ctrl Pts',(-0.393731208109296,0.143306440053455,
0.491));
#53140=CARTESIAN_POINT('Origin',(-0.420557357253009,0.145621115434421,0.04));
#53141=CARTESIAN_POINT('',(-0.399918693627878,0.143840322882602,0.485));
#53142=CARTESIAN_POINT('',(-0.399918693627878,0.143840322882602,0.2425));
#53143=CARTESIAN_POINT('Ctrl Pts',(-0.393731208109296,0.143306440053455,
0.491));
#53144=CARTESIAN_POINT('Ctrl Pts',(-0.396802957436554,0.143571483780239,
0.488022849530849));
#53145=CARTESIAN_POINT('Ctrl Pts',(-0.399918693627878,0.143840322882602,
0.485));
#53146=CARTESIAN_POINT('Origin',(-0.374122974434878,0.216,0.04));
#53147=CARTESIAN_POINT('',(-0.368865420115662,0.211100217533986,0.04));
#53148=CARTESIAN_POINT('',(-0.367250861186684,0.21389671563079,0.04));
#53149=CARTESIAN_POINT('Origin',(0.,0.,0.04));
#53150=CARTESIAN_POINT('',(-0.36286464418568,0.2095,0.04));
#53151=CARTESIAN_POINT('',(-0.388881304684075,0.216437822173509,0.04));
#53152=CARTESIAN_POINT('',(-0.36286464418568,0.2095,0.04));
#53153=CARTESIAN_POINT('Origin',(-0.36286464418568,0.2095,0.04));
#53154=CARTESIAN_POINT('',(-0.367250861186684,0.21389671563079,0.485));
#53155=CARTESIAN_POINT('',(-0.367250861186684,0.21389671563079,0.2425));
#53156=CARTESIAN_POINT('',(-0.36286464418568,0.2095,0.491));
#53157=CARTESIAN_POINT('',(-0.36286464418568,0.2095,0.04));
#53158=CARTESIAN_POINT('Ctrl Pts',(-0.367250861186684,0.21389671563079,
0.485));
#53159=CARTESIAN_POINT('Ctrl Pts',(-0.365042161867489,0.211682729679298,
0.488022849530715));
#53160=CARTESIAN_POINT('Ctrl Pts',(-0.36286464418568,0.2095,0.491));
#53161=CARTESIAN_POINT('Origin',(-0.388881304684075,0.216437822173509,0.04));
#53162=CARTESIAN_POINT('',(-0.368865420115662,0.211100217533986,0.485));
#53163=CARTESIAN_POINT('',(-0.368865420115662,0.211100217533986,0.2425));
#53164=CARTESIAN_POINT('Ctrl Pts',(-0.36286464418568,0.2095,0.491));
#53165=CARTESIAN_POINT('Ctrl Pts',(-0.365843702378652,0.210294420790042,
0.488022849530513));
#53166=CARTESIAN_POINT('Ctrl Pts',(-0.368865420115662,0.211100217533986,
0.485));
#53167=CARTESIAN_POINT('Origin',(-0.330931199427399,0.277684247384585,0.04));
#53168=CARTESIAN_POINT('',(-0.32660435746814,0.271945938897464,0.04));
#53169=CARTESIAN_POINT('',(-0.324528720518828,0.274419586688728,0.04));
#53170=CARTESIAN_POINT('Origin',(0.,0.,0.04));
#53171=CARTESIAN_POINT('',(-0.320972621666852,0.26932800845866,0.04));
#53172=CARTESIAN_POINT('',(-0.345389290455751,0.280678175208677,0.04));
#53173=CARTESIAN_POINT('',(-0.320972621666852,0.26932800845866,0.04));
#53174=CARTESIAN_POINT('Origin',(-0.320972621666852,0.26932800845866,0.04));
#53175=CARTESIAN_POINT('',(-0.324528720518828,0.274419586688728,0.485));
#53176=CARTESIAN_POINT('',(-0.324528720518828,0.274419586688728,0.2425));
#53177=CARTESIAN_POINT('',(-0.320972621666852,0.26932800845866,0.491));
#53178=CARTESIAN_POINT('',(-0.320972621666852,0.26932800845866,0.04));
#53179=CARTESIAN_POINT('Ctrl Pts',(-0.324528720518828,0.274419586688728,
0.485));
#53180=CARTESIAN_POINT('Ctrl Pts',(-0.322738030931058,0.27185569954683,
0.488022849530733));
#53181=CARTESIAN_POINT('Ctrl Pts',(-0.320972621666852,0.26932800845866,
0.491));
#53182=CARTESIAN_POINT('Origin',(-0.345389290455751,0.280678175208677,0.04));
#53183=CARTESIAN_POINT('',(-0.32660435746814,0.271945938897464,0.485));
#53184=CARTESIAN_POINT('',(-0.32660435746814,0.271945938897464,0.2425));
#53185=CARTESIAN_POINT('Ctrl Pts',(-0.320972621666852,0.26932800845866,
0.491));
#53186=CARTESIAN_POINT('Ctrl Pts',(-0.323768471549293,0.270627668238136,
0.488022849530706));
#53187=CARTESIAN_POINT('Ctrl Pts',(-0.32660435746814,0.271945938897464,
0.485));
#53188=CARTESIAN_POINT('Origin',(-0.277684247384585,0.330931199427399,0.04));
#53189=CARTESIAN_POINT('',(-0.274419586688728,0.324528720518828,0.04));
#53190=CARTESIAN_POINT('',(-0.271945938897464,0.32660435746814,0.04));
#53191=CARTESIAN_POINT('Origin',(0.,0.,0.04));
#53192=CARTESIAN_POINT('',(-0.26932800845866,0.320972621666852,0.04));
#53193=CARTESIAN_POINT('',(-0.291402797412343,0.336390263920139,0.04));
#53194=CARTESIAN_POINT('',(-0.26932800845866,0.320972621666852,0.04));
#53195=CARTESIAN_POINT('Origin',(-0.26932800845866,0.320972621666852,0.04));
#53196=CARTESIAN_POINT('',(-0.271945938897464,0.32660435746814,0.485));
#53197=CARTESIAN_POINT('',(-0.271945938897464,0.32660435746814,0.2425));
#53198=CARTESIAN_POINT('',(-0.26932800845866,0.320972621666852,0.491));
#53199=CARTESIAN_POINT('',(-0.26932800845866,0.320972621666852,0.04));
#53200=CARTESIAN_POINT('Ctrl Pts',(-0.271945938897464,0.32660435746814,
0.485));
#53201=CARTESIAN_POINT('Ctrl Pts',(-0.270627668238091,0.323768471549197,
0.488022849530808));
#53202=CARTESIAN_POINT('Ctrl Pts',(-0.26932800845866,0.320972621666852,
0.491));
#53203=CARTESIAN_POINT('Origin',(-0.291402797412343,0.336390263920139,0.04));
#53204=CARTESIAN_POINT('',(-0.274419586688728,0.324528720518828,0.485));
#53205=CARTESIAN_POINT('',(-0.274419586688728,0.324528720518828,0.2425));
#53206=CARTESIAN_POINT('Ctrl Pts',(-0.26932800845866,0.320972621666852,
0.491));
#53207=CARTESIAN_POINT('Ctrl Pts',(-0.271855699546817,0.322738030931049,
0.488022849530749));
#53208=CARTESIAN_POINT('Ctrl Pts',(-0.274419586688728,0.324528720518828,
0.485));
#53209=CARTESIAN_POINT('Origin',(-0.216,0.374122974434878,0.04));
#53210=CARTESIAN_POINT('',(-0.21389671563079,0.367250861186684,0.04));
#53211=CARTESIAN_POINT('',(-0.211100217533986,0.368865420115662,0.04));
#53212=CARTESIAN_POINT('Origin',(0.,0.,0.04));
#53213=CARTESIAN_POINT('',(-0.2095,0.36286464418568,0.04));
#53214=CARTESIAN_POINT('',(-0.228562177826491,0.381881304684075,0.04));
#53215=CARTESIAN_POINT('',(-0.2095,0.36286464418568,0.04));
#53216=CARTESIAN_POINT('Origin',(-0.2095,0.36286464418568,0.04));
#53217=CARTESIAN_POINT('',(-0.211100217533986,0.368865420115662,0.485));
#53218=CARTESIAN_POINT('',(-0.211100217533986,0.368865420115662,0.2425));
#53219=CARTESIAN_POINT('',(-0.2095,0.36286464418568,0.491));
#53220=CARTESIAN_POINT('',(-0.2095,0.36286464418568,0.04));
#53221=CARTESIAN_POINT('Ctrl Pts',(-0.211100217533986,0.368865420115662,
0.485));
#53222=CARTESIAN_POINT('Ctrl Pts',(-0.210294420789963,0.365843702378358,
0.488022849530807));
#53223=CARTESIAN_POINT('Ctrl Pts',(-0.2095,0.36286464418568,0.491));
#53224=CARTESIAN_POINT('Origin',(-0.228562177826491,0.381881304684075,0.04));
#53225=CARTESIAN_POINT('',(-0.21389671563079,0.367250861186684,0.485));
#53226=CARTESIAN_POINT('',(-0.21389671563079,0.367250861186684,0.2425));
#53227=CARTESIAN_POINT('Ctrl Pts',(-0.2095,0.36286464418568,0.491));
#53228=CARTESIAN_POINT('Ctrl Pts',(-0.211682729679243,0.365042161867435,
0.488022849530789));
#53229=CARTESIAN_POINT('Ctrl Pts',(-0.21389671563079,0.367250861186684,
0.485));
#53230=CARTESIAN_POINT('Origin',(-0.147752701916689,0.405947212179513,0.04));
#53231=CARTESIAN_POINT('',(-0.146874701105371,0.398814270275285,0.04));
#53232=CARTESIAN_POINT('',(-0.143840322882602,0.399918693627878,0.04));
#53233=CARTESIAN_POINT('Origin',(0.,0.,0.04));
#53234=CARTESIAN_POINT('',(-0.143306440053455,0.393731208109296,0.04));
#53235=CARTESIAN_POINT('',(-0.158776812125424,0.41576907524645,0.04));
#53236=CARTESIAN_POINT('',(-0.143306440053455,0.393731208109296,0.04));
#53237=CARTESIAN_POINT('Origin',(-0.143306440053455,0.393731208109296,0.04));
#53238=CARTESIAN_POINT('',(-0.143840322882602,0.399918693627878,0.485));
#53239=CARTESIAN_POINT('',(-0.143840322882602,0.399918693627878,0.2425));
#53240=CARTESIAN_POINT('',(-0.143306440053455,0.393731208109296,0.491));
#53241=CARTESIAN_POINT('',(-0.143306440053455,0.393731208109296,0.04));
#53242=CARTESIAN_POINT('Ctrl Pts',(-0.143840322882602,0.399918693627879,
0.485));
#53243=CARTESIAN_POINT('Ctrl Pts',(-0.143571483780237,0.396802957436534,
0.488022849530868));
#53244=CARTESIAN_POINT('Ctrl Pts',(-0.143306440053455,0.393731208109296,
0.491));
#53245=CARTESIAN_POINT('Origin',(-0.158776812125424,0.41576907524645,0.04));
#53246=CARTESIAN_POINT('',(-0.146874701105371,0.398814270275285,0.485));
#53247=CARTESIAN_POINT('',(-0.146874701105371,0.398814270275285,0.2425));
#53248=CARTESIAN_POINT('Ctrl Pts',(-0.143306440053455,0.393731208109296,
0.491));
#53249=CARTESIAN_POINT('Ctrl Pts',(-0.145077887187107,0.39625467143586,
0.488022849530658));
#53250=CARTESIAN_POINT('Ctrl Pts',(-0.146874701105371,0.398814270275285,
0.485));
#53251=CARTESIAN_POINT('Origin',(-0.0750160127521139,0.425436949301274,
0.04));
#53252=CARTESIAN_POINT('',(-0.0753899731090501,0.418259909571329,0.04));
#53253=CARTESIAN_POINT('',(-0.0722099128071448,0.418820640002835,0.04));
#53254=CARTESIAN_POINT('Origin',(0.,0.,0.04));
#53255=CARTESIAN_POINT('',(-0.0727585864424438,0.412634448512115,0.04));
#53256=CARTESIAN_POINT('',(-0.0841670933328695,0.437023912846764,0.04));
#53257=CARTESIAN_POINT('',(-0.0727585864424438,0.412634448512115,0.04));
#53258=CARTESIAN_POINT('Origin',(-0.0727585864424438,0.412634448512115,
0.04));
#53259=CARTESIAN_POINT('',(-0.0722099128071448,0.418820640002835,0.485));
#53260=CARTESIAN_POINT('',(-0.0722099128071448,0.418820640002835,0.2425));
#53261=CARTESIAN_POINT('',(-0.0727585864424438,0.412634448512115,0.491));
#53262=CARTESIAN_POINT('',(-0.0727585864424438,0.412634448512115,0.04));
#53263=CARTESIAN_POINT('Ctrl Pts',(-0.0722099128071449,0.418820640002835,
0.485));
#53264=CARTESIAN_POINT('Ctrl Pts',(-0.0724861998865278,0.4157055554252,
0.488022849530721));
#53265=CARTESIAN_POINT('Ctrl Pts',(-0.0727585864424438,0.412634448512115,
0.491));
#53266=CARTESIAN_POINT('Origin',(-0.0841670933328695,0.437023912846764,
0.04));
#53267=CARTESIAN_POINT('',(-0.0753899731090501,0.418259909571329,0.485));
#53268=CARTESIAN_POINT('',(-0.0753899731090501,0.418259909571329,0.2425));
#53269=CARTESIAN_POINT('Ctrl Pts',(-0.0727585864424438,0.412634448512115,
0.491));
#53270=CARTESIAN_POINT('Ctrl Pts',(-0.074064926505637,0.415427183327125,
0.488022849530684));
#53271=CARTESIAN_POINT('Ctrl Pts',(-0.0753899731090501,0.41825990957133,
0.485));
#53272=CARTESIAN_POINT('Origin',(2.77555756156289E-17,0.432,0.04));
#53273=CARTESIAN_POINT('',(-0.00161455892897801,0.424996933164776,0.04));
#53274=CARTESIAN_POINT('',(0.00161455892897809,0.424996933164776,0.04));
#53275=CARTESIAN_POINT('Origin',(0.,0.,0.04));
#53276=CARTESIAN_POINT('',(2.77555756156289E-17,0.419,0.04));
#53277=CARTESIAN_POINT('',(-0.00699999999999998,0.445,0.04));
#53278=CARTESIAN_POINT('',(2.77555756156289E-17,0.419,0.04));
#53279=CARTESIAN_POINT('Origin',(2.77555756156289E-17,0.419,0.04));
#53280=CARTESIAN_POINT('',(0.00161455892897809,0.424996933164776,0.485));
#53281=CARTESIAN_POINT('',(0.00161455892897809,0.424996933164776,0.2425));
#53282=CARTESIAN_POINT('',(2.77555756156289E-17,0.419,0.491));
#53283=CARTESIAN_POINT('',(2.77555756156289E-17,0.419,0.04));
#53284=CARTESIAN_POINT('Ctrl Pts',(0.00161455892897808,0.424996933164776,
0.485));
#53285=CARTESIAN_POINT('Ctrl Pts',(0.000801540510960544,0.421977150469282,
0.488022849530718));
#53286=CARTESIAN_POINT('Ctrl Pts',(2.77555756156289E-17,0.419,0.491));
#53287=CARTESIAN_POINT('Origin',(-0.00699999999999998,0.445,0.04));
#53288=CARTESIAN_POINT('',(-0.00161455892897802,0.424996933164776,0.485));
#53289=CARTESIAN_POINT('',(-0.00161455892897802,0.424996933164776,0.2425));
#53290=CARTESIAN_POINT('Ctrl Pts',(2.77555756156289E-17,0.419,0.491));
#53291=CARTESIAN_POINT('Ctrl Pts',(-0.000801540510964092,0.421977150469295,
0.488022849530705));
#53292=CARTESIAN_POINT('Ctrl Pts',(-0.00161455892897804,0.424996933164776,
0.485));
#53293=CARTESIAN_POINT('Origin',(0.075016012752114,0.425436949301274,0.04));
#53294=CARTESIAN_POINT('',(0.0722099128071449,0.418820640002835,0.04));
#53295=CARTESIAN_POINT('',(0.0753899731090502,0.418259909571329,0.04));
#53296=CARTESIAN_POINT('Origin',(0.,0.,0.04));
#53297=CARTESIAN_POINT('',(0.0727585864424439,0.412634448512115,0.04));
#53298=CARTESIAN_POINT('',(0.0703797847906986,0.439454987334101,0.04));
#53299=CARTESIAN_POINT('',(0.0727585864424439,0.412634448512115,0.04));
#53300=CARTESIAN_POINT('Origin',(0.0727585864424439,0.412634448512115,0.04));
#53301=CARTESIAN_POINT('',(0.0753899731090502,0.418259909571329,0.485));
#53302=CARTESIAN_POINT('',(0.0753899731090502,0.418259909571329,0.2425));
#53303=CARTESIAN_POINT('',(0.0727585864424439,0.412634448512115,0.491));
#53304=CARTESIAN_POINT('',(0.0727585864424439,0.412634448512115,0.04));
#53305=CARTESIAN_POINT('Ctrl Pts',(0.0753899731090502,0.41825990957133,
0.485));
#53306=CARTESIAN_POINT('Ctrl Pts',(0.0740649265056445,0.415427183327141,
0.488022849530667));
#53307=CARTESIAN_POINT('Ctrl Pts',(0.0727585864424439,0.412634448512115,
0.491));
#53308=CARTESIAN_POINT('Origin',(0.0703797847906986,0.439454987334101,0.04));
#53309=CARTESIAN_POINT('',(0.0722099128071449,0.418820640002835,0.485));
#53310=CARTESIAN_POINT('',(0.0722099128071449,0.418820640002835,0.2425));
#53311=CARTESIAN_POINT('Ctrl Pts',(0.0727585864424439,0.412634448512115,
0.491));
#53312=CARTESIAN_POINT('Ctrl Pts',(0.072486199886539,0.415705555425075,
0.488022849530842));
#53313=CARTESIAN_POINT('Ctrl Pts',(0.0722099128071449,0.418820640002835,
0.485));
#53314=CARTESIAN_POINT('Origin',(0.147752701916689,0.405947212179513,0.04));
#53315=CARTESIAN_POINT('',(0.143840322882602,0.399918693627878,0.04));
#53316=CARTESIAN_POINT('',(0.146874701105371,0.398814270275285,0.04));
#53317=CARTESIAN_POINT('Origin',(0.,0.,0.04));
#53318=CARTESIAN_POINT('',(0.143306440053455,0.393731208109296,0.04));
#53319=CARTESIAN_POINT('',(0.145621115434421,0.420557357253009,0.04));
#53320=CARTESIAN_POINT('',(0.143306440053455,0.393731208109296,0.04));
#53321=CARTESIAN_POINT('Origin',(0.143306440053455,0.393731208109296,0.04));
#53322=CARTESIAN_POINT('',(0.146874701105371,0.398814270275285,0.485));
#53323=CARTESIAN_POINT('',(0.146874701105371,0.398814270275285,0.2425));
#53324=CARTESIAN_POINT('',(0.143306440053455,0.393731208109296,0.491));
#53325=CARTESIAN_POINT('',(0.143306440053455,0.393731208109296,0.04));
#53326=CARTESIAN_POINT('Ctrl Pts',(0.146874701105371,0.398814270275285,
0.485));
#53327=CARTESIAN_POINT('Ctrl Pts',(0.145077887187016,0.396254671435729,
0.488022849530812));
#53328=CARTESIAN_POINT('Ctrl Pts',(0.143306440053455,0.393731208109296,
0.491));
#53329=CARTESIAN_POINT('Origin',(0.145621115434421,0.420557357253009,0.04));
#53330=CARTESIAN_POINT('',(0.143840322882602,0.399918693627878,0.485));
#53331=CARTESIAN_POINT('',(0.143840322882602,0.399918693627878,0.2425));
#53332=CARTESIAN_POINT('Ctrl Pts',(0.143306440053455,0.393731208109296,
0.491));
#53333=CARTESIAN_POINT('Ctrl Pts',(0.143571483780239,0.396802957436554,
0.488022849530849));
#53334=CARTESIAN_POINT('Ctrl Pts',(0.143840322882602,0.399918693627878,
0.485));
#53335=CARTESIAN_POINT('Origin',(0.216,0.374122974434878,0.04));
#53336=CARTESIAN_POINT('',(0.211100217533986,0.368865420115662,0.04));
#53337=CARTESIAN_POINT('',(0.21389671563079,0.367250861186684,0.04));
#53338=CARTESIAN_POINT('Origin',(0.,0.,0.04));
#53339=CARTESIAN_POINT('',(0.2095,0.36286464418568,0.04));
#53340=CARTESIAN_POINT('',(0.216437822173509,0.388881304684075,0.04));
#53341=CARTESIAN_POINT('',(0.2095,0.36286464418568,0.04));
#53342=CARTESIAN_POINT('Origin',(0.2095,0.36286464418568,0.04));
#53343=CARTESIAN_POINT('',(0.21389671563079,0.367250861186684,0.485));
#53344=CARTESIAN_POINT('',(0.21389671563079,0.367250861186684,0.2425));
#53345=CARTESIAN_POINT('',(0.2095,0.36286464418568,0.491));
#53346=CARTESIAN_POINT('',(0.2095,0.36286464418568,0.04));
#53347=CARTESIAN_POINT('Ctrl Pts',(0.21389671563079,0.367250861186684,0.485));
#53348=CARTESIAN_POINT('Ctrl Pts',(0.211682729679179,0.36504216186737,0.488022849530877));
#53349=CARTESIAN_POINT('Ctrl Pts',(0.2095,0.36286464418568,0.491));
#53350=CARTESIAN_POINT('Origin',(0.216437822173509,0.388881304684075,0.04));
#53351=CARTESIAN_POINT('',(0.211100217533986,0.368865420115662,0.485));
#53352=CARTESIAN_POINT('',(0.211100217533986,0.368865420115662,0.2425));
#53353=CARTESIAN_POINT('Ctrl Pts',(0.2095,0.36286464418568,0.491));
#53354=CARTESIAN_POINT('Ctrl Pts',(0.21029442079001,0.365843702378533,0.488022849530632));
#53355=CARTESIAN_POINT('Ctrl Pts',(0.211100217533986,0.368865420115662,
0.485));
#53356=CARTESIAN_POINT('Origin',(0.277684247384585,0.330931199427399,0.04));
#53357=CARTESIAN_POINT('',(0.271945938897464,0.32660435746814,0.04));
#53358=CARTESIAN_POINT('',(0.274419586688728,0.324528720518828,0.04));
#53359=CARTESIAN_POINT('Origin',(0.,0.,0.04));
#53360=CARTESIAN_POINT('',(0.26932800845866,0.320972621666852,0.04));
#53361=CARTESIAN_POINT('',(0.280678175208677,0.345389290455751,0.04));
#53362=CARTESIAN_POINT('',(0.26932800845866,0.320972621666852,0.04));
#53363=CARTESIAN_POINT('Origin',(0.26932800845866,0.320972621666852,0.04));
#53364=CARTESIAN_POINT('',(0.274419586688728,0.324528720518828,0.485));
#53365=CARTESIAN_POINT('',(0.274419586688728,0.324528720518828,0.2425));
#53366=CARTESIAN_POINT('',(0.26932800845866,0.320972621666852,0.491));
#53367=CARTESIAN_POINT('',(0.26932800845866,0.320972621666852,0.04));
#53368=CARTESIAN_POINT('Ctrl Pts',(0.274419586688728,0.324528720518828,
0.485));
#53369=CARTESIAN_POINT('Ctrl Pts',(0.271855699546927,0.322738030931126,
0.488022849530619));
#53370=CARTESIAN_POINT('Ctrl Pts',(0.26932800845866,0.320972621666852,0.491));
#53371=CARTESIAN_POINT('Origin',(0.280678175208677,0.345389290455751,0.04));
#53372=CARTESIAN_POINT('',(0.271945938897464,0.32660435746814,0.485));
#53373=CARTESIAN_POINT('',(0.271945938897464,0.32660435746814,0.2425));
#53374=CARTESIAN_POINT('Ctrl Pts',(0.26932800845866,0.320972621666852,0.491));
#53375=CARTESIAN_POINT('Ctrl Pts',(0.270627668238161,0.323768471549347,
0.488022849530649));
#53376=CARTESIAN_POINT('Ctrl Pts',(0.271945938897464,0.32660435746814,0.485));
#53377=CARTESIAN_POINT('Origin',(0.330931199427399,0.277684247384585,0.04));
#53378=CARTESIAN_POINT('',(0.324528720518828,0.274419586688728,0.04));
#53379=CARTESIAN_POINT('',(0.32660435746814,0.271945938897464,0.04));
#53380=CARTESIAN_POINT('Origin',(0.,0.,0.04));
#53381=CARTESIAN_POINT('',(0.320972621666852,0.26932800845866,0.04));
#53382=CARTESIAN_POINT('',(0.33639026392014,0.291402797412343,0.04));
#53383=CARTESIAN_POINT('',(0.320972621666852,0.26932800845866,0.04));
#53384=CARTESIAN_POINT('Origin',(0.320972621666852,0.26932800845866,0.04));
#53385=CARTESIAN_POINT('',(0.32660435746814,0.271945938897464,0.485));
#53386=CARTESIAN_POINT('',(0.32660435746814,0.271945938897464,0.2425));
#53387=CARTESIAN_POINT('',(0.320972621666852,0.26932800845866,0.491));
#53388=CARTESIAN_POINT('',(0.320972621666852,0.26932800845866,0.04));
#53389=CARTESIAN_POINT('Ctrl Pts',(0.32660435746814,0.271945938897464,0.485));
#53390=CARTESIAN_POINT('Ctrl Pts',(0.32376847154923,0.270627668238107,0.488022849530773));
#53391=CARTESIAN_POINT('Ctrl Pts',(0.320972621666852,0.26932800845866,0.491));
#53392=CARTESIAN_POINT('Origin',(0.33639026392014,0.291402797412343,0.04));
#53393=CARTESIAN_POINT('',(0.324528720518828,0.274419586688728,0.485));
#53394=CARTESIAN_POINT('',(0.324528720518828,0.274419586688728,0.2425));
#53395=CARTESIAN_POINT('Ctrl Pts',(0.320972621666852,0.26932800845866,0.491));
#53396=CARTESIAN_POINT('Ctrl Pts',(0.322738030931081,0.271855699546863,
0.488022849530694));
#53397=CARTESIAN_POINT('Ctrl Pts',(0.324528720518828,0.274419586688728,
0.485));
#53398=CARTESIAN_POINT('Origin',(0.374122974434878,0.216,0.04));
#53399=CARTESIAN_POINT('',(0.367250861186684,0.21389671563079,0.04));
#53400=CARTESIAN_POINT('',(0.368865420115662,0.211100217533986,0.04));
#53401=CARTESIAN_POINT('Origin',(0.,0.,0.04));
#53402=CARTESIAN_POINT('',(0.36286464418568,0.2095,0.04));
#53403=CARTESIAN_POINT('',(0.381881304684075,0.228562177826491,0.04));
#53404=CARTESIAN_POINT('',(0.36286464418568,0.2095,0.04));
#53405=CARTESIAN_POINT('Origin',(0.36286464418568,0.2095,0.04));
#53406=CARTESIAN_POINT('',(0.368865420115662,0.211100217533986,0.485));
#53407=CARTESIAN_POINT('',(0.368865420115662,0.211100217533986,0.2425));
#53408=CARTESIAN_POINT('',(0.36286464418568,0.2095,0.491));
#53409=CARTESIAN_POINT('',(0.36286464418568,0.2095,0.04));
#53410=CARTESIAN_POINT('Ctrl Pts',(0.368865420115662,0.211100217533986,
0.485));
#53411=CARTESIAN_POINT('Ctrl Pts',(0.365843702378372,0.210294420789967,
0.488022849530793));
#53412=CARTESIAN_POINT('Ctrl Pts',(0.36286464418568,0.2095,0.491));
#53413=CARTESIAN_POINT('Origin',(0.381881304684075,0.228562177826491,0.04));
#53414=CARTESIAN_POINT('',(0.367250861186684,0.21389671563079,0.485));
#53415=CARTESIAN_POINT('',(0.367250861186684,0.21389671563079,0.2425));
#53416=CARTESIAN_POINT('Ctrl Pts',(0.36286464418568,0.2095,0.491));
#53417=CARTESIAN_POINT('Ctrl Pts',(0.365042161867479,0.211682729679287,
0.488022849530729));
#53418=CARTESIAN_POINT('Ctrl Pts',(0.367250861186684,0.21389671563079,0.485));
#53419=CARTESIAN_POINT('Origin',(0.405947212179513,0.147752701916689,0.04));
#53420=CARTESIAN_POINT('',(0.398814270275285,0.146874701105371,0.04));
#53421=CARTESIAN_POINT('',(0.399918693627878,0.143840322882602,0.04));
#53422=CARTESIAN_POINT('Origin',(0.,0.,0.04));
#53423=CARTESIAN_POINT('',(0.393731208109296,0.143306440053455,0.04));
#53424=CARTESIAN_POINT('',(0.41576907524645,0.158776812125424,0.04));
#53425=CARTESIAN_POINT('',(0.393731208109296,0.143306440053455,0.04));
#53426=CARTESIAN_POINT('Origin',(0.393731208109296,0.143306440053455,0.04));
#53427=CARTESIAN_POINT('',(0.399918693627878,0.143840322882602,0.485));
#53428=CARTESIAN_POINT('',(0.399918693627878,0.143840322882602,0.2425));
#53429=CARTESIAN_POINT('',(0.393731208109296,0.143306440053455,0.491));
#53430=CARTESIAN_POINT('',(0.393731208109296,0.143306440053455,0.04));
#53431=CARTESIAN_POINT('Ctrl Pts',(0.399918693627879,0.143840322882602,
0.485));
#53432=CARTESIAN_POINT('Ctrl Pts',(0.396802957436534,0.143571483780237,
0.488022849530868));
#53433=CARTESIAN_POINT('Ctrl Pts',(0.393731208109296,0.143306440053455,
0.491));
#53434=CARTESIAN_POINT('Origin',(0.41576907524645,0.158776812125424,0.04));
#53435=CARTESIAN_POINT('',(0.398814270275285,0.146874701105371,0.485));
#53436=CARTESIAN_POINT('',(0.398814270275285,0.146874701105371,0.2425));
#53437=CARTESIAN_POINT('Ctrl Pts',(0.393731208109296,0.143306440053455,
0.491));
#53438=CARTESIAN_POINT('Ctrl Pts',(0.39625467143586,0.145077887187107,0.488022849530658));
#53439=CARTESIAN_POINT('Ctrl Pts',(0.398814270275285,0.146874701105371,
0.485));
#53440=CARTESIAN_POINT('Origin',(0.425436949301274,0.0750160127521139,0.04));
#53441=CARTESIAN_POINT('',(0.418259909571329,0.0753899731090502,0.04));
#53442=CARTESIAN_POINT('',(0.418820640002835,0.0722099128071448,0.04));
#53443=CARTESIAN_POINT('Origin',(0.,0.,0.04));
#53444=CARTESIAN_POINT('',(0.412634448512115,0.0727585864424438,0.04));
#53445=CARTESIAN_POINT('',(0.437023912846764,0.0841670933328695,0.04));
#53446=CARTESIAN_POINT('',(0.412634448512115,0.0727585864424438,0.04));
#53447=CARTESIAN_POINT('Origin',(0.412634448512115,0.0727585864424438,0.04));
#53448=CARTESIAN_POINT('',(0.418820640002835,0.0722099128071448,0.485));
#53449=CARTESIAN_POINT('',(0.418820640002835,0.0722099128071448,0.2425));
#53450=CARTESIAN_POINT('',(0.412634448512115,0.0727585864424438,0.491));
#53451=CARTESIAN_POINT('',(0.412634448512115,0.0727585864424438,0.04));
#53452=CARTESIAN_POINT('Ctrl Pts',(0.418820640002835,0.0722099128071448,
0.485));
#53453=CARTESIAN_POINT('Ctrl Pts',(0.415705555425232,0.072486199886525,
0.48802284953069));
#53454=CARTESIAN_POINT('Ctrl Pts',(0.412634448512115,0.0727585864424438,
0.491));
#53455=CARTESIAN_POINT('Origin',(0.437023912846764,0.0841670933328695,0.04));
#53456=CARTESIAN_POINT('',(0.418259909571329,0.0753899731090502,0.485));
#53457=CARTESIAN_POINT('',(0.418259909571329,0.0753899731090502,0.2425));
#53458=CARTESIAN_POINT('Ctrl Pts',(0.412634448512115,0.0727585864424438,
0.491));
#53459=CARTESIAN_POINT('Ctrl Pts',(0.41542718332698,0.074064926505569,0.488022849530839));
#53460=CARTESIAN_POINT('Ctrl Pts',(0.41825990957133,0.0753899731090502,
0.485));
#53461=CARTESIAN_POINT('Origin',(0.,0.,0.2425));
#53462=CARTESIAN_POINT('Origin',(0.,0.,0.485));
#53463=CARTESIAN_POINT('Origin',(0.,0.,0.485));
#53464=CARTESIAN_POINT('Origin',(0.,0.,0.485));
#53465=CARTESIAN_POINT('Origin',(0.,0.,0.485));
#53466=CARTESIAN_POINT('Origin',(0.,0.,0.485));
#53467=CARTESIAN_POINT('Origin',(0.,0.,0.485));
#53468=CARTESIAN_POINT('Origin',(0.,0.,0.485));
#53469=CARTESIAN_POINT('Origin',(0.,0.,0.485));
#53470=CARTESIAN_POINT('Origin',(0.,0.,0.485));
#53471=CARTESIAN_POINT('Origin',(0.,0.,0.485));
#53472=CARTESIAN_POINT('Origin',(0.,0.,0.485));
#53473=CARTESIAN_POINT('Origin',(0.,0.,0.485));
#53474=CARTESIAN_POINT('Origin',(0.,0.,0.485));
#53475=CARTESIAN_POINT('Origin',(0.,0.,0.485));
#53476=CARTESIAN_POINT('Origin',(0.,0.,0.485));
#53477=CARTESIAN_POINT('Origin',(0.,0.,0.485));
#53478=CARTESIAN_POINT('Origin',(0.,0.,0.485));
#53479=CARTESIAN_POINT('',(-0.425,-5.20474889637625E-17,0.));
#53480=CARTESIAN_POINT('',(-0.425,-5.20474889637625E-17,0.2425));
#53481=CARTESIAN_POINT('Origin',(0.,0.,0.));
#53482=CARTESIAN_POINT('Origin',(0.,0.,0.485));
#53483=CARTESIAN_POINT('Origin',(0.,0.,0.485));
#53484=CARTESIAN_POINT('Origin',(0.,0.,0.485));
#53485=CARTESIAN_POINT('Origin',(0.,0.,0.485));
#53486=CARTESIAN_POINT('Origin',(0.,0.,0.485));
#53487=CARTESIAN_POINT('Origin',(0.,0.,0.485));
#53488=CARTESIAN_POINT('Origin',(0.,0.,0.485));
#53489=CARTESIAN_POINT('Origin',(0.,0.,0.485));
#53490=CARTESIAN_POINT('Origin',(0.,0.,0.485));
#53491=CARTESIAN_POINT('Origin',(0.,0.,0.485));
#53492=CARTESIAN_POINT('Origin',(0.,0.,0.485));
#53493=CARTESIAN_POINT('Origin',(0.,0.,0.485));
#53494=CARTESIAN_POINT('Origin',(0.,0.,0.485));
#53495=CARTESIAN_POINT('Origin',(0.,0.,0.485));
#53496=CARTESIAN_POINT('Origin',(0.,0.,0.485));
#53497=CARTESIAN_POINT('Origin',(0.,0.,0.485));
#53498=CARTESIAN_POINT('Origin',(0.,0.,0.485));
#53499=CARTESIAN_POINT('',(0.424996933164776,0.00161455892897806,0.485));
#53500=CARTESIAN_POINT('Origin',(0.,0.,0.485));
#53501=CARTESIAN_POINT('',(0.424996933164776,0.00161455892897806,0.04));
#53502=CARTESIAN_POINT('',(0.424996933164776,0.00161455892897806,0.2425));
#53503=CARTESIAN_POINT('',(0.424996933164776,-0.00161455892897806,0.04));
#53504=CARTESIAN_POINT('Origin',(0.,0.,0.04));
#53505=CARTESIAN_POINT('',(0.424996933164776,-0.00161455892897806,0.485));
#53506=CARTESIAN_POINT('',(0.424996933164776,-0.00161455892897806,0.2425));
#53507=CARTESIAN_POINT('Origin',(0.,0.,0.485));
#53508=CARTESIAN_POINT('Origin',(0.419,0.,0.04));
#53509=CARTESIAN_POINT('',(0.419,8.67361737988404E-19,0.04));
#53510=CARTESIAN_POINT('',(0.419,0.,0.04));
#53511=CARTESIAN_POINT('',(0.419,8.67361737988404E-19,0.491));
#53512=CARTESIAN_POINT('',(0.419,8.67361737988404E-19,0.04));
#53513=CARTESIAN_POINT('Ctrl Pts',(0.424996933164776,-0.00161455892897809,
0.485));
#53514=CARTESIAN_POINT('Ctrl Pts',(0.421977150469257,-0.000801540510953786,
0.488022849530743));
#53515=CARTESIAN_POINT('Ctrl Pts',(0.419,8.67361737988404E-19,0.491));
#53516=CARTESIAN_POINT('Origin',(0.445,0.007,0.04));
#53517=CARTESIAN_POINT('Ctrl Pts',(0.419,8.67361737988404E-19,0.491));
#53518=CARTESIAN_POINT('Ctrl Pts',(0.421977150469257,0.000801540510953795,
0.488022849530743));
#53519=CARTESIAN_POINT('Ctrl Pts',(0.424996933164776,0.00161455892897809,
0.485));
#53520=CARTESIAN_POINT('',(0.445,0.007,0.04));
#53521=CARTESIAN_POINT('Origin',(0.432,0.,0.04));
#53522=CARTESIAN_POINT('Origin',(0.,0.,0.4925));
#53523=CARTESIAN_POINT('',(-0.41,-5.02105187650415E-17,0.5));
#53524=CARTESIAN_POINT('Origin',(0.,0.,0.5));
#53525=CARTESIAN_POINT('',(-0.4175,-5.1129003864402E-17,0.4925));
#53526=CARTESIAN_POINT('Origin',(0.,0.,0.192764973081037));
#53527=CARTESIAN_POINT('',(0.,0.,0.134529946162075));
#53528=CARTESIAN_POINT('',(-0.183165823577449,2.24313439557311E-17,0.25));
#53529=CARTESIAN_POINT('',(-0.0923760430703401,-1.1312802546399E-17,0.192764973081037));
#53530=CARTESIAN_POINT('Origin',(0.,0.,0.25));
#53531=CARTESIAN_POINT('Origin',(2.77555756156289E-17,0.23094010767585,
0.5));
#53532=CARTESIAN_POINT('',(1.41410031829988E-17,0.23094010767585,0.5));
#53533=CARTESIAN_POINT('',(0.2,0.115470053837925,0.5));
#53534=CARTESIAN_POINT('',(0.05,0.202072594216369,0.5));
#53535=CARTESIAN_POINT('',(2.77555756156289E-17,0.23094010767585,0.25));
#53536=CARTESIAN_POINT('',(1.41410031829988E-17,0.23094010767585,0.5));
#53537=CARTESIAN_POINT('',(0.2,0.115470053837925,0.25));
#53538=CARTESIAN_POINT('',(0.2,0.115470053837925,0.25));
#53539=CARTESIAN_POINT('',(0.2,0.115470053837925,0.5));
#53540=CARTESIAN_POINT('Origin',(-0.2,0.115470053837925,0.5));
#53541=CARTESIAN_POINT('',(-0.2,0.115470053837925,0.5));
#53542=CARTESIAN_POINT('',(-0.15,0.144337567297406,0.5));
#53543=CARTESIAN_POINT('',(-0.2,0.115470053837925,0.25));
#53544=CARTESIAN_POINT('',(-0.2,0.115470053837925,0.5));
#53545=CARTESIAN_POINT('',(1.41410031829988E-17,0.23094010767585,0.25));
#53546=CARTESIAN_POINT('Origin',(-0.2,-0.115470053837925,0.5));
#53547=CARTESIAN_POINT('',(-0.2,-0.115470053837925,0.5));
#53548=CARTESIAN_POINT('',(-0.2,-0.0577350269189626,0.5));
#53549=CARTESIAN_POINT('',(-0.2,-0.115470053837925,0.25));
#53550=CARTESIAN_POINT('',(-0.2,-0.115470053837925,0.5));
#53551=CARTESIAN_POINT('',(-0.2,0.115470053837925,0.25));
#53552=CARTESIAN_POINT('Origin',(-5.55111512312578E-17,-0.23094010767585,
0.5));
#53553=CARTESIAN_POINT('',(-4.24230095489963E-17,-0.23094010767585,0.5));
#53554=CARTESIAN_POINT('',(-0.0500000000000001,-0.202072594216369,0.5));
#53555=CARTESIAN_POINT('',(-5.55111512312578E-17,-0.23094010767585,0.25));
#53556=CARTESIAN_POINT('',(-4.24230095489963E-17,-0.23094010767585,0.5));
#53557=CARTESIAN_POINT('',(-0.2,-0.115470053837925,0.25));
#53558=CARTESIAN_POINT('Origin',(0.2,-0.115470053837925,0.5));
#53559=CARTESIAN_POINT('',(0.2,-0.115470053837925,0.5));
#53560=CARTESIAN_POINT('',(0.15,-0.144337567297407,0.5));
#53561=CARTESIAN_POINT('',(0.2,-0.115470053837925,0.25));
#53562=CARTESIAN_POINT('',(0.2,-0.115470053837925,0.5));
#53563=CARTESIAN_POINT('',(-4.24230095489963E-17,-0.23094010767585,0.25));
#53564=CARTESIAN_POINT('Origin',(0.2,0.115470053837925,0.5));
#53565=CARTESIAN_POINT('',(0.2,0.0577350269189625,0.5));
#53566=CARTESIAN_POINT('',(0.2,-0.115470053837925,0.25));
#53567=CARTESIAN_POINT('Origin',(0.,0.,0.25));
#53568=CARTESIAN_POINT('Origin',(0.19,0.,-1.6));
#53569=CARTESIAN_POINT('',(-0.19,-2.32682891837997E-17,-1.6));
#53570=CARTESIAN_POINT('Origin',(0.,0.,-1.6));
#53571=CARTESIAN_POINT('Origin',(0.,0.,-1.57));
#53572=CARTESIAN_POINT('',(-0.22,-2.69422295812418E-17,-1.57));
#53573=CARTESIAN_POINT('Origin',(0.,0.,-0.775));
#53574=CARTESIAN_POINT('Origin',(0.,0.,-0.0149499999999999));
#53575=CARTESIAN_POINT('Origin',(0.,0.,-0.005));
#53576=CARTESIAN_POINT('',(-0.26,-3.18408167778312E-17,-2.60208521396521E-18));
#53577=CARTESIAN_POINT('Origin',(0.,0.,0.));
#53578=CARTESIAN_POINT('',(-0.255,-3.12284933782575E-17,-0.005));
#53579=CARTESIAN_POINT('Origin',(0.425,0.,0.));
#53580=CARTESIAN_POINT('Origin',(0.,0.,0.5));
#53581=CARTESIAN_POINT('',(0.,0.,0.));
#53582=CARTESIAN_POINT('',(0.,0.,0.));
#53583=CARTESIAN_POINT('',(0.,0.,0.));
#53584=CARTESIAN_POINT('',(0.,1.4,8.5));
#53585=CARTESIAN_POINT('',(0.,-2.3,8.5));
#53586=CARTESIAN_POINT('',(2.69422295812418E-16,0.,12.9));
#53587=CARTESIAN_POINT('',(4.63323591024675,-1.55,11.175));
#53588=CARTESIAN_POINT('',(0.,-2.2,8.5));
#53589=CARTESIAN_POINT('',(0.,-3.4,8.5));
#53590=CARTESIAN_POINT('',(3.25269119345812,-3.7,11.7526911934581));
#53591=CARTESIAN_POINT('',(3.25269119345812,-3.76,11.7526911934581));
#53592=CARTESIAN_POINT('',(0.,3.2,8.5));
#53593=CARTESIAN_POINT('',(3.5,2.3,16.2));
#53594=CARTESIAN_POINT('',(4.4,3.6,8.5));
#53595=CARTESIAN_POINT('',(2.2,3.6,12.3105117766515));
#53596=CARTESIAN_POINT('',(-4.5,2.3,0.55));
#53597=CARTESIAN_POINT('',(0.,2.,8.5));
#53598=CARTESIAN_POINT('',(-3.81051177665153,0.,6.3));
#53599=CARTESIAN_POINT('',(3.81051177665153,0.,6.3));
#53600=CARTESIAN_POINT('',(-4.63323591024675,-1.55,11.175));
#53601=CARTESIAN_POINT('',(-9.82779056315751E-16,-1.55,3.15));
#53602=CARTESIAN_POINT('',(0.,1.9,8.5));
#53603=CARTESIAN_POINT('',(0.,-3.4,8.5));
#53604=CARTESIAN_POINT('',(0.,-3.4,8.5));
#53605=CARTESIAN_POINT('',(-3.25269119345812,-3.7,11.7526911934581));
#53606=CARTESIAN_POINT('',(-8.45006291411674E-16,-3.7,3.9));
#53607=CARTESIAN_POINT('',(-3.25269119345812,-3.76,11.7526911934581));
#53608=CARTESIAN_POINT('',(-8.45006291411674E-16,-3.76,3.9));
#53609=CARTESIAN_POINT('',(-2.2,3.6,12.3105117766515));
#53610=CARTESIAN_POINT('',(-2.2,3.6,4.68948822334847));
#53611=CARTESIAN_POINT('',(-4.4,3.6,8.5));
#53612=CARTESIAN_POINT('',(2.2,3.6,4.68948822334847));
#53613=CARTESIAN_POINT('',(0.,2.3,0.55));
#53614=CARTESIAN_POINT('',(4.5,2.3,0.55));
#53615=UNCERTAINTY_MEASURE_WITH_UNIT(LENGTH_MEASURE(0.001),#53651,
'DISTANCE_ACCURACY_VALUE',
'Maximum model space distance between geometric entities at asserted c
onnectivities');
#53616=UNCERTAINTY_MEASURE_WITH_UNIT(LENGTH_MEASURE(0.001),#53651,
'DISTANCE_ACCURACY_VALUE',
'Maximum model space distance between geometric entities at asserted c
onnectivities');
#53617=UNCERTAINTY_MEASURE_WITH_UNIT(LENGTH_MEASURE(0.001),#53651,
'DISTANCE_ACCURACY_VALUE',
'Maximum model space distance between geometric entities at asserted c
onnectivities');
#53618=UNCERTAINTY_MEASURE_WITH_UNIT(LENGTH_MEASURE(0.001),#53651,
'DISTANCE_ACCURACY_VALUE',
'Maximum model space distance between geometric entities at asserted c
onnectivities');
#53619=UNCERTAINTY_MEASURE_WITH_UNIT(LENGTH_MEASURE(0.001),#53651,
'DISTANCE_ACCURACY_VALUE',
'Maximum model space distance between geometric entities at asserted c
onnectivities');
#53620=UNCERTAINTY_MEASURE_WITH_UNIT(LENGTH_MEASURE(0.001),#53651,
'DISTANCE_ACCURACY_VALUE',
'Maximum model space distance between geometric entities at asserted c
onnectivities');
#53621=UNCERTAINTY_MEASURE_WITH_UNIT(LENGTH_MEASURE(0.001),#53651,
'DISTANCE_ACCURACY_VALUE',
'Maximum model space distance between geometric entities at asserted c
onnectivities');
#53622=UNCERTAINTY_MEASURE_WITH_UNIT(LENGTH_MEASURE(0.001),#53651,
'DISTANCE_ACCURACY_VALUE',
'Maximum model space distance between geometric entities at asserted c
onnectivities');
#53623=UNCERTAINTY_MEASURE_WITH_UNIT(LENGTH_MEASURE(0.001),#53651,
'DISTANCE_ACCURACY_VALUE',
'Maximum model space distance between geometric entities at asserted c
onnectivities');
#53624=UNCERTAINTY_MEASURE_WITH_UNIT(LENGTH_MEASURE(0.001),#53651,
'DISTANCE_ACCURACY_VALUE',
'Maximum model space distance between geometric entities at asserted c
onnectivities');
#53625=UNCERTAINTY_MEASURE_WITH_UNIT(LENGTH_MEASURE(0.001),#53651,
'DISTANCE_ACCURACY_VALUE',
'Maximum model space distance between geometric entities at asserted c
onnectivities');
#53626=UNCERTAINTY_MEASURE_WITH_UNIT(LENGTH_MEASURE(0.001),#53651,
'DISTANCE_ACCURACY_VALUE',
'Maximum model space distance between geometric entities at asserted c
onnectivities');
#53627=UNCERTAINTY_MEASURE_WITH_UNIT(LENGTH_MEASURE(0.001),#53651,
'DISTANCE_ACCURACY_VALUE',
'Maximum model space distance between geometric entities at asserted c
onnectivities');
#53628=UNCERTAINTY_MEASURE_WITH_UNIT(LENGTH_MEASURE(0.001),#53651,
'DISTANCE_ACCURACY_VALUE',
'Maximum model space distance between geometric entities at asserted c
onnectivities');
#53629=UNCERTAINTY_MEASURE_WITH_UNIT(LENGTH_MEASURE(0.001),#53651,
'DISTANCE_ACCURACY_VALUE',
'Maximum model space distance between geometric entities at asserted c
onnectivities');
#53630=UNCERTAINTY_MEASURE_WITH_UNIT(LENGTH_MEASURE(0.001),#53651,
'DISTANCE_ACCURACY_VALUE',
'Maximum model space distance between geometric entities at asserted c
onnectivities');
#53631=UNCERTAINTY_MEASURE_WITH_UNIT(LENGTH_MEASURE(0.001),#53651,
'DISTANCE_ACCURACY_VALUE',
'Maximum model space distance between geometric entities at asserted c
onnectivities');
#53632=UNCERTAINTY_MEASURE_WITH_UNIT(LENGTH_MEASURE(0.001),#53651,
'DISTANCE_ACCURACY_VALUE',
'Maximum model space distance between geometric entities at asserted c
onnectivities');
#53633=(
GEOMETRIC_REPRESENTATION_CONTEXT(3)
GLOBAL_UNCERTAINTY_ASSIGNED_CONTEXT((#53615))
GLOBAL_UNIT_ASSIGNED_CONTEXT((#53651,#53653,#53654))
REPRESENTATION_CONTEXT('','3D')
);
#53634=(
GEOMETRIC_REPRESENTATION_CONTEXT(3)
GLOBAL_UNCERTAINTY_ASSIGNED_CONTEXT((#53616))
GLOBAL_UNIT_ASSIGNED_CONTEXT((#53651,#53653,#53654))
REPRESENTATION_CONTEXT('','3D')
);
#53635=(
GEOMETRIC_REPRESENTATION_CONTEXT(3)
GLOBAL_UNCERTAINTY_ASSIGNED_CONTEXT((#53617))
GLOBAL_UNIT_ASSIGNED_CONTEXT((#53651,#53653,#53654))
REPRESENTATION_CONTEXT('','3D')
);
#53636=(
GEOMETRIC_REPRESENTATION_CONTEXT(3)
GLOBAL_UNCERTAINTY_ASSIGNED_CONTEXT((#53618))
GLOBAL_UNIT_ASSIGNED_CONTEXT((#53651,#53653,#53654))
REPRESENTATION_CONTEXT('','3D')
);
#53637=(
GEOMETRIC_REPRESENTATION_CONTEXT(3)
GLOBAL_UNCERTAINTY_ASSIGNED_CONTEXT((#53619))
GLOBAL_UNIT_ASSIGNED_CONTEXT((#53651,#53653,#53654))
REPRESENTATION_CONTEXT('','3D')
);
#53638=(
GEOMETRIC_REPRESENTATION_CONTEXT(3)
GLOBAL_UNCERTAINTY_ASSIGNED_CONTEXT((#53620))
GLOBAL_UNIT_ASSIGNED_CONTEXT((#53651,#53653,#53654))
REPRESENTATION_CONTEXT('','3D')
);
#53639=(
GEOMETRIC_REPRESENTATION_CONTEXT(3)
GLOBAL_UNCERTAINTY_ASSIGNED_CONTEXT((#53621))
GLOBAL_UNIT_ASSIGNED_CONTEXT((#53651,#53653,#53654))
REPRESENTATION_CONTEXT('','3D')
);
#53640=(
GEOMETRIC_REPRESENTATION_CONTEXT(3)
GLOBAL_UNCERTAINTY_ASSIGNED_CONTEXT((#53622))
GLOBAL_UNIT_ASSIGNED_CONTEXT((#53651,#53653,#53654))
REPRESENTATION_CONTEXT('','3D')
);
#53641=(
GEOMETRIC_REPRESENTATION_CONTEXT(3)
GLOBAL_UNCERTAINTY_ASSIGNED_CONTEXT((#53623))
GLOBAL_UNIT_ASSIGNED_CONTEXT((#53651,#53653,#53654))
REPRESENTATION_CONTEXT('','3D')
);
#53642=(
GEOMETRIC_REPRESENTATION_CONTEXT(3)
GLOBAL_UNCERTAINTY_ASSIGNED_CONTEXT((#53624))
GLOBAL_UNIT_ASSIGNED_CONTEXT((#53651,#53653,#53654))
REPRESENTATION_CONTEXT('','3D')
);
#53643=(
GEOMETRIC_REPRESENTATION_CONTEXT(3)
GLOBAL_UNCERTAINTY_ASSIGNED_CONTEXT((#53625))
GLOBAL_UNIT_ASSIGNED_CONTEXT((#53651,#53653,#53654))
REPRESENTATION_CONTEXT('','3D')
);
#53644=(
GEOMETRIC_REPRESENTATION_CONTEXT(3)
GLOBAL_UNCERTAINTY_ASSIGNED_CONTEXT((#53626))
GLOBAL_UNIT_ASSIGNED_CONTEXT((#53651,#53653,#53654))
REPRESENTATION_CONTEXT('','3D')
);
#53645=(
GEOMETRIC_REPRESENTATION_CONTEXT(3)
GLOBAL_UNCERTAINTY_ASSIGNED_CONTEXT((#53627))
GLOBAL_UNIT_ASSIGNED_CONTEXT((#53651,#53653,#53654))
REPRESENTATION_CONTEXT('','3D')
);
#53646=(
GEOMETRIC_REPRESENTATION_CONTEXT(3)
GLOBAL_UNCERTAINTY_ASSIGNED_CONTEXT((#53628))
GLOBAL_UNIT_ASSIGNED_CONTEXT((#53651,#53653,#53654))
REPRESENTATION_CONTEXT('','3D')
);
#53647=(
GEOMETRIC_REPRESENTATION_CONTEXT(3)
GLOBAL_UNCERTAINTY_ASSIGNED_CONTEXT((#53629))
GLOBAL_UNIT_ASSIGNED_CONTEXT((#53651,#53653,#53654))
REPRESENTATION_CONTEXT('','3D')
);
#53648=(
GEOMETRIC_REPRESENTATION_CONTEXT(3)
GLOBAL_UNCERTAINTY_ASSIGNED_CONTEXT((#53630))
GLOBAL_UNIT_ASSIGNED_CONTEXT((#53651,#53653,#53654))
REPRESENTATION_CONTEXT('','3D')
);
#53649=(
GEOMETRIC_REPRESENTATION_CONTEXT(3)
GLOBAL_UNCERTAINTY_ASSIGNED_CONTEXT((#53631))
GLOBAL_UNIT_ASSIGNED_CONTEXT((#53651,#53653,#53654))
REPRESENTATION_CONTEXT('','3D')
);
#53650=(
GEOMETRIC_REPRESENTATION_CONTEXT(3)
GLOBAL_UNCERTAINTY_ASSIGNED_CONTEXT((#53632))
GLOBAL_UNIT_ASSIGNED_CONTEXT((#53651,#53653,#53654))
REPRESENTATION_CONTEXT('','3D')
);
#53651=(
LENGTH_UNIT()
NAMED_UNIT(*)
SI_UNIT(.CENTI.,.METRE.)
);
#53652=(
LENGTH_UNIT()
NAMED_UNIT(*)
SI_UNIT($,.METRE.)
);
#53653=(
NAMED_UNIT(*)
PLANE_ANGLE_UNIT()
SI_UNIT($,.RADIAN.)
);
#53654=(
NAMED_UNIT(*)
SI_UNIT($,.STERADIAN.)
SOLID_ANGLE_UNIT()
);
#53655=SHAPE_DEFINITION_REPRESENTATION(#53672,#53723);
#53656=SHAPE_DEFINITION_REPRESENTATION(#53673,#53724);
#53657=SHAPE_DEFINITION_REPRESENTATION(#53674,#53725);
#53658=SHAPE_DEFINITION_REPRESENTATION(#53675,#53726);
#53659=SHAPE_DEFINITION_REPRESENTATION(#53676,#53727);
#53660=SHAPE_DEFINITION_REPRESENTATION(#53677,#53728);
#53661=SHAPE_DEFINITION_REPRESENTATION(#53678,#53729);
#53662=SHAPE_DEFINITION_REPRESENTATION(#53679,#53730);
#53663=SHAPE_DEFINITION_REPRESENTATION(#53680,#53731);
#53664=SHAPE_DEFINITION_REPRESENTATION(#53681,#53732);
#53665=SHAPE_DEFINITION_REPRESENTATION(#53682,#53733);
#53666=SHAPE_DEFINITION_REPRESENTATION(#53683,#53734);
#53667=SHAPE_DEFINITION_REPRESENTATION(#53684,#53735);
#53668=SHAPE_DEFINITION_REPRESENTATION(#53685,#53736);
#53669=SHAPE_DEFINITION_REPRESENTATION(#53686,#53737);
#53670=SHAPE_DEFINITION_REPRESENTATION(#53687,#53738);
#53671=SHAPE_DEFINITION_REPRESENTATION(#53688,#53739);
#53672=PRODUCT_DEFINITION_SHAPE('',$,#53741);
#53673=PRODUCT_DEFINITION_SHAPE('',$,#53742);
#53674=PRODUCT_DEFINITION_SHAPE('',$,#53743);
#53675=PRODUCT_DEFINITION_SHAPE('',$,#53744);
#53676=PRODUCT_DEFINITION_SHAPE('',$,#53745);
#53677=PRODUCT_DEFINITION_SHAPE('',$,#53746);
#53678=PRODUCT_DEFINITION_SHAPE('',$,#53747);
#53679=PRODUCT_DEFINITION_SHAPE('',$,#53748);
#53680=PRODUCT_DEFINITION_SHAPE('',$,#53749);
#53681=PRODUCT_DEFINITION_SHAPE('',$,#53750);
#53682=PRODUCT_DEFINITION_SHAPE('',$,#53751);
#53683=PRODUCT_DEFINITION_SHAPE('',$,#53752);
#53684=PRODUCT_DEFINITION_SHAPE('',$,#53753);
#53685=PRODUCT_DEFINITION_SHAPE('',$,#53754);
#53686=PRODUCT_DEFINITION_SHAPE('',$,#53755);
#53687=PRODUCT_DEFINITION_SHAPE('',$,#53756);
#53688=PRODUCT_DEFINITION_SHAPE('',$,#53757);
#53689=PRODUCT_DEFINITION_SHAPE($,$,#113);
#53690=PRODUCT_DEFINITION_SHAPE($,$,#114);
#53691=PRODUCT_DEFINITION_SHAPE($,$,#115);
#53692=PRODUCT_DEFINITION_SHAPE($,$,#116);
#53693=PRODUCT_DEFINITION_SHAPE($,$,#117);
#53694=PRODUCT_DEFINITION_SHAPE($,$,#118);
#53695=PRODUCT_DEFINITION_SHAPE($,$,#119);
#53696=PRODUCT_DEFINITION_SHAPE($,$,#120);
#53697=PRODUCT_DEFINITION_SHAPE($,$,#121);
#53698=PRODUCT_DEFINITION_SHAPE($,$,#122);
#53699=PRODUCT_DEFINITION_SHAPE($,$,#123);
#53700=PRODUCT_DEFINITION_SHAPE($,$,#124);
#53701=PRODUCT_DEFINITION_SHAPE($,$,#125);
#53702=PRODUCT_DEFINITION_SHAPE($,$,#126);
#53703=PRODUCT_DEFINITION_SHAPE($,$,#127);
#53704=PRODUCT_DEFINITION_SHAPE($,$,#128);
#53705=PRODUCT_DEFINITION_SHAPE($,$,#129);
#53706=PRODUCT_DEFINITION_SHAPE($,$,#130);
#53707=PRODUCT_DEFINITION_SHAPE($,$,#131);
#53708=PRODUCT_DEFINITION_SHAPE($,$,#132);
#53709=PRODUCT_DEFINITION_SHAPE($,$,#133);
#53710=PRODUCT_DEFINITION_SHAPE($,$,#134);
#53711=PRODUCT_DEFINITION_SHAPE($,$,#135);
#53712=PRODUCT_DEFINITION_SHAPE($,$,#136);
#53713=PRODUCT_DEFINITION_SHAPE($,$,#137);
#53714=PRODUCT_DEFINITION_SHAPE($,$,#138);
#53715=PRODUCT_DEFINITION_SHAPE($,$,#139);
#53716=PRODUCT_DEFINITION_SHAPE($,$,#140);
#53717=PRODUCT_DEFINITION_SHAPE($,$,#141);
#53718=PRODUCT_DEFINITION_SHAPE($,$,#142);
#53719=PRODUCT_DEFINITION_SHAPE($,$,#143);
#53720=PRODUCT_DEFINITION_SHAPE($,$,#144);
#53721=PRODUCT_DEFINITION_SHAPE($,$,#145);
#53722=PRODUCT_DEFINITION_SHAPE($,$,#146);
#53723=SHAPE_REPRESENTATION('',(#23496,#25620,#25621,#25622,#25623,#25624,
#25625,#25626,#25627,#25628,#25629,#25630,#25631,#25632,#25633,#25634,#25635,
#25636,#25637,#25638,#25639,#25640,#25641,#25642,#25643,#25644,#25645,#25646,
#25647,#25648,#25649,#25650,#25651,#25652,#25653),#53633);
#53724=SHAPE_REPRESENTATION('',(#23497),#53634);
#53725=SHAPE_REPRESENTATION('',(#23686),#53635);
#53726=SHAPE_REPRESENTATION('',(#23856),#53636);
#53727=SHAPE_REPRESENTATION('',(#23983),#53637);
#53728=SHAPE_REPRESENTATION('',(#24038),#53638);
#53729=SHAPE_REPRESENTATION('',(#24107),#53639);
#53730=SHAPE_REPRESENTATION('',(#24331),#53640);
#53731=SHAPE_REPRESENTATION('',(#24343),#53641);
#53732=SHAPE_REPRESENTATION('',(#24374),#53642);
#53733=SHAPE_REPRESENTATION('',(#24521),#53643);
#53734=SHAPE_REPRESENTATION('',(#24530),#53644);
#53735=SHAPE_REPRESENTATION('',(#24586),#53645);
#53736=SHAPE_REPRESENTATION('',(#24595),#53646);
#53737=SHAPE_REPRESENTATION('',(#24795),#53647);
#53738=SHAPE_REPRESENTATION('',(#25038),#53648);
#53739=SHAPE_REPRESENTATION('',(#25369),#53649);
#53740=PRODUCT_DEFINITION_CONTEXT('part definition',#53793,'design');
#53741=PRODUCT_DEFINITION('2026-10-18-22-44-22-226','MAS-298',#53758,#53740);
#53742=PRODUCT_DEFINITION('2026-10-18-22-44-24-012','01_Base_Flange',#53759,
#53740);
#53743=PRODUCT_DEFINITION('2026-10-18-22-44-26-297',
'02_Rear_Mirror_Cell_Plate',#53760,#53740);
#53744=PRODUCT_DEFINITION('2026-10-18-22-44-34-542',
'03_Front_Kinematic_Cell_Alignment_Frame',#53761,#53740);
#53745=PRODUCT_DEFINITION('2026-10-18-22-44-37-726',
'04_Invar_Low-Expansion_Spacing_Ring',#53762,#53740);
#53746=PRODUCT_DEFINITION('2026-10-18-22-44-50-492',
'12_Rear_Mirror_Retaining_Ring',#53763,#53740);
#53747=PRODUCT_DEFINITION('2026-10-18-22-44-54-812',
'13_SHV_High-Voltage_Cable_Terminal_Plug',#53764,#53740);
#53748=PRODUCT_DEFINITION('2026-10-18-22-44-39-866',
'05_Ultra-Flat_Mirror_Substrate_D75x12',#53765,#53740);
#53749=PRODUCT_DEFINITION('2026-10-18-22-44-40-399',
'06_PZT_Piezo_Actuator_Tube_OD8xID5x16',#53766,#53740);
#53750=PRODUCT_DEFINITION('2026-10-18-22-44-41-622',
'07_Capacitive_Cavity_Gap_Sensor_D8',#53767,#53740);
#53751=PRODUCT_DEFINITION('2026-10-18-22-44-43-283',
'08_Mirror_Rubber_Gasket_D75x1',#53768,#53740);
#53752=PRODUCT_DEFINITION('2026-10-18-22-44-43-794',
'09_Mirror_Retaining_Clip',#53769,#53740);
#53753=PRODUCT_DEFINITION('2026-10-18-22-44-45-955',
'10_DIN_2093_B_Belleville_Spring_8x4.2x0.4',#53770,#53740);
#53754=PRODUCT_DEFINITION('2026-10-18-22-44-46-618',
'11_Clip_Thumb_Knob_M4x12',#53771,#53740);
#53755=PRODUCT_DEFINITION('2026-10-18-22-45-05-226',
'14_ISO_4762_M3x8_A2',#53772,#53740);
#53756=PRODUCT_DEFINITION('2026-10-18-22-45-09-197',
'15_ISO_4762_M3x30_A2',#53773,#53740);
#53757=PRODUCT_DEFINITION('2026-10-18-22-45-13-086',
'16_ISO_4762_M5x16_A2',#53774,#53740);
#53758=PRODUCT_DEFINITION_FORMATION('',$,#53795);
#53759=PRODUCT_DEFINITION_FORMATION('',$,#53796);
#53760=PRODUCT_DEFINITION_FORMATION('',$,#53797);
#53761=PRODUCT_DEFINITION_FORMATION('',$,#53798);
#53762=PRODUCT_DEFINITION_FORMATION('',$,#53799);
#53763=PRODUCT_DEFINITION_FORMATION('',$,#53800);
#53764=PRODUCT_DEFINITION_FORMATION('',$,#53801);
#53765=PRODUCT_DEFINITION_FORMATION('',$,#53802);
#53766=PRODUCT_DEFINITION_FORMATION('',$,#53803);
#53767=PRODUCT_DEFINITION_FORMATION('',$,#53804);
#53768=PRODUCT_DEFINITION_FORMATION('',$,#53805);
#53769=PRODUCT_DEFINITION_FORMATION('',$,#53806);
#53770=PRODUCT_DEFINITION_FORMATION('',$,#53807);
#53771=PRODUCT_DEFINITION_FORMATION('',$,#53808);
#53772=PRODUCT_DEFINITION_FORMATION('',$,#53809);
#53773=PRODUCT_DEFINITION_FORMATION('',$,#53810);
#53774=PRODUCT_DEFINITION_FORMATION('',$,#53811);
#53775=PRODUCT_RELATED_PRODUCT_CATEGORY('MAS-298','MAS-298',(#53795));
#53776=PRODUCT_RELATED_PRODUCT_CATEGORY('01_Base_Flange',
'01_Base_Flange',(#53796));
#53777=PRODUCT_RELATED_PRODUCT_CATEGORY('02_Rear_Mirror_Cell_Plate',
'02_Rear_Mirror_Cell_Plate',(#53797));
#53778=PRODUCT_RELATED_PRODUCT_CATEGORY(
'03_Front_Kinematic_Cell_Alignment_Frame',
'03_Front_Kinematic_Cell_Alignment_Frame',(#53798));
#53779=PRODUCT_RELATED_PRODUCT_CATEGORY(
'04_Invar_Low-Expansion_Spacing_Ring',
'04_Invar_Low-Expansion_Spacing_Ring',(#53799));
#53780=PRODUCT_RELATED_PRODUCT_CATEGORY('12_Rear_Mirror_Retaining_Ring',
'12_Rear_Mirror_Retaining_Ring',(#53800));
#53781=PRODUCT_RELATED_PRODUCT_CATEGORY(
'13_SHV_High-Voltage_Cable_Terminal_Plug',
'13_SHV_High-Voltage_Cable_Terminal_Plug',(#53801));
#53782=PRODUCT_RELATED_PRODUCT_CATEGORY(
'05_Ultra-Flat_Mirror_Substrate_D75x12',
'05_Ultra-Flat_Mirror_Substrate_D75x12',(#53802));
#53783=PRODUCT_RELATED_PRODUCT_CATEGORY(
'06_PZT_Piezo_Actuator_Tube_OD8xID5x16',
'06_PZT_Piezo_Actuator_Tube_OD8xID5x16',(#53803));
#53784=PRODUCT_RELATED_PRODUCT_CATEGORY(
'07_Capacitive_Cavity_Gap_Sensor_D8',
'07_Capacitive_Cavity_Gap_Sensor_D8',(#53804));
#53785=PRODUCT_RELATED_PRODUCT_CATEGORY('08_Mirror_Rubber_Gasket_D75x1',
'08_Mirror_Rubber_Gasket_D75x1',(#53805));
#53786=PRODUCT_RELATED_PRODUCT_CATEGORY('09_Mirror_Retaining_Clip',
'09_Mirror_Retaining_Clip',(#53806));
#53787=PRODUCT_RELATED_PRODUCT_CATEGORY(
'10_DIN_2093_B_Belleville_Spring_8x4.2x0.4',
'10_DIN_2093_B_Belleville_Spring_8x4.2x0.4',(#53807));
#53788=PRODUCT_RELATED_PRODUCT_CATEGORY('11_Clip_Thumb_Knob_M4x12',
'11_Clip_Thumb_Knob_M4x12',(#53808));
#53789=PRODUCT_RELATED_PRODUCT_CATEGORY('14_ISO_4762_M3x8_A2',
'14_ISO_4762_M3x8_A2',(#53809));
#53790=PRODUCT_RELATED_PRODUCT_CATEGORY('15_ISO_4762_M3x30_A2',
'15_ISO_4762_M3x30_A2',(#53810));
#53791=PRODUCT_RELATED_PRODUCT_CATEGORY('16_ISO_4762_M5x16_A2',
'16_ISO_4762_M5x16_A2',(#53811));
#53792=APPLICATION_PROTOCOL_DEFINITION('international standard',
'automotive_design',2009,#53793);
#53793=APPLICATION_CONTEXT(
'Core Data for Automotive Mechanical Design Process');
#53794=PRODUCT_CONTEXT('part definition',#53793,'mechanical');
#53795=PRODUCT('2026-10-18-22-44-22-226','MAS-298',$,(#53794));
#53796=PRODUCT('2026-10-18-22-44-24-012','01_Base_Flange',$,(#53794));
#53797=PRODUCT('2026-10-18-22-44-26-297','02_Rear_Mirror_Cell_Plate',$,
(#53794));
#53798=PRODUCT('2026-10-18-22-44-34-542',
'03_Front_Kinematic_Cell_Alignment_Frame',$,(#53794));
#53799=PRODUCT('2026-10-18-22-44-37-726',
'04_Invar_Low-Expansion_Spacing_Ring',$,(#53794));
#53800=PRODUCT('2026-10-18-22-44-50-492',
'12_Rear_Mirror_Retaining_Ring',$,(#53794));
#53801=PRODUCT('2026-10-18-22-44-54-812',
'13_SHV_High-Voltage_Cable_Terminal_Plug',$,(#53794));
#53802=PRODUCT('2026-10-18-22-44-39-866',
'05_Ultra-Flat_Mirror_Substrate_D75x12',$,(#53794));
#53803=PRODUCT('2026-10-18-22-44-40-399',
'06_PZT_Piezo_Actuator_Tube_OD8xID5x16',$,(#53794));
#53804=PRODUCT('2026-10-18-22-44-41-622',
'07_Capacitive_Cavity_Gap_Sensor_D8',$,(#53794));
#53805=PRODUCT('2026-10-18-22-44-43-283',
'08_Mirror_Rubber_Gasket_D75x1',$,(#53794));
#53806=PRODUCT('2026-10-18-22-44-43-794','09_Mirror_Retaining_Clip',$,(#53794));
#53807=PRODUCT('2026-10-18-22-44-45-955',
'10_DIN_2093_B_Belleville_Spring_8x4.2x0.4',$,(#53794));
#53808=PRODUCT('2026-10-18-22-44-46-618','11_Clip_Thumb_Knob_M4x12',$,(#53794));
#53809=PRODUCT('2026-10-18-22-45-05-226','14_ISO_4762_M3x8_A2',$,(#53794));
#53810=PRODUCT('2026-10-18-22-45-09-197','15_ISO_4762_M3x30_A2',$,(#53794));
#53811=PRODUCT('2026-10-18-22-45-13-086','16_ISO_4762_M5x16_A2',$,(#53794));
#53812=PRESENTATION_STYLE_ASSIGNMENT((#53829));
#53813=PRESENTATION_STYLE_ASSIGNMENT((#53830));
#53814=PRESENTATION_STYLE_ASSIGNMENT((#53831));
#53815=PRESENTATION_STYLE_ASSIGNMENT((#53832));
#53816=PRESENTATION_STYLE_ASSIGNMENT((#53833));
#53817=PRESENTATION_STYLE_ASSIGNMENT((#53834));
#53818=PRESENTATION_STYLE_ASSIGNMENT((#53835));
#53819=PRESENTATION_STYLE_ASSIGNMENT((#53836));
#53820=PRESENTATION_STYLE_ASSIGNMENT((#53837));
#53821=PRESENTATION_STYLE_ASSIGNMENT((#53838));
#53822=PRESENTATION_STYLE_ASSIGNMENT((#53839));
#53823=PRESENTATION_STYLE_ASSIGNMENT((#53840));
#53824=PRESENTATION_STYLE_ASSIGNMENT((#53841));
#53825=PRESENTATION_STYLE_ASSIGNMENT((#53842));
#53826=PRESENTATION_STYLE_ASSIGNMENT((#53843));
#53827=PRESENTATION_STYLE_ASSIGNMENT((#53844));
#53828=PRESENTATION_STYLE_ASSIGNMENT((#53845));
#53829=SURFACE_STYLE_USAGE(.BOTH.,#53846);
#53830=SURFACE_STYLE_USAGE(.BOTH.,#53847);
#53831=SURFACE_STYLE_USAGE(.BOTH.,#53848);
#53832=SURFACE_STYLE_USAGE(.BOTH.,#53849);
#53833=SURFACE_STYLE_USAGE(.BOTH.,#53850);
#53834=SURFACE_STYLE_USAGE(.BOTH.,#53851);
#53835=SURFACE_STYLE_USAGE(.BOTH.,#53852);
#53836=SURFACE_STYLE_USAGE(.BOTH.,#53853);
#53837=SURFACE_STYLE_USAGE(.BOTH.,#53854);
#53838=SURFACE_STYLE_USAGE(.BOTH.,#53855);
#53839=SURFACE_STYLE_USAGE(.BOTH.,#53856);
#53840=SURFACE_STYLE_USAGE(.BOTH.,#53857);
#53841=SURFACE_STYLE_USAGE(.BOTH.,#53858);
#53842=SURFACE_STYLE_USAGE(.BOTH.,#53859);
#53843=SURFACE_STYLE_USAGE(.BOTH.,#53860);
#53844=SURFACE_STYLE_USAGE(.BOTH.,#53861);
#53845=SURFACE_STYLE_USAGE(.BOTH.,#53862);
#53846=SURFACE_SIDE_STYLE('',(#53863));
#53847=SURFACE_SIDE_STYLE('',(#53864));
#53848=SURFACE_SIDE_STYLE('',(#53865));
#53849=SURFACE_SIDE_STYLE('',(#53866));
#53850=SURFACE_SIDE_STYLE('',(#53867));
#53851=SURFACE_SIDE_STYLE('',(#53868));
#53852=SURFACE_SIDE_STYLE('',(#53869));
#53853=SURFACE_SIDE_STYLE('',(#53870));
#53854=SURFACE_SIDE_STYLE('',(#53871));
#53855=SURFACE_SIDE_STYLE('',(#53872));
#53856=SURFACE_SIDE_STYLE('',(#53873));
#53857=SURFACE_SIDE_STYLE('',(#53874));
#53858=SURFACE_SIDE_STYLE('',(#53875));
#53859=SURFACE_SIDE_STYLE('',(#53876));
#53860=SURFACE_SIDE_STYLE('',(#53877));
#53861=SURFACE_SIDE_STYLE('',(#53878));
#53862=SURFACE_SIDE_STYLE('',(#53879));
#53863=SURFACE_STYLE_FILL_AREA(#53880);
#53864=SURFACE_STYLE_FILL_AREA(#53881);
#53865=SURFACE_STYLE_FILL_AREA(#53882);
#53866=SURFACE_STYLE_FILL_AREA(#53883);
#53867=SURFACE_STYLE_FILL_AREA(#53884);
#53868=SURFACE_STYLE_FILL_AREA(#53885);
#53869=SURFACE_STYLE_FILL_AREA(#53886);
#53870=SURFACE_STYLE_FILL_AREA(#53887);
#53871=SURFACE_STYLE_FILL_AREA(#53888);
#53872=SURFACE_STYLE_FILL_AREA(#53889);
#53873=SURFACE_STYLE_FILL_AREA(#53890);
#53874=SURFACE_STYLE_FILL_AREA(#53891);
#53875=SURFACE_STYLE_FILL_AREA(#53892);
#53876=SURFACE_STYLE_FILL_AREA(#53893);
#53877=SURFACE_STYLE_FILL_AREA(#53894);
#53878=SURFACE_STYLE_FILL_AREA(#53895);
#53879=SURFACE_STYLE_FILL_AREA(#53896);
#53880=FILL_AREA_STYLE('Steel - Satin',(#53897));
#53881=FILL_AREA_STYLE('MAS298_01',(#53898));
#53882=FILL_AREA_STYLE('MAS298_02',(#53899));
#53883=FILL_AREA_STYLE('MAS298_03',(#53900));
#53884=FILL_AREA_STYLE('MAS298_04',(#53901));
#53885=FILL_AREA_STYLE('MAS298_12',(#53902));
#53886=FILL_AREA_STYLE('MAS298_13',(#53903));
#53887=FILL_AREA_STYLE('MAS298_05',(#53904));
#53888=FILL_AREA_STYLE('MAS298_06',(#53905));
#53889=FILL_AREA_STYLE('MAS298_07',(#53906));
#53890=FILL_AREA_STYLE('MAS298_08',(#53907));
#53891=FILL_AREA_STYLE('MAS298_09',(#53908));
#53892=FILL_AREA_STYLE('MAS298_10',(#53909));
#53893=FILL_AREA_STYLE('MAS298_11',(#53910));
#53894=FILL_AREA_STYLE('MAS298_14',(#53911));
#53895=FILL_AREA_STYLE('MAS298_15',(#53912));
#53896=FILL_AREA_STYLE('MAS298_16',(#53913));
#53897=FILL_AREA_STYLE_COLOUR('Steel - Satin',#53914);
#53898=FILL_AREA_STYLE_COLOUR('MAS298_01',#53915);
#53899=FILL_AREA_STYLE_COLOUR('MAS298_02',#53916);
#53900=FILL_AREA_STYLE_COLOUR('MAS298_03',#53917);
#53901=FILL_AREA_STYLE_COLOUR('MAS298_04',#53918);
#53902=FILL_AREA_STYLE_COLOUR('MAS298_12',#53919);
#53903=FILL_AREA_STYLE_COLOUR('MAS298_13',#53920);
#53904=FILL_AREA_STYLE_COLOUR('MAS298_05',#53921);
#53905=FILL_AREA_STYLE_COLOUR('MAS298_06',#53922);
#53906=FILL_AREA_STYLE_COLOUR('MAS298_07',#53923);
#53907=FILL_AREA_STYLE_COLOUR('MAS298_08',#53924);
#53908=FILL_AREA_STYLE_COLOUR('MAS298_09',#53925);
#53909=FILL_AREA_STYLE_COLOUR('MAS298_10',#53926);
#53910=FILL_AREA_STYLE_COLOUR('MAS298_11',#53927);
#53911=FILL_AREA_STYLE_COLOUR('MAS298_14',#53928);
#53912=FILL_AREA_STYLE_COLOUR('MAS298_15',#53929);
#53913=FILL_AREA_STYLE_COLOUR('MAS298_16',#53930);
#53914=COLOUR_RGB('Steel - Satin',0.627450980392157,0.627450980392157,0.627450980392157);
#53915=COLOUR_RGB('MAS298_01',0.129411764705882,0.129411764705882,0.141176470588235);
#53916=COLOUR_RGB('MAS298_02',0.117647058823529,0.117647058823529,0.129411764705882);
#53917=COLOUR_RGB('MAS298_03',0.141176470588235,0.141176470588235,0.152941176470588);
#53918=COLOUR_RGB('MAS298_04',0.690196078431373,0.705882352941177,0.729411764705882);
#53919=COLOUR_RGB('MAS298_12',0.125490196078431,0.125490196078431,0.137254901960784);
#53920=COLOUR_RGB('MAS298_13',0.831372549019608,0.83921568627451,0.854901960784314);
#53921=COLOUR_RGB('MAS298_05',0.925490196078431,0.929411764705882,0.937254901960784);
#53922=COLOUR_RGB('MAS298_06',0.886274509803922,0.870588235294118,0.823529411764706);
#53923=COLOUR_RGB('MAS298_07',0.807843137254902,0.819607843137255,0.83921568627451);
#53924=COLOUR_RGB('MAS298_08',0.101960784313725,0.101960784313725,0.109803921568627);
#53925=COLOUR_RGB('MAS298_09',0.815686274509804,0.827450980392157,0.847058823529412);
#53926=COLOUR_RGB('MAS298_10',0.784313725490196,0.796078431372549,0.815686274509804);
#53927=COLOUR_RGB('MAS298_11',0.109803921568627,0.109803921568627,0.117647058823529);
#53928=COLOUR_RGB('MAS298_14',0.776470588235294,0.792156862745098,0.815686274509804);
#53929=COLOUR_RGB('MAS298_15',0.784313725490196,0.8,0.823529411764706);
#53930=COLOUR_RGB('MAS298_16',0.792156862745098,0.807843137254902,0.827450980392157);
#53931=COLOUR_RGB('Dark Blue',0.08,0.2,0.34);
#53932=FILL_AREA_STYLE_COLOUR('',#53931);
#53933=FILL_AREA_STYLE('',(#53932));
#53934=SURFACE_STYLE_FILL_AREA(#53933);
#53935=SURFACE_SIDE_STYLE('',(#53934));
#53936=SURFACE_STYLE_USAGE(.BOTH.,#53935);
#53937=PRESENTATION_STYLE_ASSIGNMENT((#53936));
#53938=COLOUR_RGB('Light Blue',0.38,0.62,0.78);
#53939=FILL_AREA_STYLE_COLOUR('',#53938);
#53940=FILL_AREA_STYLE('',(#53939));
#53941=SURFACE_STYLE_FILL_AREA(#53940);
#53942=SURFACE_SIDE_STYLE('',(#53941));
#53943=SURFACE_STYLE_USAGE(.BOTH.,#53942);
#53944=PRESENTATION_STYLE_ASSIGNMENT((#53943));
#53945=COLOUR_RGB('Sky Blue',0.24,0.69,0.87);
#53946=FILL_AREA_STYLE_COLOUR('',#53945);
#53947=FILL_AREA_STYLE('',(#53946));
#53948=SURFACE_STYLE_FILL_AREA(#53947);
#53949=SURFACE_SIDE_STYLE('',(#53948));
#53950=SURFACE_STYLE_USAGE(.BOTH.,#53949);
#53951=PRESENTATION_STYLE_ASSIGNMENT((#53950));
#53952=COLOUR_RGB('Grey',0.48,0.52,0.57);
#53953=FILL_AREA_STYLE_COLOUR('',#53952);
#53954=FILL_AREA_STYLE('',(#53953));
#53955=SURFACE_STYLE_FILL_AREA(#53954);
#53956=SURFACE_SIDE_STYLE('',(#53955));
#53957=SURFACE_STYLE_USAGE(.BOTH.,#53956);
#53958=PRESENTATION_STYLE_ASSIGNMENT((#53957));
#53959=COLOUR_RGB('Black',0.12,0.14,0.17);
#53960=FILL_AREA_STYLE_COLOUR('',#53959);
#53961=FILL_AREA_STYLE('',(#53960));
#53962=SURFACE_STYLE_FILL_AREA(#53961);
#53963=SURFACE_SIDE_STYLE('',(#53962));
#53964=SURFACE_STYLE_USAGE(.BOTH.,#53963);
#53965=PRESENTATION_STYLE_ASSIGNMENT((#53964));
#53966=COLOUR_RGB('Off White',0.89,0.88,0.83);
#53967=FILL_AREA_STYLE_COLOUR('',#53966);
#53968=FILL_AREA_STYLE('',(#53967));
#53969=SURFACE_STYLE_FILL_AREA(#53968);
#53970=SURFACE_SIDE_STYLE('',(#53969));
#53971=SURFACE_STYLE_USAGE(.BOTH.,#53970);
#53972=PRESENTATION_STYLE_ASSIGNMENT((#53971));
ENDSEC;
END-ISO-10303-21;
